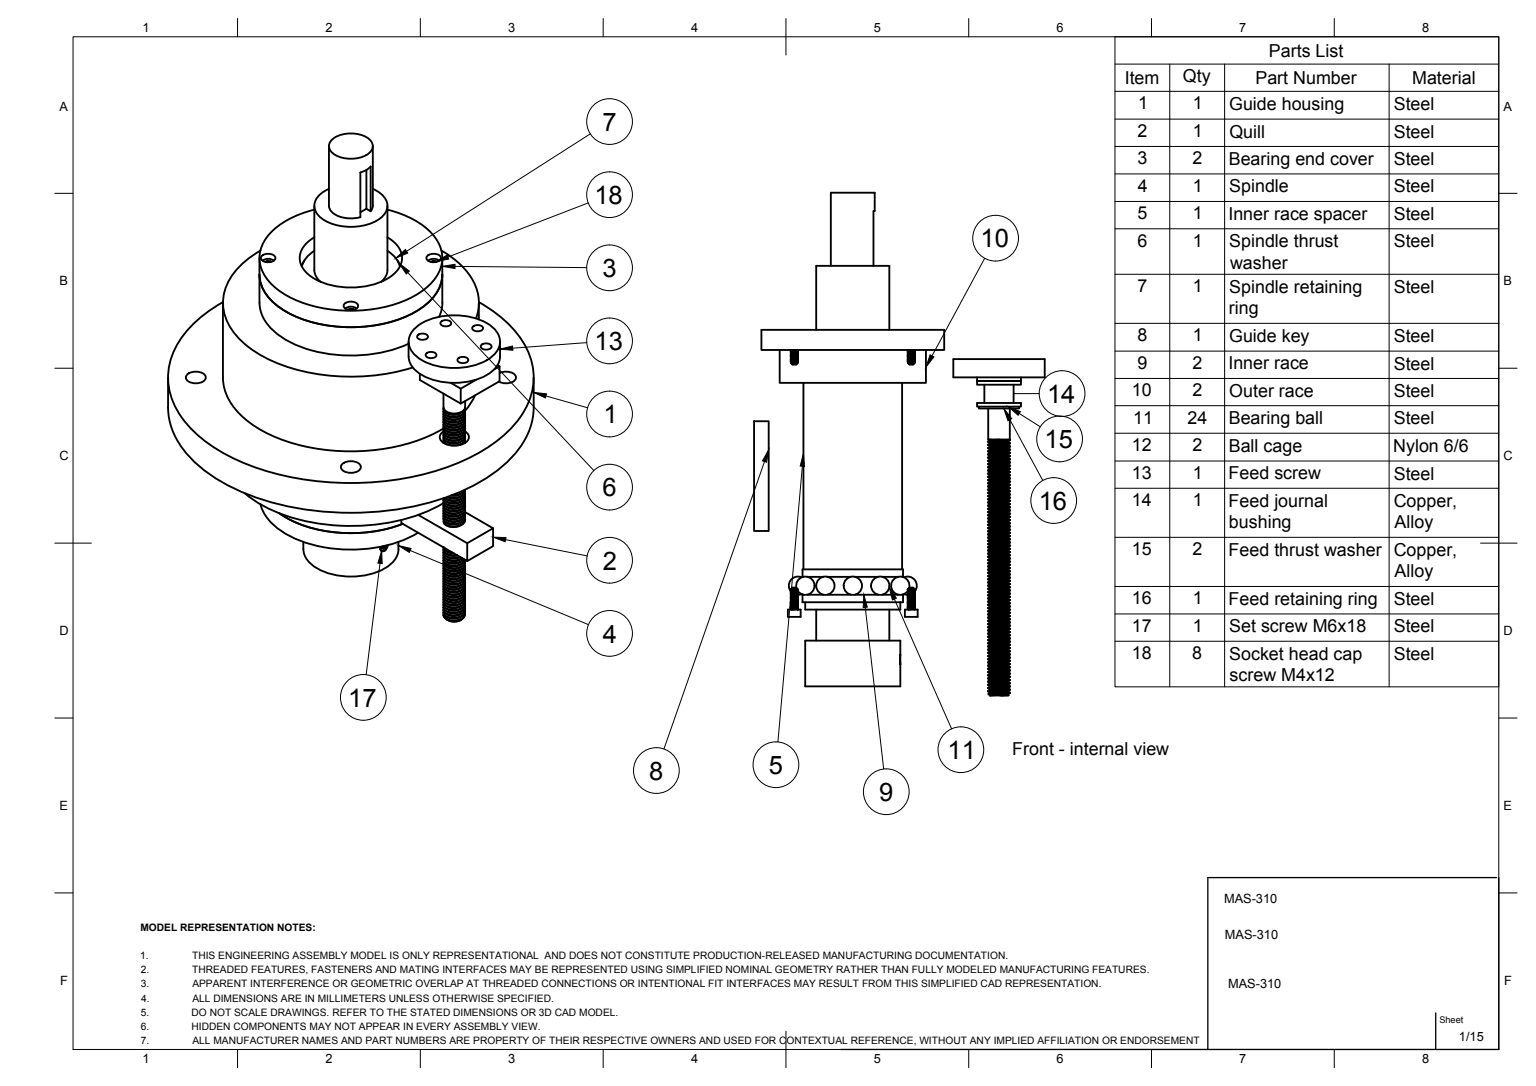
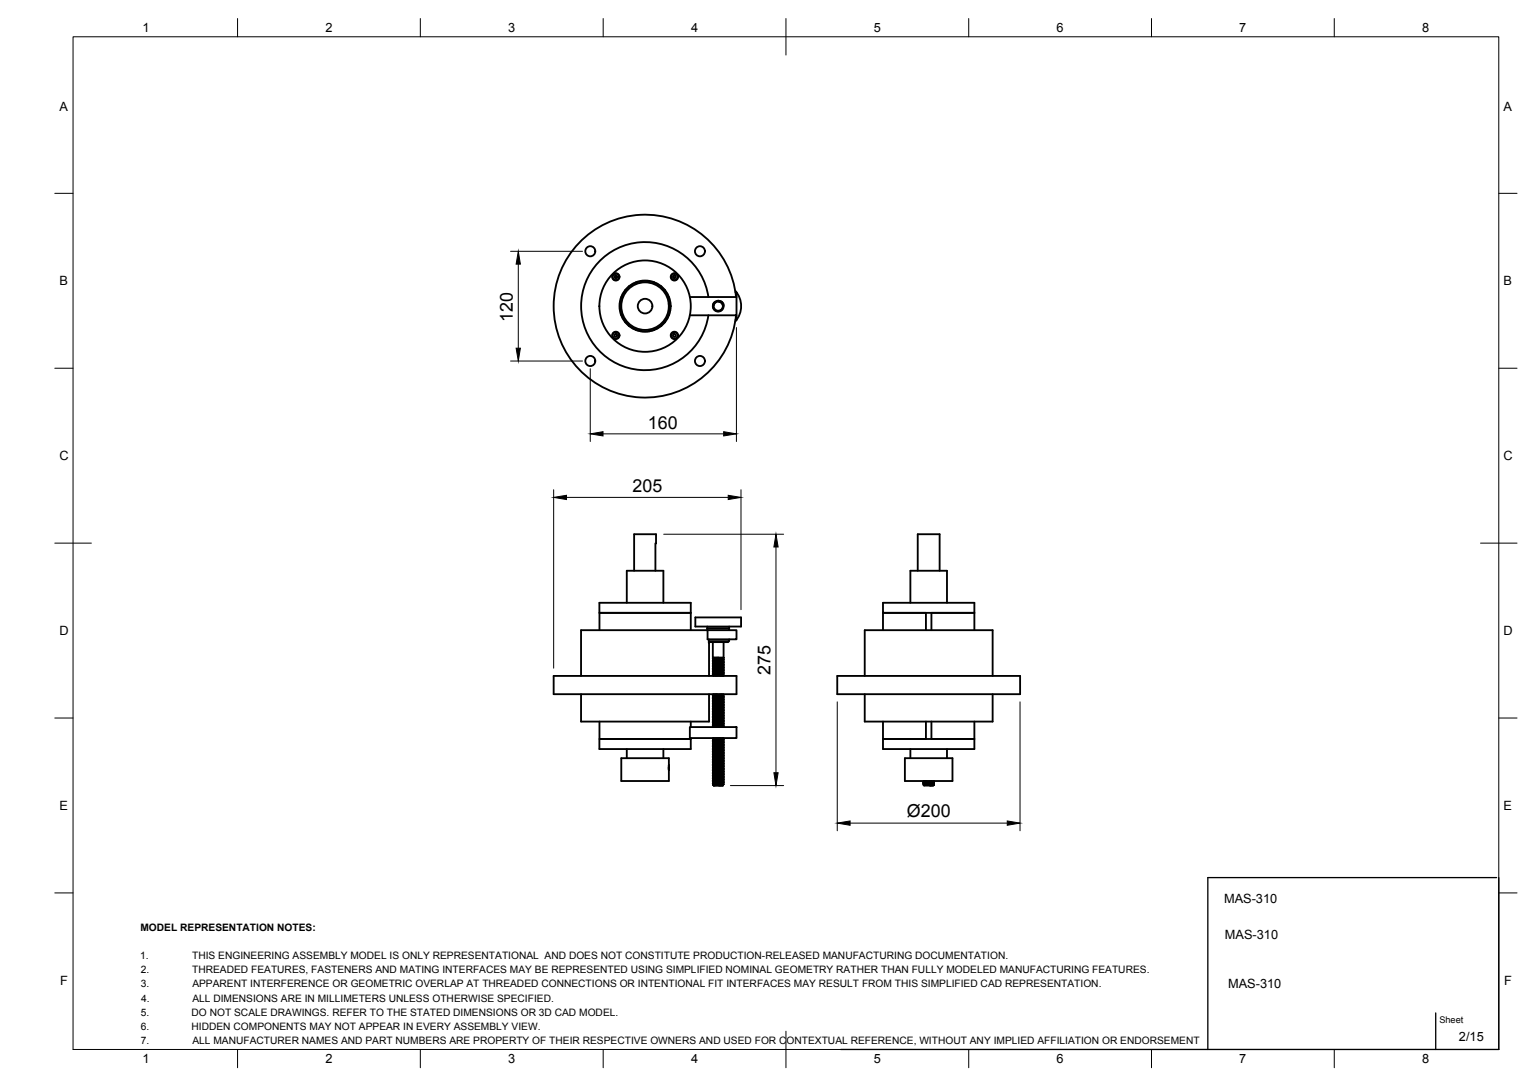
ISO-10303-21;
HEADER;
/* Generated by software containing ST-Developer
 * from STEP Tools, Inc. (www.steptools.com) 
 */

FILE_DESCRIPTION(
/* description */ ('Independent30mm screw-fed quill/spindle unit with16mm straight tool s
ocket, radial set screw, native reusable open ball bearings, retained 
inner/outer race stacks, keyed quill guide and M12x1.75 fine feed. Ext
ernal moving drive and tool not included. Ideal cage orbital links; in
dividual ball spin, force and preload not simulated. No drilling capac
ity, runout, speed, torque, load, life or machine safety rating.'),
/* implementation_level */ '2;1');

FILE_NAME(
/* name */ 'MAS-310.step',
/* time_stamp */ '2026-11-08T18:59:42-08:00',
/* author */ (''),
/* organization */ (''),
/* preprocessor_version */ 'ST-DEVELOPER v20.2',
/* originating_system */ 'Autodesk Translation Framework v15.17.0.0',
/* authorisation */ '');

FILE_SCHEMA (('AUTOMOTIVE_DESIGN { 1 0 10303 214 3 1 1 }'));
ENDSEC;

DATA;
#10=MECHANICAL_DESIGN_GEOMETRIC_PRESENTATION_REPRESENTATION('',(#1592,#1593,
#1594,#1595,#1596,#1597,#1598,#1599,#1600,#1601,#1602,#1603,#1604,#1605,
#1606,#1607,#1608,#1609),#63898);
#11=ITEM_DEFINED_TRANSFORMATION($,$,#15696,#16806);
#12=ITEM_DEFINED_TRANSFORMATION($,$,#15752,#16807);
#13=ITEM_DEFINED_TRANSFORMATION($,$,#16583,#16808);
#14=ITEM_DEFINED_TRANSFORMATION($,$,#16184,#16809);
#15=ITEM_DEFINED_TRANSFORMATION($,$,#16268,#16810);
#16=ITEM_DEFINED_TRANSFORMATION($,$,#16277,#16811);
#17=ITEM_DEFINED_TRANSFORMATION($,$,#16286,#16812);
#18=ITEM_DEFINED_TRANSFORMATION($,$,#16297,#16813);
#19=ITEM_DEFINED_TRANSFORMATION($,$,#16620,#16814);
#20=ITEM_DEFINED_TRANSFORMATION($,$,#16634,#16815);
#21=ITEM_DEFINED_TRANSFORMATION($,$,#16648,#16816);
#22=ITEM_DEFINED_TRANSFORMATION($,$,#16651,#16817);
#23=ITEM_DEFINED_TRANSFORMATION($,$,#16304,#16818);
#24=ITEM_DEFINED_TRANSFORMATION($,$,#16511,#16819);
#25=ITEM_DEFINED_TRANSFORMATION($,$,#16743,#16820);
#26=ITEM_DEFINED_TRANSFORMATION($,$,#16520,#16821);
#27=ITEM_DEFINED_TRANSFORMATION($,$,#16531,#16822);
#28=ITEM_DEFINED_TRANSFORMATION($,$,#16752,#16823);
#29=ITEM_DEFINED_TRANSFORMATION($,$,#16583,#16824);
#30=ITEM_DEFINED_TRANSFORMATION($,$,#16648,#16825);
#31=ITEM_DEFINED_TRANSFORMATION($,$,#16648,#16826);
#32=ITEM_DEFINED_TRANSFORMATION($,$,#16648,#16827);
#33=ITEM_DEFINED_TRANSFORMATION($,$,#16648,#16828);
#34=ITEM_DEFINED_TRANSFORMATION($,$,#16648,#16829);
#35=ITEM_DEFINED_TRANSFORMATION($,$,#16648,#16830);
#36=ITEM_DEFINED_TRANSFORMATION($,$,#16648,#16831);
#37=ITEM_DEFINED_TRANSFORMATION($,$,#16648,#16832);
#38=ITEM_DEFINED_TRANSFORMATION($,$,#16648,#16833);
#39=ITEM_DEFINED_TRANSFORMATION($,$,#16648,#16834);
#40=ITEM_DEFINED_TRANSFORMATION($,$,#16648,#16835);
#41=ITEM_DEFINED_TRANSFORMATION($,$,#16620,#16836);
#42=ITEM_DEFINED_TRANSFORMATION($,$,#16634,#16837);
#43=ITEM_DEFINED_TRANSFORMATION($,$,#16648,#16838);
#44=ITEM_DEFINED_TRANSFORMATION($,$,#16648,#16839);
#45=ITEM_DEFINED_TRANSFORMATION($,$,#16648,#16840);
#46=ITEM_DEFINED_TRANSFORMATION($,$,#16648,#16841);
#47=ITEM_DEFINED_TRANSFORMATION($,$,#16648,#16842);
#48=ITEM_DEFINED_TRANSFORMATION($,$,#16648,#16843);
#49=ITEM_DEFINED_TRANSFORMATION($,$,#16648,#16844);
#50=ITEM_DEFINED_TRANSFORMATION($,$,#16648,#16845);
#51=ITEM_DEFINED_TRANSFORMATION($,$,#16648,#16846);
#52=ITEM_DEFINED_TRANSFORMATION($,$,#16648,#16847);
#53=ITEM_DEFINED_TRANSFORMATION($,$,#16648,#16848);
#54=ITEM_DEFINED_TRANSFORMATION($,$,#16648,#16849);
#55=ITEM_DEFINED_TRANSFORMATION($,$,#16651,#16850);
#56=ITEM_DEFINED_TRANSFORMATION($,$,#16743,#16851);
#57=ITEM_DEFINED_TRANSFORMATION($,$,#16752,#16852);
#58=ITEM_DEFINED_TRANSFORMATION($,$,#16752,#16853);
#59=ITEM_DEFINED_TRANSFORMATION($,$,#16752,#16854);
#60=ITEM_DEFINED_TRANSFORMATION($,$,#16752,#16855);
#61=ITEM_DEFINED_TRANSFORMATION($,$,#16752,#16856);
#62=ITEM_DEFINED_TRANSFORMATION($,$,#16752,#16857);
#63=ITEM_DEFINED_TRANSFORMATION($,$,#16752,#16858);
#64=(
REPRESENTATION_RELATIONSHIP($,$,#63995,#63994)
REPRESENTATION_RELATIONSHIP_WITH_TRANSFORMATION(#11)
SHAPE_REPRESENTATION_RELATIONSHIP()
);
#65=(
REPRESENTATION_RELATIONSHIP($,$,#63996,#63994)
REPRESENTATION_RELATIONSHIP_WITH_TRANSFORMATION(#12)
SHAPE_REPRESENTATION_RELATIONSHIP()
);
#66=(
REPRESENTATION_RELATIONSHIP($,$,#64006,#63994)
REPRESENTATION_RELATIONSHIP_WITH_TRANSFORMATION(#13)
SHAPE_REPRESENTATION_RELATIONSHIP()
);
#67=(
REPRESENTATION_RELATIONSHIP($,$,#63997,#63994)
REPRESENTATION_RELATIONSHIP_WITH_TRANSFORMATION(#14)
SHAPE_REPRESENTATION_RELATIONSHIP()
);
#68=(
REPRESENTATION_RELATIONSHIP($,$,#63998,#63994)
REPRESENTATION_RELATIONSHIP_WITH_TRANSFORMATION(#15)
SHAPE_REPRESENTATION_RELATIONSHIP()
);
#69=(
REPRESENTATION_RELATIONSHIP($,$,#63999,#63994)
REPRESENTATION_RELATIONSHIP_WITH_TRANSFORMATION(#16)
SHAPE_REPRESENTATION_RELATIONSHIP()
);
#70=(
REPRESENTATION_RELATIONSHIP($,$,#64000,#63994)
REPRESENTATION_RELATIONSHIP_WITH_TRANSFORMATION(#17)
SHAPE_REPRESENTATION_RELATIONSHIP()
);
#71=(
REPRESENTATION_RELATIONSHIP($,$,#64001,#63994)
REPRESENTATION_RELATIONSHIP_WITH_TRANSFORMATION(#18)
SHAPE_REPRESENTATION_RELATIONSHIP()
);
#72=(
REPRESENTATION_RELATIONSHIP($,$,#64007,#63994)
REPRESENTATION_RELATIONSHIP_WITH_TRANSFORMATION(#19)
SHAPE_REPRESENTATION_RELATIONSHIP()
);
#73=(
REPRESENTATION_RELATIONSHIP($,$,#64008,#63994)
REPRESENTATION_RELATIONSHIP_WITH_TRANSFORMATION(#20)
SHAPE_REPRESENTATION_RELATIONSHIP()
);
#74=(
REPRESENTATION_RELATIONSHIP($,$,#64009,#63994)
REPRESENTATION_RELATIONSHIP_WITH_TRANSFORMATION(#21)
SHAPE_REPRESENTATION_RELATIONSHIP()
);
#75=(
REPRESENTATION_RELATIONSHIP($,$,#64010,#63994)
REPRESENTATION_RELATIONSHIP_WITH_TRANSFORMATION(#22)
SHAPE_REPRESENTATION_RELATIONSHIP()
);
#76=(
REPRESENTATION_RELATIONSHIP($,$,#64002,#63994)
REPRESENTATION_RELATIONSHIP_WITH_TRANSFORMATION(#23)
SHAPE_REPRESENTATION_RELATIONSHIP()
);
#77=(
REPRESENTATION_RELATIONSHIP($,$,#64003,#63994)
REPRESENTATION_RELATIONSHIP_WITH_TRANSFORMATION(#24)
SHAPE_REPRESENTATION_RELATIONSHIP()
);
#78=(
REPRESENTATION_RELATIONSHIP($,$,#64011,#63994)
REPRESENTATION_RELATIONSHIP_WITH_TRANSFORMATION(#25)
SHAPE_REPRESENTATION_RELATIONSHIP()
);
#79=(
REPRESENTATION_RELATIONSHIP($,$,#64004,#63994)
REPRESENTATION_RELATIONSHIP_WITH_TRANSFORMATION(#26)
SHAPE_REPRESENTATION_RELATIONSHIP()
);
#80=(
REPRESENTATION_RELATIONSHIP($,$,#64005,#63994)
REPRESENTATION_RELATIONSHIP_WITH_TRANSFORMATION(#27)
SHAPE_REPRESENTATION_RELATIONSHIP()
);
#81=(
REPRESENTATION_RELATIONSHIP($,$,#64012,#63994)
REPRESENTATION_RELATIONSHIP_WITH_TRANSFORMATION(#28)
SHAPE_REPRESENTATION_RELATIONSHIP()
);
#82=(
REPRESENTATION_RELATIONSHIP($,$,#64006,#63994)
REPRESENTATION_RELATIONSHIP_WITH_TRANSFORMATION(#29)
SHAPE_REPRESENTATION_RELATIONSHIP()
);
#83=(
REPRESENTATION_RELATIONSHIP($,$,#64009,#63994)
REPRESENTATION_RELATIONSHIP_WITH_TRANSFORMATION(#30)
SHAPE_REPRESENTATION_RELATIONSHIP()
);
#84=(
REPRESENTATION_RELATIONSHIP($,$,#64009,#63994)
REPRESENTATION_RELATIONSHIP_WITH_TRANSFORMATION(#31)
SHAPE_REPRESENTATION_RELATIONSHIP()
);
#85=(
REPRESENTATION_RELATIONSHIP($,$,#64009,#63994)
REPRESENTATION_RELATIONSHIP_WITH_TRANSFORMATION(#32)
SHAPE_REPRESENTATION_RELATIONSHIP()
);
#86=(
REPRESENTATION_RELATIONSHIP($,$,#64009,#63994)
REPRESENTATION_RELATIONSHIP_WITH_TRANSFORMATION(#33)
SHAPE_REPRESENTATION_RELATIONSHIP()
);
#87=(
REPRESENTATION_RELATIONSHIP($,$,#64009,#63994)
REPRESENTATION_RELATIONSHIP_WITH_TRANSFORMATION(#34)
SHAPE_REPRESENTATION_RELATIONSHIP()
);
#88=(
REPRESENTATION_RELATIONSHIP($,$,#64009,#63994)
REPRESENTATION_RELATIONSHIP_WITH_TRANSFORMATION(#35)
SHAPE_REPRESENTATION_RELATIONSHIP()
);
#89=(
REPRESENTATION_RELATIONSHIP($,$,#64009,#63994)
REPRESENTATION_RELATIONSHIP_WITH_TRANSFORMATION(#36)
SHAPE_REPRESENTATION_RELATIONSHIP()
);
#90=(
REPRESENTATION_RELATIONSHIP($,$,#64009,#63994)
REPRESENTATION_RELATIONSHIP_WITH_TRANSFORMATION(#37)
SHAPE_REPRESENTATION_RELATIONSHIP()
);
#91=(
REPRESENTATION_RELATIONSHIP($,$,#64009,#63994)
REPRESENTATION_RELATIONSHIP_WITH_TRANSFORMATION(#38)
SHAPE_REPRESENTATION_RELATIONSHIP()
);
#92=(
REPRESENTATION_RELATIONSHIP($,$,#64009,#63994)
REPRESENTATION_RELATIONSHIP_WITH_TRANSFORMATION(#39)
SHAPE_REPRESENTATION_RELATIONSHIP()
);
#93=(
REPRESENTATION_RELATIONSHIP($,$,#64009,#63994)
REPRESENTATION_RELATIONSHIP_WITH_TRANSFORMATION(#40)
SHAPE_REPRESENTATION_RELATIONSHIP()
);
#94=(
REPRESENTATION_RELATIONSHIP($,$,#64007,#63994)
REPRESENTATION_RELATIONSHIP_WITH_TRANSFORMATION(#41)
SHAPE_REPRESENTATION_RELATIONSHIP()
);
#95=(
REPRESENTATION_RELATIONSHIP($,$,#64008,#63994)
REPRESENTATION_RELATIONSHIP_WITH_TRANSFORMATION(#42)
SHAPE_REPRESENTATION_RELATIONSHIP()
);
#96=(
REPRESENTATION_RELATIONSHIP($,$,#64009,#63994)
REPRESENTATION_RELATIONSHIP_WITH_TRANSFORMATION(#43)
SHAPE_REPRESENTATION_RELATIONSHIP()
);
#97=(
REPRESENTATION_RELATIONSHIP($,$,#64009,#63994)
REPRESENTATION_RELATIONSHIP_WITH_TRANSFORMATION(#44)
SHAPE_REPRESENTATION_RELATIONSHIP()
);
#98=(
REPRESENTATION_RELATIONSHIP($,$,#64009,#63994)
REPRESENTATION_RELATIONSHIP_WITH_TRANSFORMATION(#45)
SHAPE_REPRESENTATION_RELATIONSHIP()
);
#99=(
REPRESENTATION_RELATIONSHIP($,$,#64009,#63994)
REPRESENTATION_RELATIONSHIP_WITH_TRANSFORMATION(#46)
SHAPE_REPRESENTATION_RELATIONSHIP()
);
#100=(
REPRESENTATION_RELATIONSHIP($,$,#64009,#63994)
REPRESENTATION_RELATIONSHIP_WITH_TRANSFORMATION(#47)
SHAPE_REPRESENTATION_RELATIONSHIP()
);
#101=(
REPRESENTATION_RELATIONSHIP($,$,#64009,#63994)
REPRESENTATION_RELATIONSHIP_WITH_TRANSFORMATION(#48)
SHAPE_REPRESENTATION_RELATIONSHIP()
);
#102=(
REPRESENTATION_RELATIONSHIP($,$,#64009,#63994)
REPRESENTATION_RELATIONSHIP_WITH_TRANSFORMATION(#49)
SHAPE_REPRESENTATION_RELATIONSHIP()
);
#103=(
REPRESENTATION_RELATIONSHIP($,$,#64009,#63994)
REPRESENTATION_RELATIONSHIP_WITH_TRANSFORMATION(#50)
SHAPE_REPRESENTATION_RELATIONSHIP()
);
#104=(
REPRESENTATION_RELATIONSHIP($,$,#64009,#63994)
REPRESENTATION_RELATIONSHIP_WITH_TRANSFORMATION(#51)
SHAPE_REPRESENTATION_RELATIONSHIP()
);
#105=(
REPRESENTATION_RELATIONSHIP($,$,#64009,#63994)
REPRESENTATION_RELATIONSHIP_WITH_TRANSFORMATION(#52)
SHAPE_REPRESENTATION_RELATIONSHIP()
);
#106=(
REPRESENTATION_RELATIONSHIP($,$,#64009,#63994)
REPRESENTATION_RELATIONSHIP_WITH_TRANSFORMATION(#53)
SHAPE_REPRESENTATION_RELATIONSHIP()
);
#107=(
REPRESENTATION_RELATIONSHIP($,$,#64009,#63994)
REPRESENTATION_RELATIONSHIP_WITH_TRANSFORMATION(#54)
SHAPE_REPRESENTATION_RELATIONSHIP()
);
#108=(
REPRESENTATION_RELATIONSHIP($,$,#64010,#63994)
REPRESENTATION_RELATIONSHIP_WITH_TRANSFORMATION(#55)
SHAPE_REPRESENTATION_RELATIONSHIP()
);
#109=(
REPRESENTATION_RELATIONSHIP($,$,#64011,#63994)
REPRESENTATION_RELATIONSHIP_WITH_TRANSFORMATION(#56)
SHAPE_REPRESENTATION_RELATIONSHIP()
);
#110=(
REPRESENTATION_RELATIONSHIP($,$,#64012,#63994)
REPRESENTATION_RELATIONSHIP_WITH_TRANSFORMATION(#57)
SHAPE_REPRESENTATION_RELATIONSHIP()
);
#111=(
REPRESENTATION_RELATIONSHIP($,$,#64012,#63994)
REPRESENTATION_RELATIONSHIP_WITH_TRANSFORMATION(#58)
SHAPE_REPRESENTATION_RELATIONSHIP()
);
#112=(
REPRESENTATION_RELATIONSHIP($,$,#64012,#63994)
REPRESENTATION_RELATIONSHIP_WITH_TRANSFORMATION(#59)
SHAPE_REPRESENTATION_RELATIONSHIP()
);
#113=(
REPRESENTATION_RELATIONSHIP($,$,#64012,#63994)
REPRESENTATION_RELATIONSHIP_WITH_TRANSFORMATION(#60)
SHAPE_REPRESENTATION_RELATIONSHIP()
);
#114=(
REPRESENTATION_RELATIONSHIP($,$,#64012,#63994)
REPRESENTATION_RELATIONSHIP_WITH_TRANSFORMATION(#61)
SHAPE_REPRESENTATION_RELATIONSHIP()
);
#115=(
REPRESENTATION_RELATIONSHIP($,$,#64012,#63994)
REPRESENTATION_RELATIONSHIP_WITH_TRANSFORMATION(#62)
SHAPE_REPRESENTATION_RELATIONSHIP()
);
#116=(
REPRESENTATION_RELATIONSHIP($,$,#64012,#63994)
REPRESENTATION_RELATIONSHIP_WITH_TRANSFORMATION(#63)
SHAPE_REPRESENTATION_RELATIONSHIP()
);
#117=CONTEXT_DEPENDENT_SHAPE_REPRESENTATION(#64,#63941);
#118=CONTEXT_DEPENDENT_SHAPE_REPRESENTATION(#65,#63942);
#119=CONTEXT_DEPENDENT_SHAPE_REPRESENTATION(#66,#63943);
#120=CONTEXT_DEPENDENT_SHAPE_REPRESENTATION(#67,#63944);
#121=CONTEXT_DEPENDENT_SHAPE_REPRESENTATION(#68,#63945);
#122=CONTEXT_DEPENDENT_SHAPE_REPRESENTATION(#69,#63946);
#123=CONTEXT_DEPENDENT_SHAPE_REPRESENTATION(#70,#63947);
#124=CONTEXT_DEPENDENT_SHAPE_REPRESENTATION(#71,#63948);
#125=CONTEXT_DEPENDENT_SHAPE_REPRESENTATION(#72,#63949);
#126=CONTEXT_DEPENDENT_SHAPE_REPRESENTATION(#73,#63950);
#127=CONTEXT_DEPENDENT_SHAPE_REPRESENTATION(#74,#63951);
#128=CONTEXT_DEPENDENT_SHAPE_REPRESENTATION(#75,#63952);
#129=CONTEXT_DEPENDENT_SHAPE_REPRESENTATION(#76,#63953);
#130=CONTEXT_DEPENDENT_SHAPE_REPRESENTATION(#77,#63954);
#131=CONTEXT_DEPENDENT_SHAPE_REPRESENTATION(#78,#63955);
#132=CONTEXT_DEPENDENT_SHAPE_REPRESENTATION(#79,#63956);
#133=CONTEXT_DEPENDENT_SHAPE_REPRESENTATION(#80,#63957);
#134=CONTEXT_DEPENDENT_SHAPE_REPRESENTATION(#81,#63958);
#135=CONTEXT_DEPENDENT_SHAPE_REPRESENTATION(#82,#63959);
#136=CONTEXT_DEPENDENT_SHAPE_REPRESENTATION(#83,#63960);
#137=CONTEXT_DEPENDENT_SHAPE_REPRESENTATION(#84,#63961);
#138=CONTEXT_DEPENDENT_SHAPE_REPRESENTATION(#85,#63962);
#139=CONTEXT_DEPENDENT_SHAPE_REPRESENTATION(#86,#63963);
#140=CONTEXT_DEPENDENT_SHAPE_REPRESENTATION(#87,#63964);
#141=CONTEXT_DEPENDENT_SHAPE_REPRESENTATION(#88,#63965);
#142=CONTEXT_DEPENDENT_SHAPE_REPRESENTATION(#89,#63966);
#143=CONTEXT_DEPENDENT_SHAPE_REPRESENTATION(#90,#63967);
#144=CONTEXT_DEPENDENT_SHAPE_REPRESENTATION(#91,#63968);
#145=CONTEXT_DEPENDENT_SHAPE_REPRESENTATION(#92,#63969);
#146=CONTEXT_DEPENDENT_SHAPE_REPRESENTATION(#93,#63970);
#147=CONTEXT_DEPENDENT_SHAPE_REPRESENTATION(#94,#63971);
#148=CONTEXT_DEPENDENT_SHAPE_REPRESENTATION(#95,#63972);
#149=CONTEXT_DEPENDENT_SHAPE_REPRESENTATION(#96,#63973);
#150=CONTEXT_DEPENDENT_SHAPE_REPRESENTATION(#97,#63974);
#151=CONTEXT_DEPENDENT_SHAPE_REPRESENTATION(#98,#63975);
#152=CONTEXT_DEPENDENT_SHAPE_REPRESENTATION(#99,#63976);
#153=CONTEXT_DEPENDENT_SHAPE_REPRESENTATION(#100,#63977);
#154=CONTEXT_DEPENDENT_SHAPE_REPRESENTATION(#101,#63978);
#155=CONTEXT_DEPENDENT_SHAPE_REPRESENTATION(#102,#63979);
#156=CONTEXT_DEPENDENT_SHAPE_REPRESENTATION(#103,#63980);
#157=CONTEXT_DEPENDENT_SHAPE_REPRESENTATION(#104,#63981);
#158=CONTEXT_DEPENDENT_SHAPE_REPRESENTATION(#105,#63982);
#159=CONTEXT_DEPENDENT_SHAPE_REPRESENTATION(#106,#63983);
#160=CONTEXT_DEPENDENT_SHAPE_REPRESENTATION(#107,#63984);
#161=CONTEXT_DEPENDENT_SHAPE_REPRESENTATION(#108,#63985);
#162=CONTEXT_DEPENDENT_SHAPE_REPRESENTATION(#109,#63986);
#163=CONTEXT_DEPENDENT_SHAPE_REPRESENTATION(#110,#63987);
#164=CONTEXT_DEPENDENT_SHAPE_REPRESENTATION(#111,#63988);
#165=CONTEXT_DEPENDENT_SHAPE_REPRESENTATION(#112,#63989);
#166=CONTEXT_DEPENDENT_SHAPE_REPRESENTATION(#113,#63990);
#167=CONTEXT_DEPENDENT_SHAPE_REPRESENTATION(#114,#63991);
#168=CONTEXT_DEPENDENT_SHAPE_REPRESENTATION(#115,#63992);
#169=CONTEXT_DEPENDENT_SHAPE_REPRESENTATION(#116,#63993);
#170=NEXT_ASSEMBLY_USAGE_OCCURRENCE('Guide housing:1','Guide housing:1',
'Guide housing:1',#64014,#64015,'Guide housing:1');
#171=NEXT_ASSEMBLY_USAGE_OCCURRENCE('Quill:1','Quill:1','Quill:1',#64014,
#64016,'Quill:1');
#172=NEXT_ASSEMBLY_USAGE_OCCURRENCE('Bearing end cover:1',
'Bearing end cover:1','Bearing end cover:1',#64014,#64026,
'Bearing end cover:1');
#173=NEXT_ASSEMBLY_USAGE_OCCURRENCE('Spindle:1','Spindle:1','Spindle:1',
#64014,#64017,'Spindle:1');
#174=NEXT_ASSEMBLY_USAGE_OCCURRENCE('Inner race spacer:1',
'Inner race spacer:1','Inner race spacer:1',#64014,#64018,
'Inner race spacer:1');
#175=NEXT_ASSEMBLY_USAGE_OCCURRENCE('Spindle thrust washer:1',
'Spindle thrust washer:1','Spindle thrust washer:1',#64014,#64019,
'Spindle thrust washer:1');
#176=NEXT_ASSEMBLY_USAGE_OCCURRENCE('Spindle retaining ring:1',
'Spindle retaining ring:1','Spindle retaining ring:1',#64014,#64020,
'Spindle retaining ring:1');
#177=NEXT_ASSEMBLY_USAGE_OCCURRENCE('Guide key:1','Guide key:1',
'Guide key:1',#64014,#64021,'Guide key:1');
#178=NEXT_ASSEMBLY_USAGE_OCCURRENCE('Inner race:1','Inner race:1',
'Inner race:1',#64014,#64027,'Inner race:1');
#179=NEXT_ASSEMBLY_USAGE_OCCURRENCE('Outer race:1','Outer race:1',
'Outer race:1',#64014,#64028,'Outer race:1');
#180=NEXT_ASSEMBLY_USAGE_OCCURRENCE('Bearing ball:1','Bearing ball:1',
'Bearing ball:1',#64014,#64029,'Bearing ball:1');
#181=NEXT_ASSEMBLY_USAGE_OCCURRENCE('Ball cage:1','Ball cage:1',
'Ball cage:1',#64014,#64030,'Ball cage:1');
#182=NEXT_ASSEMBLY_USAGE_OCCURRENCE('Feed screw:1','Feed screw:1',
'Feed screw:1',#64014,#64022,'Feed screw:1');
#183=NEXT_ASSEMBLY_USAGE_OCCURRENCE('Feed journal bushing:1',
'Feed journal bushing:1','Feed journal bushing:1',#64014,#64023,
'Feed journal bushing:1');
#184=NEXT_ASSEMBLY_USAGE_OCCURRENCE('Feed thrust washer:1',
'Feed thrust washer:1','Feed thrust washer:1',#64014,#64031,
'Feed thrust washer:1');
#185=NEXT_ASSEMBLY_USAGE_OCCURRENCE('Feed retaining ring:1',
'Feed retaining ring:1','Feed retaining ring:1',#64014,#64024,
'Feed retaining ring:1');
#186=NEXT_ASSEMBLY_USAGE_OCCURRENCE('Set screw M6x18:1',
'Set screw M6x18:1','Set screw M6x18:1',#64014,#64025,
'Set screw M6x18:1');
#187=NEXT_ASSEMBLY_USAGE_OCCURRENCE('Socket head cap screw M4x12:1',
'Socket head cap screw M4x12:1','Socket head cap screw M4x12:1',#64014,
#64032,'Socket head cap screw M4x12:1');
#188=NEXT_ASSEMBLY_USAGE_OCCURRENCE('Bearing end cover:2',
'Bearing end cover:2','Bearing end cover:2',#64014,#64026,
'Bearing end cover:2');
#189=NEXT_ASSEMBLY_USAGE_OCCURRENCE('Bearing ball:2','Bearing ball:2',
'Bearing ball:2',#64014,#64029,'Bearing ball:2');
#190=NEXT_ASSEMBLY_USAGE_OCCURRENCE('Bearing ball:3','Bearing ball:3',
'Bearing ball:3',#64014,#64029,'Bearing ball:3');
#191=NEXT_ASSEMBLY_USAGE_OCCURRENCE('Bearing ball:4','Bearing ball:4',
'Bearing ball:4',#64014,#64029,'Bearing ball:4');
#192=NEXT_ASSEMBLY_USAGE_OCCURRENCE('Bearing ball:5','Bearing ball:5',
'Bearing ball:5',#64014,#64029,'Bearing ball:5');
#193=NEXT_ASSEMBLY_USAGE_OCCURRENCE('Bearing ball:6','Bearing ball:6',
'Bearing ball:6',#64014,#64029,'Bearing ball:6');
#194=NEXT_ASSEMBLY_USAGE_OCCURRENCE('Bearing ball:7','Bearing ball:7',
'Bearing ball:7',#64014,#64029,'Bearing ball:7');
#195=NEXT_ASSEMBLY_USAGE_OCCURRENCE('Bearing ball:8','Bearing ball:8',
'Bearing ball:8',#64014,#64029,'Bearing ball:8');
#196=NEXT_ASSEMBLY_USAGE_OCCURRENCE('Bearing ball:9','Bearing ball:9',
'Bearing ball:9',#64014,#64029,'Bearing ball:9');
#197=NEXT_ASSEMBLY_USAGE_OCCURRENCE('Bearing ball:10','Bearing ball:10',
'Bearing ball:10',#64014,#64029,'Bearing ball:10');
#198=NEXT_ASSEMBLY_USAGE_OCCURRENCE('Bearing ball:11','Bearing ball:11',
'Bearing ball:11',#64014,#64029,'Bearing ball:11');
#199=NEXT_ASSEMBLY_USAGE_OCCURRENCE('Bearing ball:12','Bearing ball:12',
'Bearing ball:12',#64014,#64029,'Bearing ball:12');
#200=NEXT_ASSEMBLY_USAGE_OCCURRENCE('Inner race:2','Inner race:2',
'Inner race:2',#64014,#64027,'Inner race:2');
#201=NEXT_ASSEMBLY_USAGE_OCCURRENCE('Outer race:2','Outer race:2',
'Outer race:2',#64014,#64028,'Outer race:2');
#202=NEXT_ASSEMBLY_USAGE_OCCURRENCE('Bearing ball:13','Bearing ball:13',
'Bearing ball:13',#64014,#64029,'Bearing ball:13');
#203=NEXT_ASSEMBLY_USAGE_OCCURRENCE('Bearing ball:14','Bearing ball:14',
'Bearing ball:14',#64014,#64029,'Bearing ball:14');
#204=NEXT_ASSEMBLY_USAGE_OCCURRENCE('Bearing ball:15','Bearing ball:15',
'Bearing ball:15',#64014,#64029,'Bearing ball:15');
#205=NEXT_ASSEMBLY_USAGE_OCCURRENCE('Bearing ball:16','Bearing ball:16',
'Bearing ball:16',#64014,#64029,'Bearing ball:16');
#206=NEXT_ASSEMBLY_USAGE_OCCURRENCE('Bearing ball:17','Bearing ball:17',
'Bearing ball:17',#64014,#64029,'Bearing ball:17');
#207=NEXT_ASSEMBLY_USAGE_OCCURRENCE('Bearing ball:18','Bearing ball:18',
'Bearing ball:18',#64014,#64029,'Bearing ball:18');
#208=NEXT_ASSEMBLY_USAGE_OCCURRENCE('Bearing ball:19','Bearing ball:19',
'Bearing ball:19',#64014,#64029,'Bearing ball:19');
#209=NEXT_ASSEMBLY_USAGE_OCCURRENCE('Bearing ball:20','Bearing ball:20',
'Bearing ball:20',#64014,#64029,'Bearing ball:20');
#210=NEXT_ASSEMBLY_USAGE_OCCURRENCE('Bearing ball:21','Bearing ball:21',
'Bearing ball:21',#64014,#64029,'Bearing ball:21');
#211=NEXT_ASSEMBLY_USAGE_OCCURRENCE('Bearing ball:22','Bearing ball:22',
'Bearing ball:22',#64014,#64029,'Bearing ball:22');
#212=NEXT_ASSEMBLY_USAGE_OCCURRENCE('Bearing ball:23','Bearing ball:23',
'Bearing ball:23',#64014,#64029,'Bearing ball:23');
#213=NEXT_ASSEMBLY_USAGE_OCCURRENCE('Bearing ball:24','Bearing ball:24',
'Bearing ball:24',#64014,#64029,'Bearing ball:24');
#214=NEXT_ASSEMBLY_USAGE_OCCURRENCE('Ball cage:2','Ball cage:2',
'Ball cage:2',#64014,#64030,'Ball cage:2');
#215=NEXT_ASSEMBLY_USAGE_OCCURRENCE('Feed thrust washer:2',
'Feed thrust washer:2','Feed thrust washer:2',#64014,#64031,
'Feed thrust washer:2');
#216=NEXT_ASSEMBLY_USAGE_OCCURRENCE('Socket head cap screw M4x12:2',
'Socket head cap screw M4x12:2','Socket head cap screw M4x12:2',#64014,
#64032,'Socket head cap screw M4x12:2');
#217=NEXT_ASSEMBLY_USAGE_OCCURRENCE('Socket head cap screw M4x12:3',
'Socket head cap screw M4x12:3','Socket head cap screw M4x12:3',#64014,
#64032,'Socket head cap screw M4x12:3');
#218=NEXT_ASSEMBLY_USAGE_OCCURRENCE('Socket head cap screw M4x12:4',
'Socket head cap screw M4x12:4','Socket head cap screw M4x12:4',#64014,
#64032,'Socket head cap screw M4x12:4');
#219=NEXT_ASSEMBLY_USAGE_OCCURRENCE('Socket head cap screw M4x12:5',
'Socket head cap screw M4x12:5','Socket head cap screw M4x12:5',#64014,
#64032,'Socket head cap screw M4x12:5');
#220=NEXT_ASSEMBLY_USAGE_OCCURRENCE('Socket head cap screw M4x12:6',
'Socket head cap screw M4x12:6','Socket head cap screw M4x12:6',#64014,
#64032,'Socket head cap screw M4x12:6');
#221=NEXT_ASSEMBLY_USAGE_OCCURRENCE('Socket head cap screw M4x12:7',
'Socket head cap screw M4x12:7','Socket head cap screw M4x12:7',#64014,
#64032,'Socket head cap screw M4x12:7');
#222=NEXT_ASSEMBLY_USAGE_OCCURRENCE('Socket head cap screw M4x12:8',
'Socket head cap screw M4x12:8','Socket head cap screw M4x12:8',#64014,
#64032,'Socket head cap screw M4x12:8');
#223=SPHERICAL_SURFACE('',#16649,5.);
#224=SPHERICAL_SURFACE('',#16652,6.);
#225=SPHERICAL_SURFACE('',#16673,6.);
#226=SPHERICAL_SURFACE('',#16679,6.);
#227=SPHERICAL_SURFACE('',#16686,6.);
#228=SPHERICAL_SURFACE('',#16692,6.);
#229=SPHERICAL_SURFACE('',#16698,6.);
#230=SPHERICAL_SURFACE('',#16704,6.);
#231=SPHERICAL_SURFACE('',#16710,6.);
#232=SPHERICAL_SURFACE('',#16717,6.);
#233=SPHERICAL_SURFACE('',#16723,6.);
#234=SPHERICAL_SURFACE('',#16729,6.);
#235=SPHERICAL_SURFACE('',#16735,6.);
#236=TOROIDAL_SURFACE('',#16621,31.,6.);
#237=TOROIDAL_SURFACE('',#16635,29.,6.);
#238=CONICAL_SURFACE('',#16469,5.5,0.785398163397448);
#239=CONICAL_SURFACE('',#16787,1.5,0.785398163397449);
#240=B_SPLINE_SURFACE_WITH_KNOTS('',3,3,((#31744,#31745,#31746,#31747,#31748,
#31749,#31750,#31751,#31752,#31753,#31754,#31755,#31756,#31757,#31758,#31759,
#31760,#31761,#31762,#31763,#31764,#31765,#31766,#31767,#31768,#31769,#31770,
#31771,#31772,#31773,#31774,#31775,#31776,#31777,#31778,#31779,#31780,#31781,
#31782,#31783,#31784,#31785,#31786,#31787,#31788,#31789,#31790,#31791,#31792,
#31793,#31794,#31795,#31796,#31797,#31798,#31799,#31800,#31801,#31802,#31803,
#31804,#31805,#31806,#31807,#31808,#31809,#31810,#31811,#31812,#31813,#31814,
#31815,#31816,#31817,#31818,#31819,#31820,#31821,#31822,#31823,#31824,#31825,
#31826,#31827,#31828,#31829,#31830,#31831,#31832,#31833,#31834,#31835,#31836,
#31837,#31838,#31839,#31840,#31841,#31842,#31843,#31844,#31845,#31846,#31847,
#31848,#31849,#31850,#31851,#31852,#31853,#31854,#31855,#31856,#31857,#31858,
#31859,#31860,#31861,#31862,#31863,#31864,#31865),(#31866,#31867,#31868,
#31869,#31870,#31871,#31872,#31873,#31874,#31875,#31876,#31877,#31878,#31879,
#31880,#31881,#31882,#31883,#31884,#31885,#31886,#31887,#31888,#31889,#31890,
#31891,#31892,#31893,#31894,#31895,#31896,#31897,#31898,#31899,#31900,#31901,
#31902,#31903,#31904,#31905,#31906,#31907,#31908,#31909,#31910,#31911,#31912,
#31913,#31914,#31915,#31916,#31917,#31918,#31919,#31920,#31921,#31922,#31923,
#31924,#31925,#31926,#31927,#31928,#31929,#31930,#31931,#31932,#31933,#31934,
#31935,#31936,#31937,#31938,#31939,#31940,#31941,#31942,#31943,#31944,#31945,
#31946,#31947,#31948,#31949,#31950,#31951,#31952,#31953,#31954,#31955,#31956,
#31957,#31958,#31959,#31960,#31961,#31962,#31963,#31964,#31965,#31966,#31967,
#31968,#31969,#31970,#31971,#31972,#31973,#31974,#31975,#31976,#31977,#31978,
#31979,#31980,#31981,#31982,#31983,#31984,#31985,#31986,#31987),(#31988,
#31989,#31990,#31991,#31992,#31993,#31994,#31995,#31996,#31997,#31998,#31999,
#32000,#32001,#32002,#32003,#32004,#32005,#32006,#32007,#32008,#32009,#32010,
#32011,#32012,#32013,#32014,#32015,#32016,#32017,#32018,#32019,#32020,#32021,
#32022,#32023,#32024,#32025,#32026,#32027,#32028,#32029,#32030,#32031,#32032,
#32033,#32034,#32035,#32036,#32037,#32038,#32039,#32040,#32041,#32042,#32043,
#32044,#32045,#32046,#32047,#32048,#32049,#32050,#32051,#32052,#32053,#32054,
#32055,#32056,#32057,#32058,#32059,#32060,#32061,#32062,#32063,#32064,#32065,
#32066,#32067,#32068,#32069,#32070,#32071,#32072,#32073,#32074,#32075,#32076,
#32077,#32078,#32079,#32080,#32081,#32082,#32083,#32084,#32085,#32086,#32087,
#32088,#32089,#32090,#32091,#32092,#32093,#32094,#32095,#32096,#32097,#32098,
#32099,#32100,#32101,#32102,#32103,#32104,#32105,#32106,#32107,#32108,#32109),
(#32110,#32111,#32112,#32113,#32114,#32115,#32116,#32117,#32118,#32119,
#32120,#32121,#32122,#32123,#32124,#32125,#32126,#32127,#32128,#32129,#32130,
#32131,#32132,#32133,#32134,#32135,#32136,#32137,#32138,#32139,#32140,#32141,
#32142,#32143,#32144,#32145,#32146,#32147,#32148,#32149,#32150,#32151,#32152,
#32153,#32154,#32155,#32156,#32157,#32158,#32159,#32160,#32161,#32162,#32163,
#32164,#32165,#32166,#32167,#32168,#32169,#32170,#32171,#32172,#32173,#32174,
#32175,#32176,#32177,#32178,#32179,#32180,#32181,#32182,#32183,#32184,#32185,
#32186,#32187,#32188,#32189,#32190,#32191,#32192,#32193,#32194,#32195,#32196,
#32197,#32198,#32199,#32200,#32201,#32202,#32203,#32204,#32205,#32206,#32207,
#32208,#32209,#32210,#32211,#32212,#32213,#32214,#32215,#32216,#32217,#32218,
#32219,#32220,#32221,#32222,#32223,#32224,#32225,#32226,#32227,#32228,#32229,
#32230,#32231)),.UNSPECIFIED.,.F.,.F.,.F.,(4,4),(4,1,1,1,1,1,1,1,1,1,1,
1,1,1,1,1,1,1,1,1,1,1,1,1,1,1,1,1,1,1,1,1,1,1,1,1,1,1,1,1,1,1,1,1,1,1,1,
1,1,1,1,1,1,1,1,1,1,1,1,1,1,1,1,1,1,1,1,1,1,1,1,1,1,1,1,1,1,1,1,1,1,1,1,
1,1,1,1,1,1,1,1,1,1,1,1,1,1,1,1,1,1,1,1,1,1,1,1,1,1,1,1,1,1,1,1,1,1,1,1,
4),(0.,0.0448889834294937),(11.8615800042573,12.8590786597078,13.8565773151583,
14.8540759706088,15.8515746260593,16.8490732815098,17.8465719369603,18.8440705924108,
19.8415692478613,20.8390679033118,21.8365665587623,22.8340652142128,23.8315638696633,
24.8290625251138,25.8265611805643,26.8240598360148,27.8215584914653,28.8190571469158,
29.8165558023663,30.8140544578168,31.8115531132673,32.8090517687178,33.8065504241683,
34.8040490796188,35.8015477350693,36.7990463905198,37.7965450459703,38.7940437014208,
39.7915423568713,40.7890410123218,41.7865396677723,42.7840383232228,43.7815369786733,
44.7790356341238,45.7765342895743,46.7740329450248,47.7715316004753,48.7690302559258,
49.7665289113763,50.7640275668268,51.7615262222773,52.7590248777278,53.7565235331783,
54.7540221886288,55.7515208440793,56.7490194995298,57.7465181549803,58.7440168104308,
59.7415154658813,60.7390141213318,61.7365127767823,62.7340114322328,63.7315100876833,
64.7290087431338,65.7265073985843,66.7240060540348,67.7215047094853,68.7190033649358,
69.7165020203863,70.7140006758368,71.7114993312873,72.7089979867378,73.7064966421883,
74.7039952976388,75.7014939530893,76.6989926085398,77.6964912639903,78.6939899194408,
79.6914885748913,80.6889872303418,81.6864858857923,82.6839845412428,83.6814831966933,
84.6789818521438,85.6764805075943,86.6739791630448,87.6714778184953,88.6689764739458,
89.6664751293963,90.6639737848468,91.6614724402973,92.6589710957478,93.6564697511983,
94.6539684066488,95.6514670620993,96.6489657175498,97.6464643730003,98.6439630284508,
99.6414616839013,100.638960339352,101.636458994802,102.633957650253,103.631456305703,
104.628954961154,105.626453616604,106.623952272055,107.621450927505,108.618949582956,
109.616448238406,110.613946893857,111.611445549307,112.608944204758,113.606442860208,
114.603941515659,115.601440171109,116.59893882656,117.59643748201,118.593936137461,
119.591434792911,120.588933448362,121.586432103812,122.583930759263,123.581429414713,
124.578928070164,125.576426725614,126.573925381065,127.571424036515,128.568922691966,
129.566421347416,130.563920002867),.UNSPECIFIED.);
#241=B_SPLINE_SURFACE_WITH_KNOTS('',3,3,((#32339,#32340,#32341,#32342,#32343,
#32344,#32345,#32346,#32347,#32348,#32349,#32350,#32351,#32352,#32353,#32354,
#32355,#32356,#32357,#32358,#32359,#32360,#32361,#32362,#32363,#32364,#32365,
#32366,#32367,#32368,#32369,#32370,#32371,#32372,#32373,#32374,#32375,#32376,
#32377,#32378,#32379,#32380,#32381,#32382,#32383,#32384,#32385,#32386,#32387,
#32388,#32389,#32390,#32391,#32392,#32393,#32394,#32395,#32396,#32397,#32398,
#32399,#32400,#32401,#32402,#32403,#32404,#32405,#32406,#32407,#32408,#32409,
#32410,#32411,#32412,#32413,#32414,#32415,#32416,#32417,#32418,#32419,#32420,
#32421,#32422,#32423,#32424,#32425,#32426,#32427,#32428,#32429,#32430,#32431,
#32432,#32433,#32434,#32435,#32436,#32437,#32438,#32439,#32440,#32441,#32442,
#32443,#32444,#32445,#32446,#32447,#32448,#32449,#32450,#32451,#32452,#32453,
#32454,#32455,#32456,#32457,#32458,#32459,#32460),(#32461,#32462,#32463,
#32464,#32465,#32466,#32467,#32468,#32469,#32470,#32471,#32472,#32473,#32474,
#32475,#32476,#32477,#32478,#32479,#32480,#32481,#32482,#32483,#32484,#32485,
#32486,#32487,#32488,#32489,#32490,#32491,#32492,#32493,#32494,#32495,#32496,
#32497,#32498,#32499,#32500,#32501,#32502,#32503,#32504,#32505,#32506,#32507,
#32508,#32509,#32510,#32511,#32512,#32513,#32514,#32515,#32516,#32517,#32518,
#32519,#32520,#32521,#32522,#32523,#32524,#32525,#32526,#32527,#32528,#32529,
#32530,#32531,#32532,#32533,#32534,#32535,#32536,#32537,#32538,#32539,#32540,
#32541,#32542,#32543,#32544,#32545,#32546,#32547,#32548,#32549,#32550,#32551,
#32552,#32553,#32554,#32555,#32556,#32557,#32558,#32559,#32560,#32561,#32562,
#32563,#32564,#32565,#32566,#32567,#32568,#32569,#32570,#32571,#32572,#32573,
#32574,#32575,#32576,#32577,#32578,#32579,#32580,#32581,#32582),(#32583,
#32584,#32585,#32586,#32587,#32588,#32589,#32590,#32591,#32592,#32593,#32594,
#32595,#32596,#32597,#32598,#32599,#32600,#32601,#32602,#32603,#32604,#32605,
#32606,#32607,#32608,#32609,#32610,#32611,#32612,#32613,#32614,#32615,#32616,
#32617,#32618,#32619,#32620,#32621,#32622,#32623,#32624,#32625,#32626,#32627,
#32628,#32629,#32630,#32631,#32632,#32633,#32634,#32635,#32636,#32637,#32638,
#32639,#32640,#32641,#32642,#32643,#32644,#32645,#32646,#32647,#32648,#32649,
#32650,#32651,#32652,#32653,#32654,#32655,#32656,#32657,#32658,#32659,#32660,
#32661,#32662,#32663,#32664,#32665,#32666,#32667,#32668,#32669,#32670,#32671,
#32672,#32673,#32674,#32675,#32676,#32677,#32678,#32679,#32680,#32681,#32682,
#32683,#32684,#32685,#32686,#32687,#32688,#32689,#32690,#32691,#32692,#32693,
#32694,#32695,#32696,#32697,#32698,#32699,#32700,#32701,#32702,#32703,#32704),
(#32705,#32706,#32707,#32708,#32709,#32710,#32711,#32712,#32713,#32714,
#32715,#32716,#32717,#32718,#32719,#32720,#32721,#32722,#32723,#32724,#32725,
#32726,#32727,#32728,#32729,#32730,#32731,#32732,#32733,#32734,#32735,#32736,
#32737,#32738,#32739,#32740,#32741,#32742,#32743,#32744,#32745,#32746,#32747,
#32748,#32749,#32750,#32751,#32752,#32753,#32754,#32755,#32756,#32757,#32758,
#32759,#32760,#32761,#32762,#32763,#32764,#32765,#32766,#32767,#32768,#32769,
#32770,#32771,#32772,#32773,#32774,#32775,#32776,#32777,#32778,#32779,#32780,
#32781,#32782,#32783,#32784,#32785,#32786,#32787,#32788,#32789,#32790,#32791,
#32792,#32793,#32794,#32795,#32796,#32797,#32798,#32799,#32800,#32801,#32802,
#32803,#32804,#32805,#32806,#32807,#32808,#32809,#32810,#32811,#32812,#32813,
#32814,#32815,#32816,#32817,#32818,#32819,#32820,#32821,#32822,#32823,#32824,
#32825,#32826)),.UNSPECIFIED.,.F.,.F.,.F.,(4,4),(4,1,1,1,1,1,1,1,1,1,1,
1,1,1,1,1,1,1,1,1,1,1,1,1,1,1,1,1,1,1,1,1,1,1,1,1,1,1,1,1,1,1,1,1,1,1,1,
1,1,1,1,1,1,1,1,1,1,1,1,1,1,1,1,1,1,1,1,1,1,1,1,1,1,1,1,1,1,1,1,1,1,1,1,
1,1,1,1,1,1,1,1,1,1,1,1,1,1,1,1,1,1,1,1,1,1,1,1,1,1,1,1,1,1,1,1,1,1,1,1,
4),(0.,0.0448889834294937),(14.3981410127776,15.3956396682281,16.3931383236786,
17.3906369791291,18.3881356345796,19.3856342900301,20.3831329454806,21.3806316009311,
22.3781302563816,23.3756289118321,24.3731275672826,25.3706262227331,26.3681248781836,
27.3656235336341,28.3631221890846,29.3606208445351,30.3581194999856,31.3556181554361,
32.3531168108866,33.3506154663371,34.3481141217876,35.3456127772381,36.3431114326886,
37.3406100881391,38.3381087435896,39.3356073990401,40.3331060544906,41.3306047099411,
42.3281033653916,43.3256020208421,44.3231006762926,45.3205993317431,46.3180979871936,
47.3155966426441,48.3130952980946,49.3105939535451,50.3080926089956,51.3055912644461,
52.3030899198966,53.3005885753471,54.2980872307976,55.2955858862481,56.2930845416986,
57.2905831971491,58.2880818525996,59.2855805080501,60.2830791635006,61.2805778189511,
62.2780764744016,63.2755751298521,64.2730737853026,65.2705724407531,66.2680710962036,
67.2655697516541,68.2630684071046,69.2605670625551,70.2580657180056,71.2555643734561,
72.2530630289066,73.2505616843571,74.2480603398076,75.2455589952581,76.2430576507086,
77.2405563061591,78.2380549616096,79.2355536170601,80.2330522725106,81.2305509279611,
82.2280495834116,83.2255482388621,84.2230468943126,85.2205455497631,86.2180442052136,
87.2155428606641,88.2130415161146,89.2105401715651,90.2080388270156,91.2055374824661,
92.2030361379166,93.2005347933671,94.1980334488176,95.1955321042681,96.1930307597186,
97.1905294151691,98.1880280706196,99.1855267260701,100.183025381521,101.180524036971,
102.178022692422,103.175521347872,104.173020003323,105.170518658773,106.168017314224,
107.165515969674,108.163014625125,109.160513280575,110.158011936026,111.155510591476,
112.153009246927,113.150507902377,114.148006557828,115.145505213278,116.143003868729,
117.140502524179,118.13800117963,119.13549983508,120.132998490531,121.130497145981,
122.127995801432,123.125494456882,124.122993112333,125.120491767783,126.117990423234,
127.115489078684,128.112987734135,129.110486389585,130.107985045036,131.105483700486,
132.102982355937,133.100481011387),.UNSPECIFIED.);
#242=B_SPLINE_SURFACE_WITH_KNOTS('',3,3,((#33131,#33132,#33133,#33134,#33135,
#33136,#33137,#33138,#33139,#33140,#33141,#33142,#33143,#33144,#33145,#33146,
#33147,#33148,#33149,#33150,#33151,#33152,#33153,#33154,#33155,#33156,#33157,
#33158,#33159,#33160,#33161,#33162,#33163,#33164,#33165,#33166,#33167,#33168,
#33169,#33170,#33171,#33172,#33173,#33174,#33175,#33176,#33177,#33178,#33179,
#33180,#33181,#33182,#33183,#33184,#33185,#33186,#33187,#33188,#33189,#33190,
#33191,#33192,#33193,#33194,#33195,#33196,#33197,#33198,#33199,#33200,#33201,
#33202,#33203,#33204,#33205,#33206,#33207,#33208,#33209,#33210,#33211,#33212,
#33213,#33214,#33215,#33216,#33217,#33218,#33219,#33220,#33221,#33222,#33223,
#33224,#33225,#33226,#33227,#33228,#33229,#33230,#33231,#33232,#33233,#33234,
#33235,#33236,#33237,#33238,#33239,#33240,#33241,#33242,#33243,#33244,#33245,
#33246,#33247,#33248,#33249,#33250,#33251,#33252),(#33253,#33254,#33255,
#33256,#33257,#33258,#33259,#33260,#33261,#33262,#33263,#33264,#33265,#33266,
#33267,#33268,#33269,#33270,#33271,#33272,#33273,#33274,#33275,#33276,#33277,
#33278,#33279,#33280,#33281,#33282,#33283,#33284,#33285,#33286,#33287,#33288,
#33289,#33290,#33291,#33292,#33293,#33294,#33295,#33296,#33297,#33298,#33299,
#33300,#33301,#33302,#33303,#33304,#33305,#33306,#33307,#33308,#33309,#33310,
#33311,#33312,#33313,#33314,#33315,#33316,#33317,#33318,#33319,#33320,#33321,
#33322,#33323,#33324,#33325,#33326,#33327,#33328,#33329,#33330,#33331,#33332,
#33333,#33334,#33335,#33336,#33337,#33338,#33339,#33340,#33341,#33342,#33343,
#33344,#33345,#33346,#33347,#33348,#33349,#33350,#33351,#33352,#33353,#33354,
#33355,#33356,#33357,#33358,#33359,#33360,#33361,#33362,#33363,#33364,#33365,
#33366,#33367,#33368,#33369,#33370,#33371,#33372,#33373,#33374),(#33375,
#33376,#33377,#33378,#33379,#33380,#33381,#33382,#33383,#33384,#33385,#33386,
#33387,#33388,#33389,#33390,#33391,#33392,#33393,#33394,#33395,#33396,#33397,
#33398,#33399,#33400,#33401,#33402,#33403,#33404,#33405,#33406,#33407,#33408,
#33409,#33410,#33411,#33412,#33413,#33414,#33415,#33416,#33417,#33418,#33419,
#33420,#33421,#33422,#33423,#33424,#33425,#33426,#33427,#33428,#33429,#33430,
#33431,#33432,#33433,#33434,#33435,#33436,#33437,#33438,#33439,#33440,#33441,
#33442,#33443,#33444,#33445,#33446,#33447,#33448,#33449,#33450,#33451,#33452,
#33453,#33454,#33455,#33456,#33457,#33458,#33459,#33460,#33461,#33462,#33463,
#33464,#33465,#33466,#33467,#33468,#33469,#33470,#33471,#33472,#33473,#33474,
#33475,#33476,#33477,#33478,#33479,#33480,#33481,#33482,#33483,#33484,#33485,
#33486,#33487,#33488,#33489,#33490,#33491,#33492,#33493,#33494,#33495,#33496),
(#33497,#33498,#33499,#33500,#33501,#33502,#33503,#33504,#33505,#33506,
#33507,#33508,#33509,#33510,#33511,#33512,#33513,#33514,#33515,#33516,#33517,
#33518,#33519,#33520,#33521,#33522,#33523,#33524,#33525,#33526,#33527,#33528,
#33529,#33530,#33531,#33532,#33533,#33534,#33535,#33536,#33537,#33538,#33539,
#33540,#33541,#33542,#33543,#33544,#33545,#33546,#33547,#33548,#33549,#33550,
#33551,#33552,#33553,#33554,#33555,#33556,#33557,#33558,#33559,#33560,#33561,
#33562,#33563,#33564,#33565,#33566,#33567,#33568,#33569,#33570,#33571,#33572,
#33573,#33574,#33575,#33576,#33577,#33578,#33579,#33580,#33581,#33582,#33583,
#33584,#33585,#33586,#33587,#33588,#33589,#33590,#33591,#33592,#33593,#33594,
#33595,#33596,#33597,#33598,#33599,#33600,#33601,#33602,#33603,#33604,#33605,
#33606,#33607,#33608,#33609,#33610,#33611,#33612,#33613,#33614,#33615,#33616,
#33617,#33618)),.UNSPECIFIED.,.F.,.F.,.F.,(4,4),(4,1,1,1,1,1,1,1,1,1,1,
1,1,1,1,1,1,1,1,1,1,1,1,1,1,1,1,1,1,1,1,1,1,1,1,1,1,1,1,1,1,1,1,1,1,1,1,
1,1,1,1,1,1,1,1,1,1,1,1,1,1,1,1,1,1,1,1,1,1,1,1,1,1,1,1,1,1,1,1,1,1,1,1,
1,1,1,1,1,1,1,1,1,1,1,1,1,1,1,1,1,1,1,1,1,1,1,1,1,1,1,1,1,1,1,1,1,1,1,1,
4),(0.,0.0448889834294937),(11.8615800042567,12.8590786597072,13.8565773151577,
14.8540759706082,15.8515746260587,16.8490732815092,17.8465719369597,18.8440705924102,
19.8415692478607,20.8390679033112,21.8365665587617,22.8340652142122,23.8315638696627,
24.8290625251132,25.8265611805637,26.8240598360142,27.8215584914647,28.8190571469152,
29.8165558023657,30.8140544578162,31.8115531132667,32.8090517687172,33.8065504241677,
34.8040490796182,35.8015477350687,36.7990463905192,37.7965450459697,38.7940437014202,
39.7915423568707,40.7890410123212,41.7865396677717,42.7840383232222,43.7815369786727,
44.7790356341232,45.7765342895737,46.7740329450242,47.7715316004747,48.7690302559252,
49.7665289113757,50.7640275668262,51.7615262222767,52.7590248777272,53.7565235331777,
54.7540221886282,55.7515208440787,56.7490194995292,57.7465181549797,58.7440168104302,
59.7415154658807,60.7390141213312,61.7365127767817,62.7340114322322,63.7315100876827,
64.7290087431332,65.7265073985837,66.7240060540342,67.7215047094847,68.7190033649352,
69.7165020203857,70.7140006758362,71.7114993312867,72.7089979867372,73.7064966421877,
74.7039952976382,75.7014939530887,76.6989926085392,77.6964912639897,78.6939899194402,
79.6914885748907,80.6889872303412,81.6864858857917,82.6839845412422,83.6814831966927,
84.6789818521432,85.6764805075937,86.6739791630442,87.6714778184947,88.6689764739452,
89.6664751293957,90.6639737848462,91.6614724402967,92.6589710957472,93.6564697511977,
94.6539684066482,95.6514670620987,96.6489657175492,97.6464643729997,98.6439630284502,
99.6414616839007,100.638960339351,101.636458994802,102.633957650252,103.631456305703,
104.628954961153,105.626453616604,106.623952272054,107.621450927505,108.618949582955,
109.616448238406,110.613946893856,111.611445549307,112.608944204757,113.606442860208,
114.603941515658,115.601440171109,116.598938826559,117.59643748201,118.59393613746,
119.591434792911,120.588933448361,121.586432103812,122.583930759262,123.581429414713,
124.578928070163,125.576426725614,126.573925381064,127.571424036515,128.568922691965,
129.566421347416,130.563920002866),.UNSPECIFIED.);
#243=B_SPLINE_SURFACE_WITH_KNOTS('',3,3,((#33726,#33727,#33728,#33729,#33730,
#33731,#33732,#33733,#33734,#33735,#33736,#33737,#33738,#33739,#33740,#33741,
#33742,#33743,#33744,#33745,#33746,#33747,#33748,#33749,#33750,#33751,#33752,
#33753,#33754,#33755,#33756,#33757,#33758,#33759,#33760,#33761,#33762,#33763,
#33764,#33765,#33766,#33767,#33768,#33769,#33770,#33771,#33772,#33773,#33774,
#33775,#33776,#33777,#33778,#33779,#33780,#33781,#33782,#33783,#33784,#33785,
#33786,#33787,#33788,#33789,#33790,#33791,#33792,#33793,#33794,#33795,#33796,
#33797,#33798,#33799,#33800,#33801,#33802,#33803,#33804,#33805,#33806,#33807,
#33808,#33809,#33810,#33811,#33812,#33813,#33814,#33815,#33816,#33817,#33818,
#33819,#33820,#33821,#33822,#33823,#33824,#33825,#33826,#33827,#33828,#33829,
#33830,#33831,#33832,#33833,#33834,#33835,#33836,#33837,#33838,#33839,#33840,
#33841,#33842,#33843,#33844,#33845,#33846,#33847),(#33848,#33849,#33850,
#33851,#33852,#33853,#33854,#33855,#33856,#33857,#33858,#33859,#33860,#33861,
#33862,#33863,#33864,#33865,#33866,#33867,#33868,#33869,#33870,#33871,#33872,
#33873,#33874,#33875,#33876,#33877,#33878,#33879,#33880,#33881,#33882,#33883,
#33884,#33885,#33886,#33887,#33888,#33889,#33890,#33891,#33892,#33893,#33894,
#33895,#33896,#33897,#33898,#33899,#33900,#33901,#33902,#33903,#33904,#33905,
#33906,#33907,#33908,#33909,#33910,#33911,#33912,#33913,#33914,#33915,#33916,
#33917,#33918,#33919,#33920,#33921,#33922,#33923,#33924,#33925,#33926,#33927,
#33928,#33929,#33930,#33931,#33932,#33933,#33934,#33935,#33936,#33937,#33938,
#33939,#33940,#33941,#33942,#33943,#33944,#33945,#33946,#33947,#33948,#33949,
#33950,#33951,#33952,#33953,#33954,#33955,#33956,#33957,#33958,#33959,#33960,
#33961,#33962,#33963,#33964,#33965,#33966,#33967,#33968,#33969),(#33970,
#33971,#33972,#33973,#33974,#33975,#33976,#33977,#33978,#33979,#33980,#33981,
#33982,#33983,#33984,#33985,#33986,#33987,#33988,#33989,#33990,#33991,#33992,
#33993,#33994,#33995,#33996,#33997,#33998,#33999,#34000,#34001,#34002,#34003,
#34004,#34005,#34006,#34007,#34008,#34009,#34010,#34011,#34012,#34013,#34014,
#34015,#34016,#34017,#34018,#34019,#34020,#34021,#34022,#34023,#34024,#34025,
#34026,#34027,#34028,#34029,#34030,#34031,#34032,#34033,#34034,#34035,#34036,
#34037,#34038,#34039,#34040,#34041,#34042,#34043,#34044,#34045,#34046,#34047,
#34048,#34049,#34050,#34051,#34052,#34053,#34054,#34055,#34056,#34057,#34058,
#34059,#34060,#34061,#34062,#34063,#34064,#34065,#34066,#34067,#34068,#34069,
#34070,#34071,#34072,#34073,#34074,#34075,#34076,#34077,#34078,#34079,#34080,
#34081,#34082,#34083,#34084,#34085,#34086,#34087,#34088,#34089,#34090,#34091),
(#34092,#34093,#34094,#34095,#34096,#34097,#34098,#34099,#34100,#34101,
#34102,#34103,#34104,#34105,#34106,#34107,#34108,#34109,#34110,#34111,#34112,
#34113,#34114,#34115,#34116,#34117,#34118,#34119,#34120,#34121,#34122,#34123,
#34124,#34125,#34126,#34127,#34128,#34129,#34130,#34131,#34132,#34133,#34134,
#34135,#34136,#34137,#34138,#34139,#34140,#34141,#34142,#34143,#34144,#34145,
#34146,#34147,#34148,#34149,#34150,#34151,#34152,#34153,#34154,#34155,#34156,
#34157,#34158,#34159,#34160,#34161,#34162,#34163,#34164,#34165,#34166,#34167,
#34168,#34169,#34170,#34171,#34172,#34173,#34174,#34175,#34176,#34177,#34178,
#34179,#34180,#34181,#34182,#34183,#34184,#34185,#34186,#34187,#34188,#34189,
#34190,#34191,#34192,#34193,#34194,#34195,#34196,#34197,#34198,#34199,#34200,
#34201,#34202,#34203,#34204,#34205,#34206,#34207,#34208,#34209,#34210,#34211,
#34212,#34213)),.UNSPECIFIED.,.F.,.F.,.F.,(4,4),(4,1,1,1,1,1,1,1,1,1,1,
1,1,1,1,1,1,1,1,1,1,1,1,1,1,1,1,1,1,1,1,1,1,1,1,1,1,1,1,1,1,1,1,1,1,1,1,
1,1,1,1,1,1,1,1,1,1,1,1,1,1,1,1,1,1,1,1,1,1,1,1,1,1,1,1,1,1,1,1,1,1,1,1,
1,1,1,1,1,1,1,1,1,1,1,1,1,1,1,1,1,1,1,1,1,1,1,1,1,1,1,1,1,1,1,1,1,1,1,1,
4),(0.,0.0448889834294937),(14.398141012777,15.3956396682275,16.393138323678,
17.3906369791285,18.388135634579,19.3856342900295,20.38313294548,21.3806316009305,
22.378130256381,23.3756289118315,24.373127567282,25.3706262227325,26.368124878183,
27.3656235336335,28.363122189084,29.3606208445345,30.358119499985,31.3556181554355,
32.353116810886,33.3506154663365,34.348114121787,35.3456127772375,36.343111432688,
37.3406100881385,38.338108743589,39.3356073990395,40.33310605449,41.3306047099405,
42.328103365391,43.3256020208415,44.323100676292,45.3205993317425,46.318097987193,
47.3155966426435,48.313095298094,49.3105939535445,50.308092608995,51.3055912644455,
52.303089919896,53.3005885753465,54.298087230797,55.2955858862475,56.293084541698,
57.2905831971485,58.288081852599,59.2855805080495,60.2830791635,61.2805778189505,
62.278076474401,63.2755751298515,64.273073785302,65.2705724407525,66.268071096203,
67.2655697516535,68.263068407104,69.2605670625545,70.258065718005,71.2555643734555,
72.253063028906,73.2505616843565,74.248060339807,75.2455589952575,76.243057650708,
77.2405563061585,78.238054961609,79.2355536170595,80.23305227251,81.2305509279605,
82.228049583411,83.2255482388615,84.223046894312,85.2205455497625,86.218044205213,
87.2155428606635,88.213041516114,89.2105401715645,90.208038827015,91.2055374824655,
92.203036137916,93.2005347933665,94.198033448817,95.1955321042675,96.193030759718,
97.1905294151685,98.1880280706191,99.1855267260696,100.18302538152,101.180524036971,
102.178022692421,103.175521347872,104.173020003322,105.170518658773,106.168017314223,
107.165515969674,108.163014625124,109.160513280575,110.158011936025,111.155510591476,
112.153009246926,113.150507902377,114.148006557827,115.145505213278,116.143003868728,
117.140502524179,118.138001179629,119.13549983508,120.13299849053,121.130497145981,
122.127995801431,123.125494456882,124.122993112332,125.120491767783,126.117990423233,
127.115489078684,128.112987734134,129.110486389585,130.107985045035,131.105483700486,
132.102982355936,133.100481011387),.UNSPECIFIED.);
#244=B_SPLINE_SURFACE_WITH_KNOTS('',3,3,((#34518,#34519,#34520,#34521,#34522,
#34523,#34524,#34525,#34526,#34527,#34528,#34529,#34530,#34531,#34532,#34533,
#34534,#34535,#34536,#34537,#34538,#34539,#34540,#34541,#34542,#34543,#34544,
#34545,#34546,#34547,#34548,#34549,#34550,#34551,#34552,#34553,#34554,#34555,
#34556,#34557,#34558,#34559,#34560,#34561,#34562,#34563,#34564,#34565,#34566,
#34567,#34568,#34569,#34570,#34571,#34572,#34573,#34574,#34575,#34576,#34577,
#34578,#34579,#34580,#34581,#34582,#34583,#34584,#34585,#34586,#34587,#34588,
#34589,#34590,#34591,#34592,#34593,#34594,#34595,#34596,#34597,#34598,#34599,
#34600,#34601,#34602,#34603,#34604,#34605,#34606,#34607,#34608,#34609,#34610,
#34611,#34612,#34613,#34614,#34615,#34616,#34617,#34618,#34619,#34620,#34621,
#34622,#34623,#34624,#34625,#34626,#34627,#34628,#34629,#34630,#34631,#34632,
#34633,#34634,#34635,#34636,#34637,#34638,#34639),(#34640,#34641,#34642,
#34643,#34644,#34645,#34646,#34647,#34648,#34649,#34650,#34651,#34652,#34653,
#34654,#34655,#34656,#34657,#34658,#34659,#34660,#34661,#34662,#34663,#34664,
#34665,#34666,#34667,#34668,#34669,#34670,#34671,#34672,#34673,#34674,#34675,
#34676,#34677,#34678,#34679,#34680,#34681,#34682,#34683,#34684,#34685,#34686,
#34687,#34688,#34689,#34690,#34691,#34692,#34693,#34694,#34695,#34696,#34697,
#34698,#34699,#34700,#34701,#34702,#34703,#34704,#34705,#34706,#34707,#34708,
#34709,#34710,#34711,#34712,#34713,#34714,#34715,#34716,#34717,#34718,#34719,
#34720,#34721,#34722,#34723,#34724,#34725,#34726,#34727,#34728,#34729,#34730,
#34731,#34732,#34733,#34734,#34735,#34736,#34737,#34738,#34739,#34740,#34741,
#34742,#34743,#34744,#34745,#34746,#34747,#34748,#34749,#34750,#34751,#34752,
#34753,#34754,#34755,#34756,#34757,#34758,#34759,#34760,#34761),(#34762,
#34763,#34764,#34765,#34766,#34767,#34768,#34769,#34770,#34771,#34772,#34773,
#34774,#34775,#34776,#34777,#34778,#34779,#34780,#34781,#34782,#34783,#34784,
#34785,#34786,#34787,#34788,#34789,#34790,#34791,#34792,#34793,#34794,#34795,
#34796,#34797,#34798,#34799,#34800,#34801,#34802,#34803,#34804,#34805,#34806,
#34807,#34808,#34809,#34810,#34811,#34812,#34813,#34814,#34815,#34816,#34817,
#34818,#34819,#34820,#34821,#34822,#34823,#34824,#34825,#34826,#34827,#34828,
#34829,#34830,#34831,#34832,#34833,#34834,#34835,#34836,#34837,#34838,#34839,
#34840,#34841,#34842,#34843,#34844,#34845,#34846,#34847,#34848,#34849,#34850,
#34851,#34852,#34853,#34854,#34855,#34856,#34857,#34858,#34859,#34860,#34861,
#34862,#34863,#34864,#34865,#34866,#34867,#34868,#34869,#34870,#34871,#34872,
#34873,#34874,#34875,#34876,#34877,#34878,#34879,#34880,#34881,#34882,#34883),
(#34884,#34885,#34886,#34887,#34888,#34889,#34890,#34891,#34892,#34893,
#34894,#34895,#34896,#34897,#34898,#34899,#34900,#34901,#34902,#34903,#34904,
#34905,#34906,#34907,#34908,#34909,#34910,#34911,#34912,#34913,#34914,#34915,
#34916,#34917,#34918,#34919,#34920,#34921,#34922,#34923,#34924,#34925,#34926,
#34927,#34928,#34929,#34930,#34931,#34932,#34933,#34934,#34935,#34936,#34937,
#34938,#34939,#34940,#34941,#34942,#34943,#34944,#34945,#34946,#34947,#34948,
#34949,#34950,#34951,#34952,#34953,#34954,#34955,#34956,#34957,#34958,#34959,
#34960,#34961,#34962,#34963,#34964,#34965,#34966,#34967,#34968,#34969,#34970,
#34971,#34972,#34973,#34974,#34975,#34976,#34977,#34978,#34979,#34980,#34981,
#34982,#34983,#34984,#34985,#34986,#34987,#34988,#34989,#34990,#34991,#34992,
#34993,#34994,#34995,#34996,#34997,#34998,#34999,#35000,#35001,#35002,#35003,
#35004,#35005)),.UNSPECIFIED.,.F.,.F.,.F.,(4,4),(4,1,1,1,1,1,1,1,1,1,1,
1,1,1,1,1,1,1,1,1,1,1,1,1,1,1,1,1,1,1,1,1,1,1,1,1,1,1,1,1,1,1,1,1,1,1,1,
1,1,1,1,1,1,1,1,1,1,1,1,1,1,1,1,1,1,1,1,1,1,1,1,1,1,1,1,1,1,1,1,1,1,1,1,
1,1,1,1,1,1,1,1,1,1,1,1,1,1,1,1,1,1,1,1,1,1,1,1,1,1,1,1,1,1,1,1,1,1,1,1,
4),(0.,0.0448889834294937),(11.861580004257,12.8590786597075,13.856577315158,
14.8540759706085,15.851574626059,16.8490732815095,17.84657193696,18.8440705924105,
19.841569247861,20.8390679033115,21.836566558762,22.8340652142125,23.831563869663,
24.8290625251135,25.826561180564,26.8240598360145,27.821558491465,28.8190571469155,
29.816555802366,30.8140544578165,31.811553113267,32.8090517687175,33.806550424168,
34.8040490796185,35.801547735069,36.7990463905195,37.79654504597,38.7940437014205,
39.791542356871,40.7890410123215,41.786539667772,42.7840383232225,43.781536978673,
44.7790356341235,45.776534289574,46.7740329450245,47.771531600475,48.7690302559255,
49.766528911376,50.7640275668265,51.761526222277,52.7590248777275,53.756523533178,
54.7540221886285,55.751520844079,56.7490194995295,57.74651815498,58.7440168104305,
59.741515465881,60.7390141213315,61.736512776782,62.7340114322325,63.731510087683,
64.7290087431335,65.726507398584,66.7240060540345,67.721504709485,68.7190033649355,
69.716502020386,70.7140006758365,71.711499331287,72.7089979867375,73.706496642188,
74.7039952976385,75.701493953089,76.6989926085395,77.69649126399,78.6939899194405,
79.691488574891,80.6889872303415,81.686485885792,82.6839845412425,83.681483196693,
84.6789818521435,85.676480507594,86.6739791630445,87.671477818495,88.6689764739455,
89.666475129396,90.6639737848465,91.661472440297,92.6589710957475,93.656469751198,
94.6539684066485,95.651467062099,96.6489657175495,97.646464373,98.6439630284505,
99.641461683901,100.638960339352,101.636458994802,102.633957650253,103.631456305703,
104.628954961154,105.626453616604,106.623952272055,107.621450927505,108.618949582956,
109.616448238406,110.613946893857,111.611445549307,112.608944204758,113.606442860208,
114.603941515659,115.601440171109,116.59893882656,117.59643748201,118.593936137461,
119.591434792911,120.588933448362,121.586432103812,122.583930759263,123.581429414713,
124.578928070164,125.576426725614,126.573925381065,127.571424036515,128.568922691966,
129.566421347416,130.563920002867),.UNSPECIFIED.);
#245=B_SPLINE_SURFACE_WITH_KNOTS('',3,3,((#35113,#35114,#35115,#35116,#35117,
#35118,#35119,#35120,#35121,#35122,#35123,#35124,#35125,#35126,#35127,#35128,
#35129,#35130,#35131,#35132,#35133,#35134,#35135,#35136,#35137,#35138,#35139,
#35140,#35141,#35142,#35143,#35144,#35145,#35146,#35147,#35148,#35149,#35150,
#35151,#35152,#35153,#35154,#35155,#35156,#35157,#35158,#35159,#35160,#35161,
#35162,#35163,#35164,#35165,#35166,#35167,#35168,#35169,#35170,#35171,#35172,
#35173,#35174,#35175,#35176,#35177,#35178,#35179,#35180,#35181,#35182,#35183,
#35184,#35185,#35186,#35187,#35188,#35189,#35190,#35191,#35192,#35193,#35194,
#35195,#35196,#35197,#35198,#35199,#35200,#35201,#35202,#35203,#35204,#35205,
#35206,#35207,#35208,#35209,#35210,#35211,#35212,#35213,#35214,#35215,#35216,
#35217,#35218,#35219,#35220,#35221,#35222,#35223,#35224,#35225,#35226,#35227,
#35228,#35229,#35230,#35231,#35232,#35233,#35234),(#35235,#35236,#35237,
#35238,#35239,#35240,#35241,#35242,#35243,#35244,#35245,#35246,#35247,#35248,
#35249,#35250,#35251,#35252,#35253,#35254,#35255,#35256,#35257,#35258,#35259,
#35260,#35261,#35262,#35263,#35264,#35265,#35266,#35267,#35268,#35269,#35270,
#35271,#35272,#35273,#35274,#35275,#35276,#35277,#35278,#35279,#35280,#35281,
#35282,#35283,#35284,#35285,#35286,#35287,#35288,#35289,#35290,#35291,#35292,
#35293,#35294,#35295,#35296,#35297,#35298,#35299,#35300,#35301,#35302,#35303,
#35304,#35305,#35306,#35307,#35308,#35309,#35310,#35311,#35312,#35313,#35314,
#35315,#35316,#35317,#35318,#35319,#35320,#35321,#35322,#35323,#35324,#35325,
#35326,#35327,#35328,#35329,#35330,#35331,#35332,#35333,#35334,#35335,#35336,
#35337,#35338,#35339,#35340,#35341,#35342,#35343,#35344,#35345,#35346,#35347,
#35348,#35349,#35350,#35351,#35352,#35353,#35354,#35355,#35356),(#35357,
#35358,#35359,#35360,#35361,#35362,#35363,#35364,#35365,#35366,#35367,#35368,
#35369,#35370,#35371,#35372,#35373,#35374,#35375,#35376,#35377,#35378,#35379,
#35380,#35381,#35382,#35383,#35384,#35385,#35386,#35387,#35388,#35389,#35390,
#35391,#35392,#35393,#35394,#35395,#35396,#35397,#35398,#35399,#35400,#35401,
#35402,#35403,#35404,#35405,#35406,#35407,#35408,#35409,#35410,#35411,#35412,
#35413,#35414,#35415,#35416,#35417,#35418,#35419,#35420,#35421,#35422,#35423,
#35424,#35425,#35426,#35427,#35428,#35429,#35430,#35431,#35432,#35433,#35434,
#35435,#35436,#35437,#35438,#35439,#35440,#35441,#35442,#35443,#35444,#35445,
#35446,#35447,#35448,#35449,#35450,#35451,#35452,#35453,#35454,#35455,#35456,
#35457,#35458,#35459,#35460,#35461,#35462,#35463,#35464,#35465,#35466,#35467,
#35468,#35469,#35470,#35471,#35472,#35473,#35474,#35475,#35476,#35477,#35478),
(#35479,#35480,#35481,#35482,#35483,#35484,#35485,#35486,#35487,#35488,
#35489,#35490,#35491,#35492,#35493,#35494,#35495,#35496,#35497,#35498,#35499,
#35500,#35501,#35502,#35503,#35504,#35505,#35506,#35507,#35508,#35509,#35510,
#35511,#35512,#35513,#35514,#35515,#35516,#35517,#35518,#35519,#35520,#35521,
#35522,#35523,#35524,#35525,#35526,#35527,#35528,#35529,#35530,#35531,#35532,
#35533,#35534,#35535,#35536,#35537,#35538,#35539,#35540,#35541,#35542,#35543,
#35544,#35545,#35546,#35547,#35548,#35549,#35550,#35551,#35552,#35553,#35554,
#35555,#35556,#35557,#35558,#35559,#35560,#35561,#35562,#35563,#35564,#35565,
#35566,#35567,#35568,#35569,#35570,#35571,#35572,#35573,#35574,#35575,#35576,
#35577,#35578,#35579,#35580,#35581,#35582,#35583,#35584,#35585,#35586,#35587,
#35588,#35589,#35590,#35591,#35592,#35593,#35594,#35595,#35596,#35597,#35598,
#35599,#35600)),.UNSPECIFIED.,.F.,.F.,.F.,(4,4),(4,1,1,1,1,1,1,1,1,1,1,
1,1,1,1,1,1,1,1,1,1,1,1,1,1,1,1,1,1,1,1,1,1,1,1,1,1,1,1,1,1,1,1,1,1,1,1,
1,1,1,1,1,1,1,1,1,1,1,1,1,1,1,1,1,1,1,1,1,1,1,1,1,1,1,1,1,1,1,1,1,1,1,1,
1,1,1,1,1,1,1,1,1,1,1,1,1,1,1,1,1,1,1,1,1,1,1,1,1,1,1,1,1,1,1,1,1,1,1,1,
4),(0.,0.0448889834294937),(14.3981410127773,15.3956396682278,16.3931383236783,
17.3906369791288,18.3881356345793,19.3856342900298,20.3831329454803,21.3806316009308,
22.3781302563813,23.3756289118318,24.3731275672823,25.3706262227328,26.3681248781833,
27.3656235336338,28.3631221890843,29.3606208445348,30.3581194999853,31.3556181554358,
32.3531168108863,33.3506154663368,34.3481141217873,35.3456127772378,36.3431114326883,
37.3406100881388,38.3381087435893,39.3356073990398,40.3331060544903,41.3306047099408,
42.3281033653913,43.3256020208418,44.3231006762923,45.3205993317428,46.3180979871933,
47.3155966426438,48.3130952980943,49.3105939535448,50.3080926089953,51.3055912644458,
52.3030899198963,53.3005885753468,54.2980872307973,55.2955858862478,56.2930845416983,
57.2905831971488,58.2880818525993,59.2855805080498,60.2830791635003,61.2805778189508,
62.2780764744013,63.2755751298518,64.2730737853023,65.2705724407528,66.2680710962033,
67.2655697516538,68.2630684071043,69.2605670625549,70.2580657180054,71.2555643734559,
72.2530630289064,73.2505616843569,74.2480603398074,75.2455589952579,76.2430576507084,
77.2405563061589,78.2380549616094,79.2355536170598,80.2330522725103,81.2305509279608,
82.2280495834113,83.2255482388618,84.2230468943123,85.2205455497629,86.2180442052134,
87.2155428606639,88.2130415161144,89.2105401715649,90.2080388270154,91.2055374824659,
92.2030361379164,93.2005347933669,94.1980334488174,95.1955321042679,96.1930307597184,
97.1905294151689,98.1880280706194,99.1855267260699,100.18302538152,101.180524036971,
102.178022692421,103.175521347872,104.173020003322,105.170518658773,106.168017314223,
107.165515969674,108.163014625124,109.160513280575,110.158011936025,111.155510591476,
112.153009246926,113.150507902377,114.148006557827,115.145505213278,116.143003868728,
117.140502524179,118.138001179629,119.13549983508,120.13299849053,121.130497145981,
122.127995801431,123.125494456882,124.122993112332,125.120491767783,126.117990423233,
127.115489078684,128.112987734134,129.110486389585,130.107985045035,131.105483700486,
132.102982355936,133.100481011387),.UNSPECIFIED.);
#246=B_SPLINE_SURFACE_WITH_KNOTS('',3,3,((#35905,#35906,#35907,#35908,#35909,
#35910,#35911,#35912,#35913,#35914,#35915,#35916,#35917,#35918,#35919,#35920,
#35921,#35922,#35923,#35924,#35925,#35926,#35927,#35928,#35929,#35930,#35931,
#35932,#35933,#35934,#35935,#35936,#35937,#35938,#35939,#35940,#35941,#35942,
#35943,#35944,#35945,#35946,#35947,#35948,#35949,#35950,#35951,#35952,#35953,
#35954,#35955,#35956,#35957,#35958,#35959,#35960,#35961,#35962,#35963,#35964,
#35965,#35966,#35967,#35968,#35969,#35970,#35971,#35972,#35973,#35974,#35975,
#35976,#35977,#35978,#35979,#35980,#35981,#35982,#35983,#35984,#35985,#35986,
#35987,#35988,#35989,#35990,#35991,#35992,#35993,#35994,#35995,#35996,#35997,
#35998,#35999,#36000,#36001,#36002,#36003,#36004,#36005,#36006,#36007,#36008,
#36009,#36010,#36011,#36012,#36013,#36014,#36015,#36016,#36017,#36018,#36019,
#36020,#36021,#36022,#36023,#36024,#36025,#36026),(#36027,#36028,#36029,
#36030,#36031,#36032,#36033,#36034,#36035,#36036,#36037,#36038,#36039,#36040,
#36041,#36042,#36043,#36044,#36045,#36046,#36047,#36048,#36049,#36050,#36051,
#36052,#36053,#36054,#36055,#36056,#36057,#36058,#36059,#36060,#36061,#36062,
#36063,#36064,#36065,#36066,#36067,#36068,#36069,#36070,#36071,#36072,#36073,
#36074,#36075,#36076,#36077,#36078,#36079,#36080,#36081,#36082,#36083,#36084,
#36085,#36086,#36087,#36088,#36089,#36090,#36091,#36092,#36093,#36094,#36095,
#36096,#36097,#36098,#36099,#36100,#36101,#36102,#36103,#36104,#36105,#36106,
#36107,#36108,#36109,#36110,#36111,#36112,#36113,#36114,#36115,#36116,#36117,
#36118,#36119,#36120,#36121,#36122,#36123,#36124,#36125,#36126,#36127,#36128,
#36129,#36130,#36131,#36132,#36133,#36134,#36135,#36136,#36137,#36138,#36139,
#36140,#36141,#36142,#36143,#36144,#36145,#36146,#36147,#36148),(#36149,
#36150,#36151,#36152,#36153,#36154,#36155,#36156,#36157,#36158,#36159,#36160,
#36161,#36162,#36163,#36164,#36165,#36166,#36167,#36168,#36169,#36170,#36171,
#36172,#36173,#36174,#36175,#36176,#36177,#36178,#36179,#36180,#36181,#36182,
#36183,#36184,#36185,#36186,#36187,#36188,#36189,#36190,#36191,#36192,#36193,
#36194,#36195,#36196,#36197,#36198,#36199,#36200,#36201,#36202,#36203,#36204,
#36205,#36206,#36207,#36208,#36209,#36210,#36211,#36212,#36213,#36214,#36215,
#36216,#36217,#36218,#36219,#36220,#36221,#36222,#36223,#36224,#36225,#36226,
#36227,#36228,#36229,#36230,#36231,#36232,#36233,#36234,#36235,#36236,#36237,
#36238,#36239,#36240,#36241,#36242,#36243,#36244,#36245,#36246,#36247,#36248,
#36249,#36250,#36251,#36252,#36253,#36254,#36255,#36256,#36257,#36258,#36259,
#36260,#36261,#36262,#36263,#36264,#36265,#36266,#36267,#36268,#36269,#36270),
(#36271,#36272,#36273,#36274,#36275,#36276,#36277,#36278,#36279,#36280,
#36281,#36282,#36283,#36284,#36285,#36286,#36287,#36288,#36289,#36290,#36291,
#36292,#36293,#36294,#36295,#36296,#36297,#36298,#36299,#36300,#36301,#36302,
#36303,#36304,#36305,#36306,#36307,#36308,#36309,#36310,#36311,#36312,#36313,
#36314,#36315,#36316,#36317,#36318,#36319,#36320,#36321,#36322,#36323,#36324,
#36325,#36326,#36327,#36328,#36329,#36330,#36331,#36332,#36333,#36334,#36335,
#36336,#36337,#36338,#36339,#36340,#36341,#36342,#36343,#36344,#36345,#36346,
#36347,#36348,#36349,#36350,#36351,#36352,#36353,#36354,#36355,#36356,#36357,
#36358,#36359,#36360,#36361,#36362,#36363,#36364,#36365,#36366,#36367,#36368,
#36369,#36370,#36371,#36372,#36373,#36374,#36375,#36376,#36377,#36378,#36379,
#36380,#36381,#36382,#36383,#36384,#36385,#36386,#36387,#36388,#36389,#36390,
#36391,#36392)),.UNSPECIFIED.,.F.,.F.,.F.,(4,4),(4,1,1,1,1,1,1,1,1,1,1,
1,1,1,1,1,1,1,1,1,1,1,1,1,1,1,1,1,1,1,1,1,1,1,1,1,1,1,1,1,1,1,1,1,1,1,1,
1,1,1,1,1,1,1,1,1,1,1,1,1,1,1,1,1,1,1,1,1,1,1,1,1,1,1,1,1,1,1,1,1,1,1,1,
1,1,1,1,1,1,1,1,1,1,1,1,1,1,1,1,1,1,1,1,1,1,1,1,1,1,1,1,1,1,1,1,1,1,1,1,
4),(0.,0.0448889834294937),(11.861580004257,12.8590786597075,13.856577315158,
14.8540759706085,15.851574626059,16.8490732815095,17.84657193696,18.8440705924105,
19.841569247861,20.8390679033115,21.836566558762,22.8340652142125,23.831563869663,
24.8290625251135,25.826561180564,26.8240598360145,27.821558491465,28.8190571469155,
29.816555802366,30.8140544578165,31.811553113267,32.8090517687175,33.806550424168,
34.8040490796185,35.801547735069,36.7990463905195,37.79654504597,38.7940437014205,
39.791542356871,40.7890410123215,41.786539667772,42.7840383232225,43.781536978673,
44.7790356341235,45.776534289574,46.7740329450245,47.771531600475,48.7690302559255,
49.766528911376,50.7640275668265,51.761526222277,52.7590248777275,53.756523533178,
54.7540221886285,55.751520844079,56.7490194995295,57.74651815498,58.7440168104305,
59.741515465881,60.7390141213315,61.736512776782,62.7340114322325,63.731510087683,
64.7290087431335,65.726507398584,66.7240060540345,67.721504709485,68.7190033649355,
69.716502020386,70.7140006758365,71.711499331287,72.7089979867375,73.706496642188,
74.7039952976385,75.701493953089,76.6989926085395,77.69649126399,78.6939899194405,
79.691488574891,80.6889872303415,81.686485885792,82.6839845412425,83.681483196693,
84.6789818521435,85.676480507594,86.6739791630445,87.671477818495,88.6689764739455,
89.666475129396,90.6639737848465,91.661472440297,92.6589710957475,93.656469751198,
94.6539684066485,95.651467062099,96.6489657175495,97.646464373,98.6439630284505,
99.641461683901,100.638960339352,101.636458994802,102.633957650253,103.631456305703,
104.628954961154,105.626453616604,106.623952272055,107.621450927505,108.618949582956,
109.616448238406,110.613946893857,111.611445549307,112.608944204758,113.606442860208,
114.603941515659,115.601440171109,116.59893882656,117.59643748201,118.593936137461,
119.591434792911,120.588933448362,121.586432103812,122.583930759263,123.581429414713,
124.578928070164,125.576426725614,126.573925381065,127.571424036515,128.568922691966,
129.566421347416,130.563920002867),.UNSPECIFIED.);
#247=B_SPLINE_SURFACE_WITH_KNOTS('',3,3,((#36500,#36501,#36502,#36503,#36504,
#36505,#36506,#36507,#36508,#36509,#36510,#36511,#36512,#36513,#36514,#36515,
#36516,#36517,#36518,#36519,#36520,#36521,#36522,#36523,#36524,#36525,#36526,
#36527,#36528,#36529,#36530,#36531,#36532,#36533,#36534,#36535,#36536,#36537,
#36538,#36539,#36540,#36541,#36542,#36543,#36544,#36545,#36546,#36547,#36548,
#36549,#36550,#36551,#36552,#36553,#36554,#36555,#36556,#36557,#36558,#36559,
#36560,#36561,#36562,#36563,#36564,#36565,#36566,#36567,#36568,#36569,#36570,
#36571,#36572,#36573,#36574,#36575,#36576,#36577,#36578,#36579,#36580,#36581,
#36582,#36583,#36584,#36585,#36586,#36587,#36588,#36589,#36590,#36591,#36592,
#36593,#36594,#36595,#36596,#36597,#36598,#36599,#36600,#36601,#36602,#36603,
#36604,#36605,#36606,#36607,#36608,#36609,#36610,#36611,#36612,#36613,#36614,
#36615,#36616,#36617,#36618,#36619,#36620,#36621),(#36622,#36623,#36624,
#36625,#36626,#36627,#36628,#36629,#36630,#36631,#36632,#36633,#36634,#36635,
#36636,#36637,#36638,#36639,#36640,#36641,#36642,#36643,#36644,#36645,#36646,
#36647,#36648,#36649,#36650,#36651,#36652,#36653,#36654,#36655,#36656,#36657,
#36658,#36659,#36660,#36661,#36662,#36663,#36664,#36665,#36666,#36667,#36668,
#36669,#36670,#36671,#36672,#36673,#36674,#36675,#36676,#36677,#36678,#36679,
#36680,#36681,#36682,#36683,#36684,#36685,#36686,#36687,#36688,#36689,#36690,
#36691,#36692,#36693,#36694,#36695,#36696,#36697,#36698,#36699,#36700,#36701,
#36702,#36703,#36704,#36705,#36706,#36707,#36708,#36709,#36710,#36711,#36712,
#36713,#36714,#36715,#36716,#36717,#36718,#36719,#36720,#36721,#36722,#36723,
#36724,#36725,#36726,#36727,#36728,#36729,#36730,#36731,#36732,#36733,#36734,
#36735,#36736,#36737,#36738,#36739,#36740,#36741,#36742,#36743),(#36744,
#36745,#36746,#36747,#36748,#36749,#36750,#36751,#36752,#36753,#36754,#36755,
#36756,#36757,#36758,#36759,#36760,#36761,#36762,#36763,#36764,#36765,#36766,
#36767,#36768,#36769,#36770,#36771,#36772,#36773,#36774,#36775,#36776,#36777,
#36778,#36779,#36780,#36781,#36782,#36783,#36784,#36785,#36786,#36787,#36788,
#36789,#36790,#36791,#36792,#36793,#36794,#36795,#36796,#36797,#36798,#36799,
#36800,#36801,#36802,#36803,#36804,#36805,#36806,#36807,#36808,#36809,#36810,
#36811,#36812,#36813,#36814,#36815,#36816,#36817,#36818,#36819,#36820,#36821,
#36822,#36823,#36824,#36825,#36826,#36827,#36828,#36829,#36830,#36831,#36832,
#36833,#36834,#36835,#36836,#36837,#36838,#36839,#36840,#36841,#36842,#36843,
#36844,#36845,#36846,#36847,#36848,#36849,#36850,#36851,#36852,#36853,#36854,
#36855,#36856,#36857,#36858,#36859,#36860,#36861,#36862,#36863,#36864,#36865),
(#36866,#36867,#36868,#36869,#36870,#36871,#36872,#36873,#36874,#36875,
#36876,#36877,#36878,#36879,#36880,#36881,#36882,#36883,#36884,#36885,#36886,
#36887,#36888,#36889,#36890,#36891,#36892,#36893,#36894,#36895,#36896,#36897,
#36898,#36899,#36900,#36901,#36902,#36903,#36904,#36905,#36906,#36907,#36908,
#36909,#36910,#36911,#36912,#36913,#36914,#36915,#36916,#36917,#36918,#36919,
#36920,#36921,#36922,#36923,#36924,#36925,#36926,#36927,#36928,#36929,#36930,
#36931,#36932,#36933,#36934,#36935,#36936,#36937,#36938,#36939,#36940,#36941,
#36942,#36943,#36944,#36945,#36946,#36947,#36948,#36949,#36950,#36951,#36952,
#36953,#36954,#36955,#36956,#36957,#36958,#36959,#36960,#36961,#36962,#36963,
#36964,#36965,#36966,#36967,#36968,#36969,#36970,#36971,#36972,#36973,#36974,
#36975,#36976,#36977,#36978,#36979,#36980,#36981,#36982,#36983,#36984,#36985,
#36986,#36987)),.UNSPECIFIED.,.F.,.F.,.F.,(4,4),(4,1,1,1,1,1,1,1,1,1,1,
1,1,1,1,1,1,1,1,1,1,1,1,1,1,1,1,1,1,1,1,1,1,1,1,1,1,1,1,1,1,1,1,1,1,1,1,
1,1,1,1,1,1,1,1,1,1,1,1,1,1,1,1,1,1,1,1,1,1,1,1,1,1,1,1,1,1,1,1,1,1,1,1,
1,1,1,1,1,1,1,1,1,1,1,1,1,1,1,1,1,1,1,1,1,1,1,1,1,1,1,1,1,1,1,1,1,1,1,1,
4),(0.,0.0448889834294937),(14.3981410127773,15.3956396682278,16.3931383236783,
17.3906369791288,18.3881356345793,19.3856342900298,20.3831329454803,21.3806316009308,
22.3781302563813,23.3756289118318,24.3731275672823,25.3706262227328,26.3681248781833,
27.3656235336338,28.3631221890843,29.3606208445348,30.3581194999853,31.3556181554358,
32.3531168108863,33.3506154663368,34.3481141217873,35.3456127772378,36.3431114326883,
37.3406100881388,38.3381087435893,39.3356073990398,40.3331060544903,41.3306047099408,
42.3281033653913,43.3256020208418,44.3231006762923,45.3205993317428,46.3180979871933,
47.3155966426438,48.3130952980943,49.3105939535448,50.3080926089953,51.3055912644458,
52.3030899198963,53.3005885753468,54.2980872307973,55.2955858862478,56.2930845416983,
57.2905831971488,58.2880818525993,59.2855805080498,60.2830791635003,61.2805778189508,
62.2780764744013,63.2755751298518,64.2730737853023,65.2705724407528,66.2680710962033,
67.2655697516538,68.2630684071043,69.2605670625549,70.2580657180054,71.2555643734559,
72.2530630289064,73.2505616843569,74.2480603398074,75.2455589952579,76.2430576507084,
77.2405563061589,78.2380549616094,79.2355536170598,80.2330522725103,81.2305509279608,
82.2280495834113,83.2255482388618,84.2230468943123,85.2205455497629,86.2180442052134,
87.2155428606639,88.2130415161144,89.2105401715649,90.2080388270154,91.2055374824659,
92.2030361379164,93.2005347933669,94.1980334488174,95.1955321042679,96.1930307597184,
97.1905294151689,98.1880280706194,99.1855267260699,100.18302538152,101.180524036971,
102.178022692421,103.175521347872,104.173020003322,105.170518658773,106.168017314223,
107.165515969674,108.163014625124,109.160513280575,110.158011936025,111.155510591476,
112.153009246926,113.150507902377,114.148006557827,115.145505213278,116.143003868728,
117.140502524179,118.138001179629,119.13549983508,120.13299849053,121.130497145981,
122.127995801431,123.125494456882,124.122993112332,125.120491767783,126.117990423233,
127.115489078684,128.112987734134,129.110486389585,130.107985045035,131.105483700486,
132.102982355936,133.100481011387),.UNSPECIFIED.);
#248=B_SPLINE_SURFACE_WITH_KNOTS('',3,3,((#37296,#37297,#37298,#37299,#37300,
#37301,#37302,#37303,#37304,#37305,#37306,#37307,#37308,#37309,#37310,#37311,
#37312,#37313,#37314,#37315,#37316,#37317,#37318,#37319,#37320,#37321,#37322,
#37323,#37324,#37325,#37326,#37327,#37328,#37329,#37330,#37331,#37332,#37333,
#37334,#37335,#37336,#37337,#37338,#37339,#37340,#37341,#37342,#37343,#37344,
#37345,#37346,#37347,#37348,#37349,#37350,#37351,#37352,#37353,#37354,#37355,
#37356,#37357,#37358,#37359,#37360,#37361,#37362,#37363,#37364,#37365,#37366,
#37367,#37368,#37369,#37370,#37371,#37372,#37373,#37374,#37375,#37376,#37377,
#37378,#37379,#37380,#37381,#37382,#37383,#37384,#37385,#37386,#37387,#37388,
#37389,#37390,#37391,#37392,#37393,#37394,#37395,#37396,#37397,#37398,#37399,
#37400,#37401,#37402,#37403,#37404,#37405,#37406,#37407,#37408,#37409,#37410,
#37411,#37412,#37413,#37414,#37415,#37416,#37417),(#37418,#37419,#37420,
#37421,#37422,#37423,#37424,#37425,#37426,#37427,#37428,#37429,#37430,#37431,
#37432,#37433,#37434,#37435,#37436,#37437,#37438,#37439,#37440,#37441,#37442,
#37443,#37444,#37445,#37446,#37447,#37448,#37449,#37450,#37451,#37452,#37453,
#37454,#37455,#37456,#37457,#37458,#37459,#37460,#37461,#37462,#37463,#37464,
#37465,#37466,#37467,#37468,#37469,#37470,#37471,#37472,#37473,#37474,#37475,
#37476,#37477,#37478,#37479,#37480,#37481,#37482,#37483,#37484,#37485,#37486,
#37487,#37488,#37489,#37490,#37491,#37492,#37493,#37494,#37495,#37496,#37497,
#37498,#37499,#37500,#37501,#37502,#37503,#37504,#37505,#37506,#37507,#37508,
#37509,#37510,#37511,#37512,#37513,#37514,#37515,#37516,#37517,#37518,#37519,
#37520,#37521,#37522,#37523,#37524,#37525,#37526,#37527,#37528,#37529,#37530,
#37531,#37532,#37533,#37534,#37535,#37536,#37537,#37538,#37539),(#37540,
#37541,#37542,#37543,#37544,#37545,#37546,#37547,#37548,#37549,#37550,#37551,
#37552,#37553,#37554,#37555,#37556,#37557,#37558,#37559,#37560,#37561,#37562,
#37563,#37564,#37565,#37566,#37567,#37568,#37569,#37570,#37571,#37572,#37573,
#37574,#37575,#37576,#37577,#37578,#37579,#37580,#37581,#37582,#37583,#37584,
#37585,#37586,#37587,#37588,#37589,#37590,#37591,#37592,#37593,#37594,#37595,
#37596,#37597,#37598,#37599,#37600,#37601,#37602,#37603,#37604,#37605,#37606,
#37607,#37608,#37609,#37610,#37611,#37612,#37613,#37614,#37615,#37616,#37617,
#37618,#37619,#37620,#37621,#37622,#37623,#37624,#37625,#37626,#37627,#37628,
#37629,#37630,#37631,#37632,#37633,#37634,#37635,#37636,#37637,#37638,#37639,
#37640,#37641,#37642,#37643,#37644,#37645,#37646,#37647,#37648,#37649,#37650,
#37651,#37652,#37653,#37654,#37655,#37656,#37657,#37658,#37659,#37660,#37661),
(#37662,#37663,#37664,#37665,#37666,#37667,#37668,#37669,#37670,#37671,
#37672,#37673,#37674,#37675,#37676,#37677,#37678,#37679,#37680,#37681,#37682,
#37683,#37684,#37685,#37686,#37687,#37688,#37689,#37690,#37691,#37692,#37693,
#37694,#37695,#37696,#37697,#37698,#37699,#37700,#37701,#37702,#37703,#37704,
#37705,#37706,#37707,#37708,#37709,#37710,#37711,#37712,#37713,#37714,#37715,
#37716,#37717,#37718,#37719,#37720,#37721,#37722,#37723,#37724,#37725,#37726,
#37727,#37728,#37729,#37730,#37731,#37732,#37733,#37734,#37735,#37736,#37737,
#37738,#37739,#37740,#37741,#37742,#37743,#37744,#37745,#37746,#37747,#37748,
#37749,#37750,#37751,#37752,#37753,#37754,#37755,#37756,#37757,#37758,#37759,
#37760,#37761,#37762,#37763,#37764,#37765,#37766,#37767,#37768,#37769,#37770,
#37771,#37772,#37773,#37774,#37775,#37776,#37777,#37778,#37779,#37780,#37781,
#37782,#37783)),.UNSPECIFIED.,.F.,.F.,.F.,(4,4),(4,1,1,1,1,1,1,1,1,1,1,
1,1,1,1,1,1,1,1,1,1,1,1,1,1,1,1,1,1,1,1,1,1,1,1,1,1,1,1,1,1,1,1,1,1,1,1,
1,1,1,1,1,1,1,1,1,1,1,1,1,1,1,1,1,1,1,1,1,1,1,1,1,1,1,1,1,1,1,1,1,1,1,1,
1,1,1,1,1,1,1,1,1,1,1,1,1,1,1,1,1,1,1,1,1,1,1,1,1,1,1,1,1,1,1,1,1,1,1,1,
4),(0.,0.0448889834294937),(11.8615800042567,12.8590786597072,13.8565773151577,
14.8540759706082,15.8515746260587,16.8490732815092,17.8465719369597,18.8440705924102,
19.8415692478607,20.8390679033112,21.8365665587617,22.8340652142122,23.8315638696627,
24.8290625251132,25.8265611805637,26.8240598360142,27.8215584914647,28.8190571469152,
29.8165558023657,30.8140544578162,31.8115531132667,32.8090517687172,33.8065504241677,
34.8040490796182,35.8015477350687,36.7990463905192,37.7965450459697,38.7940437014202,
39.7915423568707,40.7890410123212,41.7865396677717,42.7840383232222,43.7815369786727,
44.7790356341232,45.7765342895737,46.7740329450242,47.7715316004747,48.7690302559252,
49.7665289113757,50.7640275668262,51.7615262222767,52.7590248777272,53.7565235331777,
54.7540221886282,55.7515208440787,56.7490194995292,57.7465181549797,58.7440168104302,
59.7415154658807,60.7390141213312,61.7365127767817,62.7340114322322,63.7315100876827,
64.7290087431332,65.7265073985837,66.7240060540342,67.7215047094847,68.7190033649352,
69.7165020203857,70.7140006758362,71.7114993312867,72.7089979867372,73.7064966421877,
74.7039952976382,75.7014939530887,76.6989926085392,77.6964912639897,78.6939899194402,
79.6914885748908,80.6889872303413,81.6864858857918,82.6839845412423,83.6814831966928,
84.6789818521433,85.6764805075938,86.6739791630443,87.6714778184948,88.6689764739453,
89.6664751293958,90.6639737848463,91.6614724402968,92.6589710957473,93.6564697511978,
94.6539684066483,95.6514670620988,96.6489657175493,97.6464643729998,98.6439630284503,
99.6414616839008,100.638960339351,101.636458994802,102.633957650252,103.631456305703,
104.628954961153,105.626453616604,106.623952272054,107.621450927505,108.618949582955,
109.616448238406,110.613946893856,111.611445549307,112.608944204757,113.606442860208,
114.603941515658,115.601440171109,116.598938826559,117.59643748201,118.59393613746,
119.591434792911,120.588933448361,121.586432103812,122.583930759262,123.581429414713,
124.578928070163,125.576426725614,126.573925381064,127.571424036515,128.568922691965,
129.566421347416,130.563920002866),.UNSPECIFIED.);
#249=B_SPLINE_SURFACE_WITH_KNOTS('',3,3,((#37891,#37892,#37893,#37894,#37895,
#37896,#37897,#37898,#37899,#37900,#37901,#37902,#37903,#37904,#37905,#37906,
#37907,#37908,#37909,#37910,#37911,#37912,#37913,#37914,#37915,#37916,#37917,
#37918,#37919,#37920,#37921,#37922,#37923,#37924,#37925,#37926,#37927,#37928,
#37929,#37930,#37931,#37932,#37933,#37934,#37935,#37936,#37937,#37938,#37939,
#37940,#37941,#37942,#37943,#37944,#37945,#37946,#37947,#37948,#37949,#37950,
#37951,#37952,#37953,#37954,#37955,#37956,#37957,#37958,#37959,#37960,#37961,
#37962,#37963,#37964,#37965,#37966,#37967,#37968,#37969,#37970,#37971,#37972,
#37973,#37974,#37975,#37976,#37977,#37978,#37979,#37980,#37981,#37982,#37983,
#37984,#37985,#37986,#37987,#37988,#37989,#37990,#37991,#37992,#37993,#37994,
#37995,#37996,#37997,#37998,#37999,#38000,#38001,#38002,#38003,#38004,#38005,
#38006,#38007,#38008,#38009,#38010,#38011,#38012),(#38013,#38014,#38015,
#38016,#38017,#38018,#38019,#38020,#38021,#38022,#38023,#38024,#38025,#38026,
#38027,#38028,#38029,#38030,#38031,#38032,#38033,#38034,#38035,#38036,#38037,
#38038,#38039,#38040,#38041,#38042,#38043,#38044,#38045,#38046,#38047,#38048,
#38049,#38050,#38051,#38052,#38053,#38054,#38055,#38056,#38057,#38058,#38059,
#38060,#38061,#38062,#38063,#38064,#38065,#38066,#38067,#38068,#38069,#38070,
#38071,#38072,#38073,#38074,#38075,#38076,#38077,#38078,#38079,#38080,#38081,
#38082,#38083,#38084,#38085,#38086,#38087,#38088,#38089,#38090,#38091,#38092,
#38093,#38094,#38095,#38096,#38097,#38098,#38099,#38100,#38101,#38102,#38103,
#38104,#38105,#38106,#38107,#38108,#38109,#38110,#38111,#38112,#38113,#38114,
#38115,#38116,#38117,#38118,#38119,#38120,#38121,#38122,#38123,#38124,#38125,
#38126,#38127,#38128,#38129,#38130,#38131,#38132,#38133,#38134),(#38135,
#38136,#38137,#38138,#38139,#38140,#38141,#38142,#38143,#38144,#38145,#38146,
#38147,#38148,#38149,#38150,#38151,#38152,#38153,#38154,#38155,#38156,#38157,
#38158,#38159,#38160,#38161,#38162,#38163,#38164,#38165,#38166,#38167,#38168,
#38169,#38170,#38171,#38172,#38173,#38174,#38175,#38176,#38177,#38178,#38179,
#38180,#38181,#38182,#38183,#38184,#38185,#38186,#38187,#38188,#38189,#38190,
#38191,#38192,#38193,#38194,#38195,#38196,#38197,#38198,#38199,#38200,#38201,
#38202,#38203,#38204,#38205,#38206,#38207,#38208,#38209,#38210,#38211,#38212,
#38213,#38214,#38215,#38216,#38217,#38218,#38219,#38220,#38221,#38222,#38223,
#38224,#38225,#38226,#38227,#38228,#38229,#38230,#38231,#38232,#38233,#38234,
#38235,#38236,#38237,#38238,#38239,#38240,#38241,#38242,#38243,#38244,#38245,
#38246,#38247,#38248,#38249,#38250,#38251,#38252,#38253,#38254,#38255,#38256),
(#38257,#38258,#38259,#38260,#38261,#38262,#38263,#38264,#38265,#38266,
#38267,#38268,#38269,#38270,#38271,#38272,#38273,#38274,#38275,#38276,#38277,
#38278,#38279,#38280,#38281,#38282,#38283,#38284,#38285,#38286,#38287,#38288,
#38289,#38290,#38291,#38292,#38293,#38294,#38295,#38296,#38297,#38298,#38299,
#38300,#38301,#38302,#38303,#38304,#38305,#38306,#38307,#38308,#38309,#38310,
#38311,#38312,#38313,#38314,#38315,#38316,#38317,#38318,#38319,#38320,#38321,
#38322,#38323,#38324,#38325,#38326,#38327,#38328,#38329,#38330,#38331,#38332,
#38333,#38334,#38335,#38336,#38337,#38338,#38339,#38340,#38341,#38342,#38343,
#38344,#38345,#38346,#38347,#38348,#38349,#38350,#38351,#38352,#38353,#38354,
#38355,#38356,#38357,#38358,#38359,#38360,#38361,#38362,#38363,#38364,#38365,
#38366,#38367,#38368,#38369,#38370,#38371,#38372,#38373,#38374,#38375,#38376,
#38377,#38378)),.UNSPECIFIED.,.F.,.F.,.F.,(4,4),(4,1,1,1,1,1,1,1,1,1,1,
1,1,1,1,1,1,1,1,1,1,1,1,1,1,1,1,1,1,1,1,1,1,1,1,1,1,1,1,1,1,1,1,1,1,1,1,
1,1,1,1,1,1,1,1,1,1,1,1,1,1,1,1,1,1,1,1,1,1,1,1,1,1,1,1,1,1,1,1,1,1,1,1,
1,1,1,1,1,1,1,1,1,1,1,1,1,1,1,1,1,1,1,1,1,1,1,1,1,1,1,1,1,1,1,1,1,1,1,1,
4),(0.,0.0448889834294937),(14.3981410127769,15.3956396682274,16.3931383236779,
17.3906369791284,18.3881356345789,19.3856342900294,20.3831329454799,21.3806316009304,
22.3781302563809,23.3756289118314,24.3731275672819,25.3706262227324,26.3681248781829,
27.3656235336334,28.3631221890839,29.3606208445344,30.3581194999849,31.3556181554354,
32.3531168108859,33.3506154663364,34.3481141217869,35.3456127772374,36.3431114326879,
37.3406100881384,38.3381087435889,39.3356073990394,40.3331060544899,41.3306047099404,
42.3281033653909,43.3256020208414,44.3231006762919,45.3205993317424,46.3180979871929,
47.3155966426434,48.3130952980939,49.3105939535444,50.3080926089949,51.3055912644454,
52.3030899198959,53.3005885753464,54.2980872307969,55.2955858862474,56.2930845416979,
57.2905831971484,58.2880818525989,59.2855805080494,60.2830791634999,61.2805778189504,
62.2780764744009,63.2755751298514,64.2730737853019,65.2705724407524,66.2680710962029,
67.2655697516534,68.2630684071039,69.2605670625544,70.2580657180049,71.2555643734554,
72.2530630289059,73.2505616843565,74.248060339807,75.2455589952575,76.243057650708,
77.2405563061585,78.238054961609,79.2355536170595,80.23305227251,81.2305509279605,
82.228049583411,83.2255482388615,84.223046894312,85.2205455497625,86.218044205213,
87.2155428606635,88.213041516114,89.2105401715645,90.208038827015,91.2055374824655,
92.203036137916,93.2005347933665,94.198033448817,95.1955321042675,96.193030759718,
97.1905294151685,98.188028070619,99.1855267260695,100.18302538152,101.18052403697,
102.178022692421,103.175521347871,104.173020003322,105.170518658772,106.168017314223,
107.165515969673,108.163014625124,109.160513280574,110.158011936025,111.155510591476,
112.153009246926,113.150507902377,114.148006557827,115.145505213278,116.143003868728,
117.140502524179,118.138001179629,119.13549983508,120.13299849053,121.130497145981,
122.127995801431,123.125494456882,124.122993112332,125.120491767783,126.117990423233,
127.115489078684,128.112987734134,129.110486389585,130.107985045035,131.105483700486,
132.102982355936,133.100481011387),.UNSPECIFIED.);
#250=B_SPLINE_SURFACE_WITH_KNOTS('',3,3,((#38683,#38684,#38685,#38686,#38687,
#38688,#38689,#38690,#38691,#38692,#38693,#38694,#38695,#38696,#38697,#38698,
#38699,#38700,#38701,#38702,#38703,#38704,#38705,#38706,#38707,#38708,#38709,
#38710,#38711,#38712,#38713,#38714,#38715,#38716,#38717,#38718,#38719,#38720,
#38721,#38722,#38723,#38724,#38725,#38726,#38727,#38728,#38729,#38730,#38731,
#38732,#38733,#38734,#38735,#38736,#38737,#38738,#38739,#38740,#38741,#38742,
#38743,#38744,#38745,#38746,#38747,#38748,#38749,#38750,#38751,#38752,#38753,
#38754,#38755,#38756,#38757,#38758,#38759,#38760,#38761,#38762,#38763,#38764,
#38765,#38766,#38767,#38768,#38769,#38770,#38771,#38772,#38773,#38774,#38775,
#38776,#38777,#38778,#38779,#38780,#38781,#38782,#38783,#38784,#38785,#38786,
#38787,#38788,#38789,#38790,#38791,#38792,#38793,#38794,#38795,#38796,#38797,
#38798,#38799,#38800,#38801,#38802,#38803,#38804),(#38805,#38806,#38807,
#38808,#38809,#38810,#38811,#38812,#38813,#38814,#38815,#38816,#38817,#38818,
#38819,#38820,#38821,#38822,#38823,#38824,#38825,#38826,#38827,#38828,#38829,
#38830,#38831,#38832,#38833,#38834,#38835,#38836,#38837,#38838,#38839,#38840,
#38841,#38842,#38843,#38844,#38845,#38846,#38847,#38848,#38849,#38850,#38851,
#38852,#38853,#38854,#38855,#38856,#38857,#38858,#38859,#38860,#38861,#38862,
#38863,#38864,#38865,#38866,#38867,#38868,#38869,#38870,#38871,#38872,#38873,
#38874,#38875,#38876,#38877,#38878,#38879,#38880,#38881,#38882,#38883,#38884,
#38885,#38886,#38887,#38888,#38889,#38890,#38891,#38892,#38893,#38894,#38895,
#38896,#38897,#38898,#38899,#38900,#38901,#38902,#38903,#38904,#38905,#38906,
#38907,#38908,#38909,#38910,#38911,#38912,#38913,#38914,#38915,#38916,#38917,
#38918,#38919,#38920,#38921,#38922,#38923,#38924,#38925,#38926),(#38927,
#38928,#38929,#38930,#38931,#38932,#38933,#38934,#38935,#38936,#38937,#38938,
#38939,#38940,#38941,#38942,#38943,#38944,#38945,#38946,#38947,#38948,#38949,
#38950,#38951,#38952,#38953,#38954,#38955,#38956,#38957,#38958,#38959,#38960,
#38961,#38962,#38963,#38964,#38965,#38966,#38967,#38968,#38969,#38970,#38971,
#38972,#38973,#38974,#38975,#38976,#38977,#38978,#38979,#38980,#38981,#38982,
#38983,#38984,#38985,#38986,#38987,#38988,#38989,#38990,#38991,#38992,#38993,
#38994,#38995,#38996,#38997,#38998,#38999,#39000,#39001,#39002,#39003,#39004,
#39005,#39006,#39007,#39008,#39009,#39010,#39011,#39012,#39013,#39014,#39015,
#39016,#39017,#39018,#39019,#39020,#39021,#39022,#39023,#39024,#39025,#39026,
#39027,#39028,#39029,#39030,#39031,#39032,#39033,#39034,#39035,#39036,#39037,
#39038,#39039,#39040,#39041,#39042,#39043,#39044,#39045,#39046,#39047,#39048),
(#39049,#39050,#39051,#39052,#39053,#39054,#39055,#39056,#39057,#39058,
#39059,#39060,#39061,#39062,#39063,#39064,#39065,#39066,#39067,#39068,#39069,
#39070,#39071,#39072,#39073,#39074,#39075,#39076,#39077,#39078,#39079,#39080,
#39081,#39082,#39083,#39084,#39085,#39086,#39087,#39088,#39089,#39090,#39091,
#39092,#39093,#39094,#39095,#39096,#39097,#39098,#39099,#39100,#39101,#39102,
#39103,#39104,#39105,#39106,#39107,#39108,#39109,#39110,#39111,#39112,#39113,
#39114,#39115,#39116,#39117,#39118,#39119,#39120,#39121,#39122,#39123,#39124,
#39125,#39126,#39127,#39128,#39129,#39130,#39131,#39132,#39133,#39134,#39135,
#39136,#39137,#39138,#39139,#39140,#39141,#39142,#39143,#39144,#39145,#39146,
#39147,#39148,#39149,#39150,#39151,#39152,#39153,#39154,#39155,#39156,#39157,
#39158,#39159,#39160,#39161,#39162,#39163,#39164,#39165,#39166,#39167,#39168,
#39169,#39170)),.UNSPECIFIED.,.F.,.F.,.F.,(4,4),(4,1,1,1,1,1,1,1,1,1,1,
1,1,1,1,1,1,1,1,1,1,1,1,1,1,1,1,1,1,1,1,1,1,1,1,1,1,1,1,1,1,1,1,1,1,1,1,
1,1,1,1,1,1,1,1,1,1,1,1,1,1,1,1,1,1,1,1,1,1,1,1,1,1,1,1,1,1,1,1,1,1,1,1,
1,1,1,1,1,1,1,1,1,1,1,1,1,1,1,1,1,1,1,1,1,1,1,1,1,1,1,1,1,1,1,1,1,1,1,1,
4),(0.,0.0448889834294937),(11.8615800042567,12.8590786597072,13.8565773151577,
14.8540759706082,15.8515746260587,16.8490732815092,17.8465719369597,18.8440705924102,
19.8415692478607,20.8390679033112,21.8365665587617,22.8340652142122,23.8315638696627,
24.8290625251132,25.8265611805637,26.8240598360142,27.8215584914647,28.8190571469152,
29.8165558023657,30.8140544578162,31.8115531132667,32.8090517687172,33.8065504241677,
34.8040490796182,35.8015477350687,36.7990463905192,37.7965450459697,38.7940437014202,
39.7915423568707,40.7890410123212,41.7865396677717,42.7840383232222,43.7815369786727,
44.7790356341232,45.7765342895737,46.7740329450242,47.7715316004747,48.7690302559252,
49.7665289113757,50.7640275668262,51.7615262222767,52.7590248777272,53.7565235331777,
54.7540221886282,55.7515208440787,56.7490194995292,57.7465181549797,58.7440168104302,
59.7415154658807,60.7390141213312,61.7365127767817,62.7340114322322,63.7315100876827,
64.7290087431332,65.7265073985837,66.7240060540342,67.7215047094847,68.7190033649352,
69.7165020203857,70.7140006758362,71.7114993312867,72.7089979867372,73.7064966421877,
74.7039952976382,75.7014939530887,76.6989926085392,77.6964912639897,78.6939899194402,
79.6914885748908,80.6889872303413,81.6864858857918,82.6839845412423,83.6814831966928,
84.6789818521433,85.6764805075938,86.6739791630443,87.6714778184948,88.6689764739453,
89.6664751293958,90.6639737848463,91.6614724402968,92.6589710957473,93.6564697511978,
94.6539684066483,95.6514670620988,96.6489657175493,97.6464643729998,98.6439630284503,
99.6414616839008,100.638960339351,101.636458994802,102.633957650252,103.631456305703,
104.628954961153,105.626453616604,106.623952272054,107.621450927505,108.618949582955,
109.616448238406,110.613946893856,111.611445549307,112.608944204757,113.606442860208,
114.603941515658,115.601440171109,116.598938826559,117.59643748201,118.59393613746,
119.591434792911,120.588933448361,121.586432103812,122.583930759262,123.581429414713,
124.578928070163,125.576426725614,126.573925381064,127.571424036515,128.568922691965,
129.566421347416,130.563920002866),.UNSPECIFIED.);
#251=B_SPLINE_SURFACE_WITH_KNOTS('',3,3,((#39278,#39279,#39280,#39281,#39282,
#39283,#39284,#39285,#39286,#39287,#39288,#39289,#39290,#39291,#39292,#39293,
#39294,#39295,#39296,#39297,#39298,#39299,#39300,#39301,#39302,#39303,#39304,
#39305,#39306,#39307,#39308,#39309,#39310,#39311,#39312,#39313,#39314,#39315,
#39316,#39317,#39318,#39319,#39320,#39321,#39322,#39323,#39324,#39325,#39326,
#39327,#39328,#39329,#39330,#39331,#39332,#39333,#39334,#39335,#39336,#39337,
#39338,#39339,#39340,#39341,#39342,#39343,#39344,#39345,#39346,#39347,#39348,
#39349,#39350,#39351,#39352,#39353,#39354,#39355,#39356,#39357,#39358,#39359,
#39360,#39361,#39362,#39363,#39364,#39365,#39366,#39367,#39368,#39369,#39370,
#39371,#39372,#39373,#39374,#39375,#39376,#39377,#39378,#39379,#39380,#39381,
#39382,#39383,#39384,#39385,#39386,#39387,#39388,#39389,#39390,#39391,#39392,
#39393,#39394,#39395,#39396,#39397,#39398,#39399),(#39400,#39401,#39402,
#39403,#39404,#39405,#39406,#39407,#39408,#39409,#39410,#39411,#39412,#39413,
#39414,#39415,#39416,#39417,#39418,#39419,#39420,#39421,#39422,#39423,#39424,
#39425,#39426,#39427,#39428,#39429,#39430,#39431,#39432,#39433,#39434,#39435,
#39436,#39437,#39438,#39439,#39440,#39441,#39442,#39443,#39444,#39445,#39446,
#39447,#39448,#39449,#39450,#39451,#39452,#39453,#39454,#39455,#39456,#39457,
#39458,#39459,#39460,#39461,#39462,#39463,#39464,#39465,#39466,#39467,#39468,
#39469,#39470,#39471,#39472,#39473,#39474,#39475,#39476,#39477,#39478,#39479,
#39480,#39481,#39482,#39483,#39484,#39485,#39486,#39487,#39488,#39489,#39490,
#39491,#39492,#39493,#39494,#39495,#39496,#39497,#39498,#39499,#39500,#39501,
#39502,#39503,#39504,#39505,#39506,#39507,#39508,#39509,#39510,#39511,#39512,
#39513,#39514,#39515,#39516,#39517,#39518,#39519,#39520,#39521),(#39522,
#39523,#39524,#39525,#39526,#39527,#39528,#39529,#39530,#39531,#39532,#39533,
#39534,#39535,#39536,#39537,#39538,#39539,#39540,#39541,#39542,#39543,#39544,
#39545,#39546,#39547,#39548,#39549,#39550,#39551,#39552,#39553,#39554,#39555,
#39556,#39557,#39558,#39559,#39560,#39561,#39562,#39563,#39564,#39565,#39566,
#39567,#39568,#39569,#39570,#39571,#39572,#39573,#39574,#39575,#39576,#39577,
#39578,#39579,#39580,#39581,#39582,#39583,#39584,#39585,#39586,#39587,#39588,
#39589,#39590,#39591,#39592,#39593,#39594,#39595,#39596,#39597,#39598,#39599,
#39600,#39601,#39602,#39603,#39604,#39605,#39606,#39607,#39608,#39609,#39610,
#39611,#39612,#39613,#39614,#39615,#39616,#39617,#39618,#39619,#39620,#39621,
#39622,#39623,#39624,#39625,#39626,#39627,#39628,#39629,#39630,#39631,#39632,
#39633,#39634,#39635,#39636,#39637,#39638,#39639,#39640,#39641,#39642,#39643),
(#39644,#39645,#39646,#39647,#39648,#39649,#39650,#39651,#39652,#39653,
#39654,#39655,#39656,#39657,#39658,#39659,#39660,#39661,#39662,#39663,#39664,
#39665,#39666,#39667,#39668,#39669,#39670,#39671,#39672,#39673,#39674,#39675,
#39676,#39677,#39678,#39679,#39680,#39681,#39682,#39683,#39684,#39685,#39686,
#39687,#39688,#39689,#39690,#39691,#39692,#39693,#39694,#39695,#39696,#39697,
#39698,#39699,#39700,#39701,#39702,#39703,#39704,#39705,#39706,#39707,#39708,
#39709,#39710,#39711,#39712,#39713,#39714,#39715,#39716,#39717,#39718,#39719,
#39720,#39721,#39722,#39723,#39724,#39725,#39726,#39727,#39728,#39729,#39730,
#39731,#39732,#39733,#39734,#39735,#39736,#39737,#39738,#39739,#39740,#39741,
#39742,#39743,#39744,#39745,#39746,#39747,#39748,#39749,#39750,#39751,#39752,
#39753,#39754,#39755,#39756,#39757,#39758,#39759,#39760,#39761,#39762,#39763,
#39764,#39765)),.UNSPECIFIED.,.F.,.F.,.F.,(4,4),(4,1,1,1,1,1,1,1,1,1,1,
1,1,1,1,1,1,1,1,1,1,1,1,1,1,1,1,1,1,1,1,1,1,1,1,1,1,1,1,1,1,1,1,1,1,1,1,
1,1,1,1,1,1,1,1,1,1,1,1,1,1,1,1,1,1,1,1,1,1,1,1,1,1,1,1,1,1,1,1,1,1,1,1,
1,1,1,1,1,1,1,1,1,1,1,1,1,1,1,1,1,1,1,1,1,1,1,1,1,1,1,1,1,1,1,1,1,1,1,1,
4),(0.,0.0448889834294937),(14.3981410127769,15.3956396682274,16.3931383236779,
17.3906369791284,18.3881356345789,19.3856342900294,20.3831329454799,21.3806316009304,
22.3781302563809,23.3756289118314,24.3731275672819,25.3706262227324,26.3681248781829,
27.3656235336334,28.3631221890839,29.3606208445344,30.3581194999849,31.3556181554354,
32.3531168108859,33.3506154663364,34.3481141217869,35.3456127772374,36.3431114326879,
37.3406100881384,38.3381087435889,39.3356073990394,40.3331060544899,41.3306047099404,
42.3281033653909,43.3256020208414,44.3231006762919,45.3205993317424,46.3180979871929,
47.3155966426434,48.3130952980939,49.3105939535444,50.3080926089949,51.3055912644454,
52.3030899198959,53.3005885753464,54.2980872307969,55.2955858862474,56.2930845416979,
57.2905831971484,58.2880818525989,59.2855805080494,60.2830791634999,61.2805778189504,
62.2780764744009,63.2755751298514,64.2730737853019,65.2705724407524,66.2680710962029,
67.2655697516534,68.2630684071039,69.2605670625544,70.2580657180049,71.2555643734554,
72.2530630289059,73.2505616843565,74.248060339807,75.2455589952575,76.243057650708,
77.2405563061585,78.238054961609,79.2355536170595,80.23305227251,81.2305509279605,
82.228049583411,83.2255482388615,84.223046894312,85.2205455497625,86.218044205213,
87.2155428606635,88.213041516114,89.2105401715645,90.208038827015,91.2055374824655,
92.203036137916,93.2005347933665,94.198033448817,95.1955321042675,96.193030759718,
97.1905294151685,98.188028070619,99.1855267260695,100.18302538152,101.18052403697,
102.178022692421,103.175521347871,104.173020003322,105.170518658772,106.168017314223,
107.165515969673,108.163014625124,109.160513280574,110.158011936025,111.155510591476,
112.153009246926,113.150507902377,114.148006557827,115.145505213278,116.143003868728,
117.140502524179,118.138001179629,119.13549983508,120.13299849053,121.130497145981,
122.127995801431,123.125494456882,124.122993112332,125.120491767783,126.117990423233,
127.115489078684,128.112987734134,129.110486389585,130.107985045035,131.105483700486,
132.102982355936,133.100481011387),.UNSPECIFIED.);
#252=B_SPLINE_SURFACE_WITH_KNOTS('',3,3,((#40070,#40071,#40072,#40073,#40074,
#40075,#40076,#40077,#40078,#40079,#40080,#40081,#40082,#40083,#40084,#40085,
#40086,#40087,#40088,#40089,#40090,#40091,#40092,#40093,#40094,#40095,#40096,
#40097,#40098,#40099,#40100,#40101,#40102,#40103,#40104,#40105,#40106,#40107,
#40108,#40109,#40110,#40111,#40112,#40113,#40114,#40115,#40116,#40117,#40118,
#40119,#40120,#40121,#40122,#40123,#40124,#40125,#40126,#40127,#40128,#40129,
#40130,#40131,#40132,#40133,#40134,#40135,#40136,#40137,#40138,#40139,#40140,
#40141,#40142,#40143,#40144,#40145,#40146,#40147,#40148,#40149,#40150,#40151,
#40152,#40153,#40154,#40155,#40156,#40157,#40158,#40159,#40160,#40161,#40162,
#40163,#40164,#40165,#40166,#40167,#40168,#40169,#40170,#40171,#40172,#40173,
#40174,#40175,#40176,#40177,#40178,#40179,#40180,#40181,#40182,#40183,#40184,
#40185,#40186,#40187,#40188,#40189,#40190,#40191),(#40192,#40193,#40194,
#40195,#40196,#40197,#40198,#40199,#40200,#40201,#40202,#40203,#40204,#40205,
#40206,#40207,#40208,#40209,#40210,#40211,#40212,#40213,#40214,#40215,#40216,
#40217,#40218,#40219,#40220,#40221,#40222,#40223,#40224,#40225,#40226,#40227,
#40228,#40229,#40230,#40231,#40232,#40233,#40234,#40235,#40236,#40237,#40238,
#40239,#40240,#40241,#40242,#40243,#40244,#40245,#40246,#40247,#40248,#40249,
#40250,#40251,#40252,#40253,#40254,#40255,#40256,#40257,#40258,#40259,#40260,
#40261,#40262,#40263,#40264,#40265,#40266,#40267,#40268,#40269,#40270,#40271,
#40272,#40273,#40274,#40275,#40276,#40277,#40278,#40279,#40280,#40281,#40282,
#40283,#40284,#40285,#40286,#40287,#40288,#40289,#40290,#40291,#40292,#40293,
#40294,#40295,#40296,#40297,#40298,#40299,#40300,#40301,#40302,#40303,#40304,
#40305,#40306,#40307,#40308,#40309,#40310,#40311,#40312,#40313),(#40314,
#40315,#40316,#40317,#40318,#40319,#40320,#40321,#40322,#40323,#40324,#40325,
#40326,#40327,#40328,#40329,#40330,#40331,#40332,#40333,#40334,#40335,#40336,
#40337,#40338,#40339,#40340,#40341,#40342,#40343,#40344,#40345,#40346,#40347,
#40348,#40349,#40350,#40351,#40352,#40353,#40354,#40355,#40356,#40357,#40358,
#40359,#40360,#40361,#40362,#40363,#40364,#40365,#40366,#40367,#40368,#40369,
#40370,#40371,#40372,#40373,#40374,#40375,#40376,#40377,#40378,#40379,#40380,
#40381,#40382,#40383,#40384,#40385,#40386,#40387,#40388,#40389,#40390,#40391,
#40392,#40393,#40394,#40395,#40396,#40397,#40398,#40399,#40400,#40401,#40402,
#40403,#40404,#40405,#40406,#40407,#40408,#40409,#40410,#40411,#40412,#40413,
#40414,#40415,#40416,#40417,#40418,#40419,#40420,#40421,#40422,#40423,#40424,
#40425,#40426,#40427,#40428,#40429,#40430,#40431,#40432,#40433,#40434,#40435),
(#40436,#40437,#40438,#40439,#40440,#40441,#40442,#40443,#40444,#40445,
#40446,#40447,#40448,#40449,#40450,#40451,#40452,#40453,#40454,#40455,#40456,
#40457,#40458,#40459,#40460,#40461,#40462,#40463,#40464,#40465,#40466,#40467,
#40468,#40469,#40470,#40471,#40472,#40473,#40474,#40475,#40476,#40477,#40478,
#40479,#40480,#40481,#40482,#40483,#40484,#40485,#40486,#40487,#40488,#40489,
#40490,#40491,#40492,#40493,#40494,#40495,#40496,#40497,#40498,#40499,#40500,
#40501,#40502,#40503,#40504,#40505,#40506,#40507,#40508,#40509,#40510,#40511,
#40512,#40513,#40514,#40515,#40516,#40517,#40518,#40519,#40520,#40521,#40522,
#40523,#40524,#40525,#40526,#40527,#40528,#40529,#40530,#40531,#40532,#40533,
#40534,#40535,#40536,#40537,#40538,#40539,#40540,#40541,#40542,#40543,#40544,
#40545,#40546,#40547,#40548,#40549,#40550,#40551,#40552,#40553,#40554,#40555,
#40556,#40557)),.UNSPECIFIED.,.F.,.F.,.F.,(4,4),(4,1,1,1,1,1,1,1,1,1,1,
1,1,1,1,1,1,1,1,1,1,1,1,1,1,1,1,1,1,1,1,1,1,1,1,1,1,1,1,1,1,1,1,1,1,1,1,
1,1,1,1,1,1,1,1,1,1,1,1,1,1,1,1,1,1,1,1,1,1,1,1,1,1,1,1,1,1,1,1,1,1,1,1,
1,1,1,1,1,1,1,1,1,1,1,1,1,1,1,1,1,1,1,1,1,1,1,1,1,1,1,1,1,1,1,1,1,1,1,1,
4),(0.,0.0448889834294937),(11.8615800042567,12.8590786597072,13.8565773151577,
14.8540759706082,15.8515746260587,16.8490732815092,17.8465719369597,18.8440705924102,
19.8415692478607,20.8390679033112,21.8365665587617,22.8340652142122,23.8315638696627,
24.8290625251132,25.8265611805637,26.8240598360142,27.8215584914647,28.8190571469152,
29.8165558023657,30.8140544578162,31.8115531132667,32.8090517687172,33.8065504241677,
34.8040490796182,35.8015477350687,36.7990463905192,37.7965450459697,38.7940437014202,
39.7915423568707,40.7890410123212,41.7865396677717,42.7840383232222,43.7815369786727,
44.7790356341232,45.7765342895737,46.7740329450242,47.7715316004747,48.7690302559252,
49.7665289113757,50.7640275668262,51.7615262222767,52.7590248777272,53.7565235331777,
54.7540221886282,55.7515208440787,56.7490194995292,57.7465181549797,58.7440168104302,
59.7415154658807,60.7390141213312,61.7365127767817,62.7340114322322,63.7315100876827,
64.7290087431332,65.7265073985837,66.7240060540342,67.7215047094847,68.7190033649352,
69.7165020203857,70.7140006758362,71.7114993312867,72.7089979867372,73.7064966421877,
74.7039952976382,75.7014939530887,76.6989926085392,77.6964912639897,78.6939899194402,
79.6914885748908,80.6889872303413,81.6864858857918,82.6839845412423,83.6814831966928,
84.6789818521433,85.6764805075938,86.6739791630443,87.6714778184948,88.6689764739453,
89.6664751293958,90.6639737848463,91.6614724402968,92.6589710957473,93.6564697511978,
94.6539684066483,95.6514670620988,96.6489657175493,97.6464643729998,98.6439630284503,
99.6414616839008,100.638960339351,101.636458994802,102.633957650252,103.631456305703,
104.628954961153,105.626453616604,106.623952272054,107.621450927505,108.618949582955,
109.616448238406,110.613946893856,111.611445549307,112.608944204757,113.606442860208,
114.603941515658,115.601440171109,116.598938826559,117.59643748201,118.59393613746,
119.591434792911,120.588933448361,121.586432103812,122.583930759262,123.581429414713,
124.578928070163,125.576426725614,126.573925381064,127.571424036515,128.568922691965,
129.566421347416,130.563920002866),.UNSPECIFIED.);
#253=B_SPLINE_SURFACE_WITH_KNOTS('',3,3,((#40665,#40666,#40667,#40668,#40669,
#40670,#40671,#40672,#40673,#40674,#40675,#40676,#40677,#40678,#40679,#40680,
#40681,#40682,#40683,#40684,#40685,#40686,#40687,#40688,#40689,#40690,#40691,
#40692,#40693,#40694,#40695,#40696,#40697,#40698,#40699,#40700,#40701,#40702,
#40703,#40704,#40705,#40706,#40707,#40708,#40709,#40710,#40711,#40712,#40713,
#40714,#40715,#40716,#40717,#40718,#40719,#40720,#40721,#40722,#40723,#40724,
#40725,#40726,#40727,#40728,#40729,#40730,#40731,#40732,#40733,#40734,#40735,
#40736,#40737,#40738,#40739,#40740,#40741,#40742,#40743,#40744,#40745,#40746,
#40747,#40748,#40749,#40750,#40751,#40752,#40753,#40754,#40755,#40756,#40757,
#40758,#40759,#40760,#40761,#40762,#40763,#40764,#40765,#40766,#40767,#40768,
#40769,#40770,#40771,#40772,#40773,#40774,#40775,#40776,#40777,#40778,#40779,
#40780,#40781,#40782,#40783,#40784,#40785,#40786),(#40787,#40788,#40789,
#40790,#40791,#40792,#40793,#40794,#40795,#40796,#40797,#40798,#40799,#40800,
#40801,#40802,#40803,#40804,#40805,#40806,#40807,#40808,#40809,#40810,#40811,
#40812,#40813,#40814,#40815,#40816,#40817,#40818,#40819,#40820,#40821,#40822,
#40823,#40824,#40825,#40826,#40827,#40828,#40829,#40830,#40831,#40832,#40833,
#40834,#40835,#40836,#40837,#40838,#40839,#40840,#40841,#40842,#40843,#40844,
#40845,#40846,#40847,#40848,#40849,#40850,#40851,#40852,#40853,#40854,#40855,
#40856,#40857,#40858,#40859,#40860,#40861,#40862,#40863,#40864,#40865,#40866,
#40867,#40868,#40869,#40870,#40871,#40872,#40873,#40874,#40875,#40876,#40877,
#40878,#40879,#40880,#40881,#40882,#40883,#40884,#40885,#40886,#40887,#40888,
#40889,#40890,#40891,#40892,#40893,#40894,#40895,#40896,#40897,#40898,#40899,
#40900,#40901,#40902,#40903,#40904,#40905,#40906,#40907,#40908),(#40909,
#40910,#40911,#40912,#40913,#40914,#40915,#40916,#40917,#40918,#40919,#40920,
#40921,#40922,#40923,#40924,#40925,#40926,#40927,#40928,#40929,#40930,#40931,
#40932,#40933,#40934,#40935,#40936,#40937,#40938,#40939,#40940,#40941,#40942,
#40943,#40944,#40945,#40946,#40947,#40948,#40949,#40950,#40951,#40952,#40953,
#40954,#40955,#40956,#40957,#40958,#40959,#40960,#40961,#40962,#40963,#40964,
#40965,#40966,#40967,#40968,#40969,#40970,#40971,#40972,#40973,#40974,#40975,
#40976,#40977,#40978,#40979,#40980,#40981,#40982,#40983,#40984,#40985,#40986,
#40987,#40988,#40989,#40990,#40991,#40992,#40993,#40994,#40995,#40996,#40997,
#40998,#40999,#41000,#41001,#41002,#41003,#41004,#41005,#41006,#41007,#41008,
#41009,#41010,#41011,#41012,#41013,#41014,#41015,#41016,#41017,#41018,#41019,
#41020,#41021,#41022,#41023,#41024,#41025,#41026,#41027,#41028,#41029,#41030),
(#41031,#41032,#41033,#41034,#41035,#41036,#41037,#41038,#41039,#41040,
#41041,#41042,#41043,#41044,#41045,#41046,#41047,#41048,#41049,#41050,#41051,
#41052,#41053,#41054,#41055,#41056,#41057,#41058,#41059,#41060,#41061,#41062,
#41063,#41064,#41065,#41066,#41067,#41068,#41069,#41070,#41071,#41072,#41073,
#41074,#41075,#41076,#41077,#41078,#41079,#41080,#41081,#41082,#41083,#41084,
#41085,#41086,#41087,#41088,#41089,#41090,#41091,#41092,#41093,#41094,#41095,
#41096,#41097,#41098,#41099,#41100,#41101,#41102,#41103,#41104,#41105,#41106,
#41107,#41108,#41109,#41110,#41111,#41112,#41113,#41114,#41115,#41116,#41117,
#41118,#41119,#41120,#41121,#41122,#41123,#41124,#41125,#41126,#41127,#41128,
#41129,#41130,#41131,#41132,#41133,#41134,#41135,#41136,#41137,#41138,#41139,
#41140,#41141,#41142,#41143,#41144,#41145,#41146,#41147,#41148,#41149,#41150,
#41151,#41152)),.UNSPECIFIED.,.F.,.F.,.F.,(4,4),(4,1,1,1,1,1,1,1,1,1,1,
1,1,1,1,1,1,1,1,1,1,1,1,1,1,1,1,1,1,1,1,1,1,1,1,1,1,1,1,1,1,1,1,1,1,1,1,
1,1,1,1,1,1,1,1,1,1,1,1,1,1,1,1,1,1,1,1,1,1,1,1,1,1,1,1,1,1,1,1,1,1,1,1,
1,1,1,1,1,1,1,1,1,1,1,1,1,1,1,1,1,1,1,1,1,1,1,1,1,1,1,1,1,1,1,1,1,1,1,1,
4),(0.,0.0448889834294937),(14.3981410127769,15.3956396682274,16.3931383236779,
17.3906369791284,18.3881356345789,19.3856342900294,20.3831329454799,21.3806316009304,
22.3781302563809,23.3756289118314,24.3731275672819,25.3706262227324,26.3681248781829,
27.3656235336334,28.3631221890839,29.3606208445344,30.3581194999849,31.3556181554354,
32.3531168108859,33.3506154663364,34.3481141217869,35.3456127772374,36.3431114326879,
37.3406100881384,38.3381087435889,39.3356073990394,40.3331060544899,41.3306047099404,
42.3281033653909,43.3256020208414,44.3231006762919,45.3205993317424,46.3180979871929,
47.3155966426434,48.3130952980939,49.3105939535444,50.3080926089949,51.3055912644454,
52.3030899198959,53.3005885753464,54.2980872307969,55.2955858862474,56.2930845416979,
57.2905831971484,58.2880818525989,59.2855805080494,60.2830791634999,61.2805778189504,
62.2780764744009,63.2755751298514,64.2730737853019,65.2705724407524,66.2680710962029,
67.2655697516534,68.2630684071039,69.2605670625544,70.2580657180049,71.2555643734554,
72.2530630289059,73.2505616843565,74.248060339807,75.2455589952575,76.243057650708,
77.2405563061585,78.238054961609,79.2355536170595,80.23305227251,81.2305509279605,
82.228049583411,83.2255482388615,84.223046894312,85.2205455497625,86.218044205213,
87.2155428606635,88.213041516114,89.2105401715645,90.208038827015,91.2055374824655,
92.203036137916,93.2005347933665,94.198033448817,95.1955321042675,96.193030759718,
97.1905294151685,98.188028070619,99.1855267260695,100.18302538152,101.18052403697,
102.178022692421,103.175521347871,104.173020003322,105.170518658772,106.168017314223,
107.165515969673,108.163014625124,109.160513280574,110.158011936025,111.155510591476,
112.153009246926,113.150507902377,114.148006557827,115.145505213278,116.143003868728,
117.140502524179,118.138001179629,119.13549983508,120.13299849053,121.130497145981,
122.127995801431,123.125494456882,124.122993112332,125.120491767783,126.117990423233,
127.115489078684,128.112987734134,129.110486389585,130.107985045035,131.105483700486,
132.102982355936,133.100481011387),.UNSPECIFIED.);
#254=B_SPLINE_SURFACE_WITH_KNOTS('',3,3,((#41457,#41458,#41459,#41460,#41461,
#41462,#41463,#41464,#41465,#41466,#41467,#41468,#41469,#41470,#41471,#41472,
#41473,#41474,#41475,#41476,#41477,#41478,#41479,#41480,#41481,#41482,#41483,
#41484,#41485,#41486,#41487,#41488,#41489,#41490,#41491,#41492,#41493,#41494,
#41495,#41496,#41497,#41498,#41499,#41500,#41501,#41502,#41503,#41504,#41505,
#41506,#41507,#41508,#41509,#41510,#41511,#41512,#41513,#41514,#41515,#41516,
#41517,#41518,#41519,#41520,#41521,#41522,#41523,#41524,#41525,#41526,#41527,
#41528,#41529,#41530,#41531,#41532,#41533,#41534,#41535,#41536,#41537,#41538,
#41539,#41540,#41541,#41542,#41543,#41544,#41545,#41546,#41547,#41548,#41549,
#41550,#41551,#41552,#41553,#41554,#41555,#41556,#41557,#41558,#41559,#41560,
#41561,#41562,#41563,#41564,#41565,#41566,#41567,#41568,#41569,#41570,#41571,
#41572,#41573,#41574,#41575,#41576,#41577,#41578),(#41579,#41580,#41581,
#41582,#41583,#41584,#41585,#41586,#41587,#41588,#41589,#41590,#41591,#41592,
#41593,#41594,#41595,#41596,#41597,#41598,#41599,#41600,#41601,#41602,#41603,
#41604,#41605,#41606,#41607,#41608,#41609,#41610,#41611,#41612,#41613,#41614,
#41615,#41616,#41617,#41618,#41619,#41620,#41621,#41622,#41623,#41624,#41625,
#41626,#41627,#41628,#41629,#41630,#41631,#41632,#41633,#41634,#41635,#41636,
#41637,#41638,#41639,#41640,#41641,#41642,#41643,#41644,#41645,#41646,#41647,
#41648,#41649,#41650,#41651,#41652,#41653,#41654,#41655,#41656,#41657,#41658,
#41659,#41660,#41661,#41662,#41663,#41664,#41665,#41666,#41667,#41668,#41669,
#41670,#41671,#41672,#41673,#41674,#41675,#41676,#41677,#41678,#41679,#41680,
#41681,#41682,#41683,#41684,#41685,#41686,#41687,#41688,#41689,#41690,#41691,
#41692,#41693,#41694,#41695,#41696,#41697,#41698,#41699,#41700),(#41701,
#41702,#41703,#41704,#41705,#41706,#41707,#41708,#41709,#41710,#41711,#41712,
#41713,#41714,#41715,#41716,#41717,#41718,#41719,#41720,#41721,#41722,#41723,
#41724,#41725,#41726,#41727,#41728,#41729,#41730,#41731,#41732,#41733,#41734,
#41735,#41736,#41737,#41738,#41739,#41740,#41741,#41742,#41743,#41744,#41745,
#41746,#41747,#41748,#41749,#41750,#41751,#41752,#41753,#41754,#41755,#41756,
#41757,#41758,#41759,#41760,#41761,#41762,#41763,#41764,#41765,#41766,#41767,
#41768,#41769,#41770,#41771,#41772,#41773,#41774,#41775,#41776,#41777,#41778,
#41779,#41780,#41781,#41782,#41783,#41784,#41785,#41786,#41787,#41788,#41789,
#41790,#41791,#41792,#41793,#41794,#41795,#41796,#41797,#41798,#41799,#41800,
#41801,#41802,#41803,#41804,#41805,#41806,#41807,#41808,#41809,#41810,#41811,
#41812,#41813,#41814,#41815,#41816,#41817,#41818,#41819,#41820,#41821,#41822),
(#41823,#41824,#41825,#41826,#41827,#41828,#41829,#41830,#41831,#41832,
#41833,#41834,#41835,#41836,#41837,#41838,#41839,#41840,#41841,#41842,#41843,
#41844,#41845,#41846,#41847,#41848,#41849,#41850,#41851,#41852,#41853,#41854,
#41855,#41856,#41857,#41858,#41859,#41860,#41861,#41862,#41863,#41864,#41865,
#41866,#41867,#41868,#41869,#41870,#41871,#41872,#41873,#41874,#41875,#41876,
#41877,#41878,#41879,#41880,#41881,#41882,#41883,#41884,#41885,#41886,#41887,
#41888,#41889,#41890,#41891,#41892,#41893,#41894,#41895,#41896,#41897,#41898,
#41899,#41900,#41901,#41902,#41903,#41904,#41905,#41906,#41907,#41908,#41909,
#41910,#41911,#41912,#41913,#41914,#41915,#41916,#41917,#41918,#41919,#41920,
#41921,#41922,#41923,#41924,#41925,#41926,#41927,#41928,#41929,#41930,#41931,
#41932,#41933,#41934,#41935,#41936,#41937,#41938,#41939,#41940,#41941,#41942,
#41943,#41944)),.UNSPECIFIED.,.F.,.F.,.F.,(4,4),(4,1,1,1,1,1,1,1,1,1,1,
1,1,1,1,1,1,1,1,1,1,1,1,1,1,1,1,1,1,1,1,1,1,1,1,1,1,1,1,1,1,1,1,1,1,1,1,
1,1,1,1,1,1,1,1,1,1,1,1,1,1,1,1,1,1,1,1,1,1,1,1,1,1,1,1,1,1,1,1,1,1,1,1,
1,1,1,1,1,1,1,1,1,1,1,1,1,1,1,1,1,1,1,1,1,1,1,1,1,1,1,1,1,1,1,1,1,1,1,1,
4),(0.,0.0448889834294937),(11.8615800042567,12.8590786597072,13.8565773151577,
14.8540759706082,15.8515746260587,16.8490732815092,17.8465719369597,18.8440705924102,
19.8415692478607,20.8390679033112,21.8365665587617,22.8340652142122,23.8315638696627,
24.8290625251132,25.8265611805637,26.8240598360142,27.8215584914647,28.8190571469152,
29.8165558023657,30.8140544578162,31.8115531132667,32.8090517687172,33.8065504241677,
34.8040490796182,35.8015477350687,36.7990463905192,37.7965450459697,38.7940437014202,
39.7915423568707,40.7890410123212,41.7865396677717,42.7840383232222,43.7815369786727,
44.7790356341232,45.7765342895737,46.7740329450242,47.7715316004747,48.7690302559252,
49.7665289113757,50.7640275668262,51.7615262222767,52.7590248777272,53.7565235331777,
54.7540221886282,55.7515208440787,56.7490194995292,57.7465181549797,58.7440168104302,
59.7415154658807,60.7390141213312,61.7365127767817,62.7340114322322,63.7315100876827,
64.7290087431332,65.7265073985837,66.7240060540342,67.7215047094847,68.7190033649352,
69.7165020203857,70.7140006758362,71.7114993312867,72.7089979867372,73.7064966421877,
74.7039952976382,75.7014939530887,76.6989926085392,77.6964912639897,78.6939899194402,
79.6914885748908,80.6889872303413,81.6864858857918,82.6839845412423,83.6814831966928,
84.6789818521433,85.6764805075938,86.6739791630443,87.6714778184948,88.6689764739453,
89.6664751293958,90.6639737848463,91.6614724402968,92.6589710957473,93.6564697511978,
94.6539684066483,95.6514670620988,96.6489657175493,97.6464643729998,98.6439630284503,
99.6414616839008,100.638960339351,101.636458994802,102.633957650252,103.631456305703,
104.628954961153,105.626453616604,106.623952272054,107.621450927505,108.618949582955,
109.616448238406,110.613946893856,111.611445549307,112.608944204757,113.606442860208,
114.603941515658,115.601440171109,116.598938826559,117.59643748201,118.59393613746,
119.591434792911,120.588933448361,121.586432103812,122.583930759262,123.581429414713,
124.578928070163,125.576426725614,126.573925381064,127.571424036515,128.568922691965,
129.566421347416,130.563920002866),.UNSPECIFIED.);
#255=B_SPLINE_SURFACE_WITH_KNOTS('',3,3,((#42052,#42053,#42054,#42055,#42056,
#42057,#42058,#42059,#42060,#42061,#42062,#42063,#42064,#42065,#42066,#42067,
#42068,#42069,#42070,#42071,#42072,#42073,#42074,#42075,#42076,#42077,#42078,
#42079,#42080,#42081,#42082,#42083,#42084,#42085,#42086,#42087,#42088,#42089,
#42090,#42091,#42092,#42093,#42094,#42095,#42096,#42097,#42098,#42099,#42100,
#42101,#42102,#42103,#42104,#42105,#42106,#42107,#42108,#42109,#42110,#42111,
#42112,#42113,#42114,#42115,#42116,#42117,#42118,#42119,#42120,#42121,#42122,
#42123,#42124,#42125,#42126,#42127,#42128,#42129,#42130,#42131,#42132,#42133,
#42134,#42135,#42136,#42137,#42138,#42139,#42140,#42141,#42142,#42143,#42144,
#42145,#42146,#42147,#42148,#42149,#42150,#42151,#42152,#42153,#42154,#42155,
#42156,#42157,#42158,#42159,#42160,#42161,#42162,#42163,#42164,#42165,#42166,
#42167,#42168,#42169,#42170,#42171,#42172,#42173),(#42174,#42175,#42176,
#42177,#42178,#42179,#42180,#42181,#42182,#42183,#42184,#42185,#42186,#42187,
#42188,#42189,#42190,#42191,#42192,#42193,#42194,#42195,#42196,#42197,#42198,
#42199,#42200,#42201,#42202,#42203,#42204,#42205,#42206,#42207,#42208,#42209,
#42210,#42211,#42212,#42213,#42214,#42215,#42216,#42217,#42218,#42219,#42220,
#42221,#42222,#42223,#42224,#42225,#42226,#42227,#42228,#42229,#42230,#42231,
#42232,#42233,#42234,#42235,#42236,#42237,#42238,#42239,#42240,#42241,#42242,
#42243,#42244,#42245,#42246,#42247,#42248,#42249,#42250,#42251,#42252,#42253,
#42254,#42255,#42256,#42257,#42258,#42259,#42260,#42261,#42262,#42263,#42264,
#42265,#42266,#42267,#42268,#42269,#42270,#42271,#42272,#42273,#42274,#42275,
#42276,#42277,#42278,#42279,#42280,#42281,#42282,#42283,#42284,#42285,#42286,
#42287,#42288,#42289,#42290,#42291,#42292,#42293,#42294,#42295),(#42296,
#42297,#42298,#42299,#42300,#42301,#42302,#42303,#42304,#42305,#42306,#42307,
#42308,#42309,#42310,#42311,#42312,#42313,#42314,#42315,#42316,#42317,#42318,
#42319,#42320,#42321,#42322,#42323,#42324,#42325,#42326,#42327,#42328,#42329,
#42330,#42331,#42332,#42333,#42334,#42335,#42336,#42337,#42338,#42339,#42340,
#42341,#42342,#42343,#42344,#42345,#42346,#42347,#42348,#42349,#42350,#42351,
#42352,#42353,#42354,#42355,#42356,#42357,#42358,#42359,#42360,#42361,#42362,
#42363,#42364,#42365,#42366,#42367,#42368,#42369,#42370,#42371,#42372,#42373,
#42374,#42375,#42376,#42377,#42378,#42379,#42380,#42381,#42382,#42383,#42384,
#42385,#42386,#42387,#42388,#42389,#42390,#42391,#42392,#42393,#42394,#42395,
#42396,#42397,#42398,#42399,#42400,#42401,#42402,#42403,#42404,#42405,#42406,
#42407,#42408,#42409,#42410,#42411,#42412,#42413,#42414,#42415,#42416,#42417),
(#42418,#42419,#42420,#42421,#42422,#42423,#42424,#42425,#42426,#42427,
#42428,#42429,#42430,#42431,#42432,#42433,#42434,#42435,#42436,#42437,#42438,
#42439,#42440,#42441,#42442,#42443,#42444,#42445,#42446,#42447,#42448,#42449,
#42450,#42451,#42452,#42453,#42454,#42455,#42456,#42457,#42458,#42459,#42460,
#42461,#42462,#42463,#42464,#42465,#42466,#42467,#42468,#42469,#42470,#42471,
#42472,#42473,#42474,#42475,#42476,#42477,#42478,#42479,#42480,#42481,#42482,
#42483,#42484,#42485,#42486,#42487,#42488,#42489,#42490,#42491,#42492,#42493,
#42494,#42495,#42496,#42497,#42498,#42499,#42500,#42501,#42502,#42503,#42504,
#42505,#42506,#42507,#42508,#42509,#42510,#42511,#42512,#42513,#42514,#42515,
#42516,#42517,#42518,#42519,#42520,#42521,#42522,#42523,#42524,#42525,#42526,
#42527,#42528,#42529,#42530,#42531,#42532,#42533,#42534,#42535,#42536,#42537,
#42538,#42539)),.UNSPECIFIED.,.F.,.F.,.F.,(4,4),(4,1,1,1,1,1,1,1,1,1,1,
1,1,1,1,1,1,1,1,1,1,1,1,1,1,1,1,1,1,1,1,1,1,1,1,1,1,1,1,1,1,1,1,1,1,1,1,
1,1,1,1,1,1,1,1,1,1,1,1,1,1,1,1,1,1,1,1,1,1,1,1,1,1,1,1,1,1,1,1,1,1,1,1,
1,1,1,1,1,1,1,1,1,1,1,1,1,1,1,1,1,1,1,1,1,1,1,1,1,1,1,1,1,1,1,1,1,1,1,1,
4),(0.,0.0448889834294937),(14.3981410127769,15.3956396682274,16.3931383236779,
17.3906369791284,18.3881356345789,19.3856342900294,20.3831329454799,21.3806316009304,
22.3781302563809,23.3756289118314,24.3731275672819,25.3706262227324,26.3681248781829,
27.3656235336334,28.3631221890839,29.3606208445344,30.3581194999849,31.3556181554354,
32.3531168108859,33.3506154663364,34.3481141217869,35.3456127772374,36.3431114326879,
37.3406100881384,38.3381087435889,39.3356073990394,40.3331060544899,41.3306047099404,
42.3281033653909,43.3256020208414,44.3231006762919,45.3205993317424,46.3180979871929,
47.3155966426434,48.3130952980939,49.3105939535444,50.3080926089949,51.3055912644454,
52.3030899198959,53.3005885753464,54.2980872307969,55.2955858862474,56.2930845416979,
57.2905831971484,58.2880818525989,59.2855805080494,60.2830791634999,61.2805778189504,
62.2780764744009,63.2755751298514,64.2730737853019,65.2705724407524,66.2680710962029,
67.2655697516534,68.2630684071039,69.2605670625544,70.2580657180049,71.2555643734554,
72.2530630289059,73.2505616843565,74.248060339807,75.2455589952575,76.243057650708,
77.2405563061585,78.238054961609,79.2355536170595,80.23305227251,81.2305509279605,
82.228049583411,83.2255482388615,84.223046894312,85.2205455497625,86.218044205213,
87.2155428606635,88.213041516114,89.2105401715645,90.208038827015,91.2055374824655,
92.203036137916,93.2005347933665,94.198033448817,95.1955321042675,96.193030759718,
97.1905294151685,98.188028070619,99.1855267260695,100.18302538152,101.18052403697,
102.178022692421,103.175521347871,104.173020003322,105.170518658772,106.168017314223,
107.165515969673,108.163014625124,109.160513280574,110.158011936025,111.155510591476,
112.153009246926,113.150507902377,114.148006557827,115.145505213278,116.143003868728,
117.140502524179,118.138001179629,119.13549983508,120.13299849053,121.130497145981,
122.127995801431,123.125494456882,124.122993112332,125.120491767783,126.117990423233,
127.115489078684,128.112987734134,129.110486389585,130.107985045035,131.105483700486,
132.102982355936,133.100481011387),.UNSPECIFIED.);
#256=B_SPLINE_SURFACE_WITH_KNOTS('',3,3,((#42712,#42713,#42714,#42715,#42716,
#42717,#42718,#42719,#42720,#42721,#42722,#42723,#42724,#42725,#42726,#42727,
#42728,#42729,#42730,#42731,#42732,#42733,#42734,#42735,#42736,#42737,#42738,
#42739,#42740,#42741,#42742,#42743,#42744,#42745,#42746,#42747,#42748,#42749,
#42750,#42751,#42752,#42753,#42754,#42755,#42756,#42757,#42758,#42759,#42760,
#42761,#42762,#42763,#42764,#42765,#42766,#42767,#42768,#42769,#42770,#42771,
#42772,#42773,#42774,#42775,#42776,#42777,#42778,#42779,#42780,#42781,#42782,
#42783,#42784,#42785,#42786,#42787,#42788,#42789,#42790,#42791,#42792,#42793,
#42794,#42795,#42796,#42797,#42798,#42799,#42800,#42801,#42802,#42803,#42804,
#42805,#42806),(#42807,#42808,#42809,#42810,#42811,#42812,#42813,#42814,
#42815,#42816,#42817,#42818,#42819,#42820,#42821,#42822,#42823,#42824,#42825,
#42826,#42827,#42828,#42829,#42830,#42831,#42832,#42833,#42834,#42835,#42836,
#42837,#42838,#42839,#42840,#42841,#42842,#42843,#42844,#42845,#42846,#42847,
#42848,#42849,#42850,#42851,#42852,#42853,#42854,#42855,#42856,#42857,#42858,
#42859,#42860,#42861,#42862,#42863,#42864,#42865,#42866,#42867,#42868,#42869,
#42870,#42871,#42872,#42873,#42874,#42875,#42876,#42877,#42878,#42879,#42880,
#42881,#42882,#42883,#42884,#42885,#42886,#42887,#42888,#42889,#42890,#42891,
#42892,#42893,#42894,#42895,#42896,#42897,#42898,#42899,#42900,#42901),
(#42902,#42903,#42904,#42905,#42906,#42907,#42908,#42909,#42910,#42911,
#42912,#42913,#42914,#42915,#42916,#42917,#42918,#42919,#42920,#42921,#42922,
#42923,#42924,#42925,#42926,#42927,#42928,#42929,#42930,#42931,#42932,#42933,
#42934,#42935,#42936,#42937,#42938,#42939,#42940,#42941,#42942,#42943,#42944,
#42945,#42946,#42947,#42948,#42949,#42950,#42951,#42952,#42953,#42954,#42955,
#42956,#42957,#42958,#42959,#42960,#42961,#42962,#42963,#42964,#42965,#42966,
#42967,#42968,#42969,#42970,#42971,#42972,#42973,#42974,#42975,#42976,#42977,
#42978,#42979,#42980,#42981,#42982,#42983,#42984,#42985,#42986,#42987,#42988,
#42989,#42990,#42991,#42992,#42993,#42994,#42995,#42996),(#42997,#42998,
#42999,#43000,#43001,#43002,#43003,#43004,#43005,#43006,#43007,#43008,#43009,
#43010,#43011,#43012,#43013,#43014,#43015,#43016,#43017,#43018,#43019,#43020,
#43021,#43022,#43023,#43024,#43025,#43026,#43027,#43028,#43029,#43030,#43031,
#43032,#43033,#43034,#43035,#43036,#43037,#43038,#43039,#43040,#43041,#43042,
#43043,#43044,#43045,#43046,#43047,#43048,#43049,#43050,#43051,#43052,#43053,
#43054,#43055,#43056,#43057,#43058,#43059,#43060,#43061,#43062,#43063,#43064,
#43065,#43066,#43067,#43068,#43069,#43070,#43071,#43072,#43073,#43074,#43075,
#43076,#43077,#43078,#43079,#43080,#43081,#43082,#43083,#43084,#43085,#43086,
#43087,#43088,#43089,#43090,#43091)),.UNSPECIFIED.,.F.,.F.,.F.,(4,4),(4,
1,1,1,1,1,1,1,1,1,1,1,1,1,1,1,1,1,1,1,1,1,1,1,1,1,1,1,1,1,1,1,1,1,1,1,1,
1,1,1,1,1,1,1,1,1,1,1,1,1,1,1,1,1,1,1,1,1,1,1,1,1,1,1,1,1,1,1,1,1,1,1,1,
1,1,1,1,1,1,1,1,1,1,1,1,1,1,1,1,1,1,1,4),(0.,0.112756507572734),(11.8517336648509,
12.3420477881087,12.8323619113665,13.3226760346243,13.812990157882,14.3033042811398,
14.7936184043976,15.2839325276554,15.7742466509132,16.264560774171,16.7548748974288,
17.2451890206866,17.7355031439444,18.2258172672022,18.71613139046,19.2064455137178,
19.6967596369755,20.1870737602333,20.6773878834911,21.1677020067489,21.6580161300067,
22.1483302532645,22.6386443765223,23.1289584997801,23.6192726230379,24.1095867462957,
24.5999008695535,25.0902149928113,25.5805291160691,26.0708432393268,26.5611573625846,
27.0514714858424,27.5417856091002,28.032099732358,28.5224138556158,29.0127279788736,
29.5030421021314,29.9933562253892,30.483670348647,30.9739844719048,31.4642985951626,
31.9546127184203,32.4449268416781,32.9352409649359,33.4255550881937,33.9158692114515,
34.4061833347093,34.8964974579671,35.3868115812249,35.8771257044827,36.3674398277405,
36.8577539509983,37.3480680742561,37.8383821975139,38.3286963207716,38.8190104440294,
39.3093245672872,39.799638690545,40.2899528138028,40.7802669370606,41.2705810603184,
41.7608951835762,42.251209306834,42.7415234300918,43.2318375533496,43.7221516766074,
44.2124657998651,44.7027799231229,45.1930940463807,45.6834081696385,46.1737222928963,
46.6640364161541,47.1543505394119,47.6446646626697,48.1349787859275,48.6252929091853,
49.1156070324431,49.6059211557009,50.0962352789586,50.5865494022164,51.0768635254742,
51.567177648732,52.0574917719898,52.5478058952476,53.0381200185054,53.5284341417632,
54.018748265021,54.5090623882788,54.9993765115366,55.4896906347944,55.9800047580521,
56.4703188813099,56.9606330045677),.UNSPECIFIED.);
#257=B_SPLINE_SURFACE_WITH_KNOTS('',3,3,((#43365,#43366,#43367,#43368,#43369,
#43370,#43371,#43372,#43373,#43374,#43375,#43376,#43377,#43378,#43379,#43380,
#43381,#43382,#43383,#43384,#43385,#43386,#43387,#43388,#43389,#43390,#43391,
#43392,#43393,#43394,#43395,#43396,#43397,#43398,#43399,#43400,#43401,#43402,
#43403,#43404,#43405,#43406,#43407,#43408,#43409,#43410,#43411,#43412,#43413,
#43414,#43415,#43416,#43417,#43418,#43419,#43420,#43421,#43422,#43423,#43424,
#43425,#43426,#43427,#43428,#43429,#43430,#43431,#43432,#43433,#43434,#43435,
#43436,#43437,#43438,#43439,#43440,#43441,#43442,#43443,#43444,#43445,#43446,
#43447,#43448,#43449,#43450,#43451,#43452,#43453,#43454,#43455,#43456,#43457,
#43458,#43459),(#43460,#43461,#43462,#43463,#43464,#43465,#43466,#43467,
#43468,#43469,#43470,#43471,#43472,#43473,#43474,#43475,#43476,#43477,#43478,
#43479,#43480,#43481,#43482,#43483,#43484,#43485,#43486,#43487,#43488,#43489,
#43490,#43491,#43492,#43493,#43494,#43495,#43496,#43497,#43498,#43499,#43500,
#43501,#43502,#43503,#43504,#43505,#43506,#43507,#43508,#43509,#43510,#43511,
#43512,#43513,#43514,#43515,#43516,#43517,#43518,#43519,#43520,#43521,#43522,
#43523,#43524,#43525,#43526,#43527,#43528,#43529,#43530,#43531,#43532,#43533,
#43534,#43535,#43536,#43537,#43538,#43539,#43540,#43541,#43542,#43543,#43544,
#43545,#43546,#43547,#43548,#43549,#43550,#43551,#43552,#43553,#43554),
(#43555,#43556,#43557,#43558,#43559,#43560,#43561,#43562,#43563,#43564,
#43565,#43566,#43567,#43568,#43569,#43570,#43571,#43572,#43573,#43574,#43575,
#43576,#43577,#43578,#43579,#43580,#43581,#43582,#43583,#43584,#43585,#43586,
#43587,#43588,#43589,#43590,#43591,#43592,#43593,#43594,#43595,#43596,#43597,
#43598,#43599,#43600,#43601,#43602,#43603,#43604,#43605,#43606,#43607,#43608,
#43609,#43610,#43611,#43612,#43613,#43614,#43615,#43616,#43617,#43618,#43619,
#43620,#43621,#43622,#43623,#43624,#43625,#43626,#43627,#43628,#43629,#43630,
#43631,#43632,#43633,#43634,#43635,#43636,#43637,#43638,#43639,#43640,#43641,
#43642,#43643,#43644,#43645,#43646,#43647,#43648,#43649),(#43650,#43651,
#43652,#43653,#43654,#43655,#43656,#43657,#43658,#43659,#43660,#43661,#43662,
#43663,#43664,#43665,#43666,#43667,#43668,#43669,#43670,#43671,#43672,#43673,
#43674,#43675,#43676,#43677,#43678,#43679,#43680,#43681,#43682,#43683,#43684,
#43685,#43686,#43687,#43688,#43689,#43690,#43691,#43692,#43693,#43694,#43695,
#43696,#43697,#43698,#43699,#43700,#43701,#43702,#43703,#43704,#43705,#43706,
#43707,#43708,#43709,#43710,#43711,#43712,#43713,#43714,#43715,#43716,#43717,
#43718,#43719,#43720,#43721,#43722,#43723,#43724,#43725,#43726,#43727,#43728,
#43729,#43730,#43731,#43732,#43733,#43734,#43735,#43736,#43737,#43738,#43739,
#43740,#43741,#43742,#43743,#43744)),.UNSPECIFIED.,.F.,.F.,.F.,(4,4),(4,
1,1,1,1,1,1,1,1,1,1,1,1,1,1,1,1,1,1,1,1,1,1,1,1,1,1,1,1,1,1,1,1,1,1,1,1,
1,1,1,1,1,1,1,1,1,1,1,1,1,1,1,1,1,1,1,1,1,1,1,1,1,1,1,1,1,1,1,1,1,1,1,1,
1,1,1,1,1,1,1,1,1,1,1,1,1,1,1,1,1,1,1,4),(0.,0.112756507572734),(14.3984001269719,
14.8887142502297,15.3790283734874,15.8693424967452,16.359656620003,16.8499707432608,
17.3402848665186,17.8305989897764,18.3209131130342,18.811227236292,19.3015413595498,
19.7918554828076,20.2821696060654,20.7724837293232,21.2627978525809,21.7531119758387,
22.2434260990965,22.7337402223543,23.2240543456121,23.7143684688699,24.2046825921277,
24.6949967153855,25.1853108386433,25.6756249619011,26.1659390851589,26.6562532084167,
27.1465673316744,27.6368814549322,28.12719557819,28.6175097014478,29.1078238247056,
29.5981379479634,30.0884520712212,30.578766194479,31.0690803177368,31.5593944409946,
32.0497085642524,32.5400226875101,33.0303368107679,33.5206509340257,34.0109650572835,
34.5012791805413,34.9915933037991,35.4819074270569,35.9722215503147,36.4625356735725,
36.9528497968303,37.4431639200881,37.9334780433459,38.4237921666036,38.9141062898614,
39.4044204131192,39.894734536377,40.3850486596348,40.8753627828926,41.3656769061504,
41.8559910294082,42.346305152666,42.8366192759238,43.3269333991816,43.8172475224394,
44.3075616456971,44.7978757689549,45.2881898922127,45.7785040154705,46.2688181387283,
46.7591322619861,47.2494463852439,47.7397605085017,48.2300746317595,48.7203887550173,
49.2107028782751,49.7010170015329,50.1913311247907,50.6816452480484,51.1719593713062,
51.662273494564,52.1525876178218,52.6429017410796,53.1332158643374,53.6235299875952,
54.113844110853,54.6041582341108,55.0944723573686,55.5847864806264,56.0751006038842,
56.5654147271419,57.0557288503997,57.5460429736575,58.0363570969153,58.5266712201731,
59.0169853434309,59.5072994666887),.UNSPECIFIED.);
#258=B_SPLINE_SURFACE_WITH_KNOTS('',3,3,((#45452,#45453,#45454,#45455,#45456,
#45457,#45458,#45459,#45460,#45461,#45462,#45463,#45464,#45465,#45466,#45467,
#45468,#45469,#45470,#45471,#45472,#45473,#45474,#45475,#45476,#45477,#45478,
#45479,#45480,#45481,#45482,#45483,#45484,#45485,#45486,#45487,#45488,#45489,
#45490,#45491,#45492,#45493,#45494,#45495,#45496,#45497,#45498,#45499,#45500,
#45501,#45502,#45503,#45504,#45505,#45506,#45507,#45508,#45509,#45510,#45511,
#45512,#45513,#45514,#45515,#45516,#45517,#45518,#45519,#45520,#45521,#45522,
#45523,#45524,#45525,#45526,#45527,#45528,#45529,#45530,#45531,#45532,#45533,
#45534,#45535,#45536,#45537,#45538,#45539,#45540,#45541,#45542,#45543,#45544,
#45545,#45546,#45547,#45548,#45549,#45550,#45551,#45552,#45553,#45554,#45555,
#45556,#45557,#45558,#45559,#45560,#45561,#45562,#45563,#45564,#45565,#45566,
#45567,#45568,#45569),(#45570,#45571,#45572,#45573,#45574,#45575,#45576,
#45577,#45578,#45579,#45580,#45581,#45582,#45583,#45584,#45585,#45586,#45587,
#45588,#45589,#45590,#45591,#45592,#45593,#45594,#45595,#45596,#45597,#45598,
#45599,#45600,#45601,#45602,#45603,#45604,#45605,#45606,#45607,#45608,#45609,
#45610,#45611,#45612,#45613,#45614,#45615,#45616,#45617,#45618,#45619,#45620,
#45621,#45622,#45623,#45624,#45625,#45626,#45627,#45628,#45629,#45630,#45631,
#45632,#45633,#45634,#45635,#45636,#45637,#45638,#45639,#45640,#45641,#45642,
#45643,#45644,#45645,#45646,#45647,#45648,#45649,#45650,#45651,#45652,#45653,
#45654,#45655,#45656,#45657,#45658,#45659,#45660,#45661,#45662,#45663,#45664,
#45665,#45666,#45667,#45668,#45669,#45670,#45671,#45672,#45673,#45674,#45675,
#45676,#45677,#45678,#45679,#45680,#45681,#45682,#45683,#45684,#45685,#45686,
#45687),(#45688,#45689,#45690,#45691,#45692,#45693,#45694,#45695,#45696,
#45697,#45698,#45699,#45700,#45701,#45702,#45703,#45704,#45705,#45706,#45707,
#45708,#45709,#45710,#45711,#45712,#45713,#45714,#45715,#45716,#45717,#45718,
#45719,#45720,#45721,#45722,#45723,#45724,#45725,#45726,#45727,#45728,#45729,
#45730,#45731,#45732,#45733,#45734,#45735,#45736,#45737,#45738,#45739,#45740,
#45741,#45742,#45743,#45744,#45745,#45746,#45747,#45748,#45749,#45750,#45751,
#45752,#45753,#45754,#45755,#45756,#45757,#45758,#45759,#45760,#45761,#45762,
#45763,#45764,#45765,#45766,#45767,#45768,#45769,#45770,#45771,#45772,#45773,
#45774,#45775,#45776,#45777,#45778,#45779,#45780,#45781,#45782,#45783,#45784,
#45785,#45786,#45787,#45788,#45789,#45790,#45791,#45792,#45793,#45794,#45795,
#45796,#45797,#45798,#45799,#45800,#45801,#45802,#45803,#45804,#45805),
(#45806,#45807,#45808,#45809,#45810,#45811,#45812,#45813,#45814,#45815,
#45816,#45817,#45818,#45819,#45820,#45821,#45822,#45823,#45824,#45825,#45826,
#45827,#45828,#45829,#45830,#45831,#45832,#45833,#45834,#45835,#45836,#45837,
#45838,#45839,#45840,#45841,#45842,#45843,#45844,#45845,#45846,#45847,#45848,
#45849,#45850,#45851,#45852,#45853,#45854,#45855,#45856,#45857,#45858,#45859,
#45860,#45861,#45862,#45863,#45864,#45865,#45866,#45867,#45868,#45869,#45870,
#45871,#45872,#45873,#45874,#45875,#45876,#45877,#45878,#45879,#45880,#45881,
#45882,#45883,#45884,#45885,#45886,#45887,#45888,#45889,#45890,#45891,#45892,
#45893,#45894,#45895,#45896,#45897,#45898,#45899,#45900,#45901,#45902,#45903,
#45904,#45905,#45906,#45907,#45908,#45909,#45910,#45911,#45912,#45913,#45914,
#45915,#45916,#45917,#45918,#45919,#45920,#45921,#45922,#45923)),
 .UNSPECIFIED.,.F.,.F.,.F.,(4,4),(4,1,1,1,1,1,1,1,1,1,1,1,1,1,1,1,1,1,1,
1,1,1,1,1,1,1,1,1,1,1,1,1,1,1,1,1,1,1,1,1,1,1,1,1,1,1,1,1,1,1,1,1,1,1,1,
1,1,1,1,1,1,1,1,1,1,1,1,1,1,1,1,1,1,1,1,1,1,1,1,1,1,1,1,1,1,1,1,1,1,1,1,
1,1,1,1,1,1,1,1,1,1,1,1,1,1,1,1,1,1,1,1,1,1,1,1,4),(0.,0.0642013499338863),
(12.6240367263184,13.6183778789988,14.6127190316793,15.6070601843597,16.6014013370402,
17.5957424897206,18.590083642401,19.5844247950815,20.5787659477619,21.5731071004423,
22.5674482531228,23.5617894058032,24.5561305584837,25.5504717111641,26.5448128638445,
27.539154016525,28.5334951692054,29.5278363218858,30.5221774745663,31.5165186272467,
32.5108597799272,33.5052009326076,34.499542085288,35.4938832379685,36.4882243906489,
37.4825655433293,38.4769066960098,39.4712478486902,40.4655890013707,41.4599301540511,
42.4542713067315,43.448612459412,44.4429536120924,45.4372947647728,46.4316359174533,
47.4259770701337,48.4203182228142,49.4146593754946,50.409000528175,51.4033416808555,
52.3976828335359,53.3920239862163,54.3863651388968,55.3807062915772,56.3750474442577,
57.3693885969381,58.3637297496185,59.358070902299,60.3524120549794,61.3467532076598,
62.3410943603403,63.3354355130207,64.3297766657012,65.3241178183816,66.318458971062,
67.3128001237425,68.3071412764229,69.3014824291033,70.2958235817838,71.2901647344642,
72.2845058871447,73.2788470398251,74.2731881925055,75.267529345186,76.2618704978664,
77.2562116505468,78.2505528032273,79.2448939559077,80.2392351085882,81.2335762612686,
82.227917413949,83.2222585666295,84.2165997193099,85.2109408719903,86.2052820246708,
87.1996231773512,88.1939643300317,89.1883054827121,90.1826466353925,91.176987788073,
92.1713289407534,93.1656700934338,94.1600112461143,95.1543523987947,96.1486935514752,
97.1430347041556,98.137375856836,99.1317170095165,100.126058162197,101.120399314877,
102.114740467558,103.109081620238,104.103422772919,105.097763925599,106.09210507828,
107.08644623096,108.08078738364,109.075128536321,110.069469689001,111.063810841682,
112.058151994362,113.052493147043,114.046834299723,115.041175452403,116.035516605084,
117.029857757764,118.024198910445,119.018540063125,120.012881215806,121.007222368486,
122.001563521167,122.995904673847,123.990245826527,124.984586979208,125.978928131888,
126.973269284569),.UNSPECIFIED.);
#259=B_SPLINE_SURFACE_WITH_KNOTS('',3,3,((#46071,#46072,#46073,#46074,#46075,
#46076,#46077,#46078,#46079,#46080,#46081,#46082,#46083,#46084,#46085,#46086,
#46087,#46088,#46089,#46090,#46091,#46092,#46093,#46094,#46095,#46096,#46097,
#46098,#46099,#46100,#46101,#46102,#46103,#46104,#46105,#46106,#46107,#46108,
#46109,#46110,#46111,#46112,#46113,#46114,#46115,#46116,#46117,#46118,#46119,
#46120,#46121,#46122,#46123,#46124,#46125,#46126,#46127,#46128,#46129,#46130,
#46131,#46132,#46133,#46134,#46135,#46136,#46137,#46138,#46139,#46140,#46141,
#46142,#46143,#46144,#46145,#46146,#46147,#46148,#46149,#46150,#46151,#46152,
#46153,#46154,#46155,#46156,#46157,#46158,#46159,#46160,#46161,#46162,#46163,
#46164,#46165,#46166,#46167,#46168,#46169,#46170,#46171,#46172,#46173,#46174,
#46175,#46176,#46177,#46178,#46179,#46180,#46181,#46182,#46183,#46184,#46185,
#46186,#46187,#46188),(#46189,#46190,#46191,#46192,#46193,#46194,#46195,
#46196,#46197,#46198,#46199,#46200,#46201,#46202,#46203,#46204,#46205,#46206,
#46207,#46208,#46209,#46210,#46211,#46212,#46213,#46214,#46215,#46216,#46217,
#46218,#46219,#46220,#46221,#46222,#46223,#46224,#46225,#46226,#46227,#46228,
#46229,#46230,#46231,#46232,#46233,#46234,#46235,#46236,#46237,#46238,#46239,
#46240,#46241,#46242,#46243,#46244,#46245,#46246,#46247,#46248,#46249,#46250,
#46251,#46252,#46253,#46254,#46255,#46256,#46257,#46258,#46259,#46260,#46261,
#46262,#46263,#46264,#46265,#46266,#46267,#46268,#46269,#46270,#46271,#46272,
#46273,#46274,#46275,#46276,#46277,#46278,#46279,#46280,#46281,#46282,#46283,
#46284,#46285,#46286,#46287,#46288,#46289,#46290,#46291,#46292,#46293,#46294,
#46295,#46296,#46297,#46298,#46299,#46300,#46301,#46302,#46303,#46304,#46305,
#46306),(#46307,#46308,#46309,#46310,#46311,#46312,#46313,#46314,#46315,
#46316,#46317,#46318,#46319,#46320,#46321,#46322,#46323,#46324,#46325,#46326,
#46327,#46328,#46329,#46330,#46331,#46332,#46333,#46334,#46335,#46336,#46337,
#46338,#46339,#46340,#46341,#46342,#46343,#46344,#46345,#46346,#46347,#46348,
#46349,#46350,#46351,#46352,#46353,#46354,#46355,#46356,#46357,#46358,#46359,
#46360,#46361,#46362,#46363,#46364,#46365,#46366,#46367,#46368,#46369,#46370,
#46371,#46372,#46373,#46374,#46375,#46376,#46377,#46378,#46379,#46380,#46381,
#46382,#46383,#46384,#46385,#46386,#46387,#46388,#46389,#46390,#46391,#46392,
#46393,#46394,#46395,#46396,#46397,#46398,#46399,#46400,#46401,#46402,#46403,
#46404,#46405,#46406,#46407,#46408,#46409,#46410,#46411,#46412,#46413,#46414,
#46415,#46416,#46417,#46418,#46419,#46420,#46421,#46422,#46423,#46424),
(#46425,#46426,#46427,#46428,#46429,#46430,#46431,#46432,#46433,#46434,
#46435,#46436,#46437,#46438,#46439,#46440,#46441,#46442,#46443,#46444,#46445,
#46446,#46447,#46448,#46449,#46450,#46451,#46452,#46453,#46454,#46455,#46456,
#46457,#46458,#46459,#46460,#46461,#46462,#46463,#46464,#46465,#46466,#46467,
#46468,#46469,#46470,#46471,#46472,#46473,#46474,#46475,#46476,#46477,#46478,
#46479,#46480,#46481,#46482,#46483,#46484,#46485,#46486,#46487,#46488,#46489,
#46490,#46491,#46492,#46493,#46494,#46495,#46496,#46497,#46498,#46499,#46500,
#46501,#46502,#46503,#46504,#46505,#46506,#46507,#46508,#46509,#46510,#46511,
#46512,#46513,#46514,#46515,#46516,#46517,#46518,#46519,#46520,#46521,#46522,
#46523,#46524,#46525,#46526,#46527,#46528,#46529,#46530,#46531,#46532,#46533,
#46534,#46535,#46536,#46537,#46538,#46539,#46540,#46541,#46542)),
 .UNSPECIFIED.,.F.,.F.,.F.,(4,4),(4,1,1,1,1,1,1,1,1,1,1,1,1,1,1,1,1,1,1,
1,1,1,1,1,1,1,1,1,1,1,1,1,1,1,1,1,1,1,1,1,1,1,1,1,1,1,1,1,1,1,1,1,1,1,1,
1,1,1,1,1,1,1,1,1,1,1,1,1,1,1,1,1,1,1,1,1,1,1,1,1,1,1,1,1,1,1,1,1,1,1,1,
1,1,1,1,1,1,1,1,1,1,1,1,1,1,1,1,1,1,1,1,1,1,1,1,4),(0.,0.0642013499338863),
(15.4901713080479,16.481671388406,17.4731714687642,18.4646715491223,19.4561716294804,
20.4476717098386,21.4391717901967,22.4306718705548,23.4221719509129,24.4136720312711,
25.4051721116292,26.3966721919873,27.3881722723455,28.3796723527036,29.3711724330617,
30.3626725134198,31.354172593778,32.3456726741361,33.3371727544942,34.3286728348524,
35.3201729152105,36.3116729955686,37.3031730759268,38.2946731562849,39.286173236643,
40.2776733170011,41.2691733973593,42.2606734777174,43.2521735580755,44.2436736384336,
45.2351737187918,46.2266737991499,47.218173879508,48.2096739598662,49.2011740402243,
50.1926741205824,51.1841742009405,52.1756742812987,53.1671743616568,54.1586744420149,
55.1501745223731,56.1416746027312,57.1331746830893,58.1246747634475,59.1161748438056,
60.1076749241637,61.0991750045218,62.09067508488,63.0821751652381,64.0736752455962,
65.0651753259544,66.0566754063125,67.0481754866706,68.0396755670287,69.0311756473869,
70.022675727745,71.0141758081031,72.0056758884613,72.9971759688194,73.9886760491775,
74.9801761295356,75.9716762098938,76.9631762902519,77.95467637061,78.9461764509682,
79.9376765313263,80.9291766116844,81.9206766920425,82.9121767724007,83.9036768527588,
84.8951769331169,85.8866770134751,86.8781770938332,87.8696771741913,88.8611772545494,
89.8526773349076,90.8441774152657,91.8356774956238,92.827177575982,93.8186776563401,
94.8101777366982,95.8016778170563,96.7931778974145,97.7846779777726,98.7761780581307,
99.7676781384889,100.759178218847,101.750678299205,102.742178379563,103.733678459921,
104.72517854028,105.716678620638,106.708178700996,107.699678781354,108.691178861712,
109.68267894207,110.674179022428,111.665679102786,112.657179183145,113.648679263503,
114.640179343861,115.631679424219,116.623179504577,117.614679584935,118.606179665293,
119.597679745651,120.58917982601,121.580679906368,122.572179986726,123.563680067084,
124.555180147442,125.5466802278,126.538180308158,127.529680388516,128.521180468875,
129.512680549233),.UNSPECIFIED.);
#260=B_SPLINE_SURFACE_WITH_KNOTS('',3,3,((#53360,#53361,#53362,#53363,#53364,
#53365,#53366,#53367,#53368,#53369,#53370,#53371,#53372,#53373,#53374,#53375,
#53376,#53377,#53378,#53379,#53380,#53381,#53382,#53383,#53384,#53385,#53386,
#53387,#53388,#53389,#53390,#53391,#53392,#53393,#53394,#53395,#53396,#53397,
#53398,#53399,#53400,#53401,#53402,#53403,#53404,#53405,#53406,#53407,#53408,
#53409,#53410,#53411,#53412,#53413,#53414,#53415,#53416,#53417,#53418,#53419,
#53420,#53421,#53422,#53423,#53424,#53425,#53426,#53427,#53428,#53429,#53430,
#53431,#53432,#53433,#53434,#53435,#53436,#53437,#53438,#53439,#53440,#53441,
#53442,#53443,#53444,#53445,#53446,#53447,#53448,#53449,#53450,#53451,#53452,
#53453,#53454,#53455,#53456,#53457,#53458,#53459,#53460,#53461,#53462,#53463,
#53464,#53465,#53466,#53467,#53468,#53469,#53470,#53471,#53472,#53473,#53474,
#53475,#53476,#53477,#53478,#53479,#53480,#53481,#53482,#53483,#53484,#53485,
#53486,#53487,#53488,#53489,#53490,#53491,#53492,#53493,#53494,#53495,#53496,
#53497,#53498,#53499,#53500,#53501,#53502,#53503,#53504,#53505,#53506,#53507,
#53508,#53509,#53510,#53511,#53512,#53513,#53514,#53515,#53516,#53517,#53518,
#53519,#53520,#53521,#53522,#53523,#53524,#53525,#53526,#53527,#53528,#53529,
#53530,#53531,#53532,#53533,#53534,#53535,#53536,#53537,#53538,#53539,#53540,
#53541,#53542,#53543,#53544,#53545,#53546,#53547,#53548,#53549,#53550,#53551,
#53552,#53553,#53554,#53555,#53556,#53557,#53558,#53559,#53560,#53561,#53562,
#53563,#53564,#53565,#53566,#53567,#53568,#53569,#53570,#53571,#53572,#53573,
#53574,#53575,#53576,#53577,#53578,#53579,#53580,#53581,#53582,#53583,#53584,
#53585,#53586,#53587,#53588,#53589,#53590,#53591,#53592,#53593,#53594,#53595,
#53596,#53597,#53598,#53599,#53600,#53601,#53602,#53603,#53604,#53605,#53606,
#53607,#53608,#53609,#53610,#53611,#53612,#53613,#53614,#53615,#53616,#53617,
#53618,#53619,#53620,#53621,#53622,#53623,#53624,#53625,#53626,#53627,#53628,
#53629,#53630,#53631,#53632,#53633,#53634,#53635,#53636,#53637,#53638,#53639,
#53640,#53641,#53642,#53643,#53644,#53645,#53646,#53647,#53648,#53649,#53650,
#53651,#53652,#53653,#53654,#53655,#53656,#53657,#53658,#53659,#53660,#53661,
#53662,#53663,#53664,#53665,#53666,#53667,#53668,#53669,#53670,#53671,#53672,
#53673,#53674,#53675,#53676,#53677,#53678,#53679,#53680,#53681,#53682,#53683,
#53684,#53685,#53686,#53687,#53688,#53689,#53690,#53691,#53692,#53693,#53694,
#53695,#53696,#53697,#53698,#53699,#53700,#53701,#53702,#53703,#53704,#53705,
#53706,#53707,#53708,#53709,#53710,#53711,#53712,#53713,#53714,#53715,#53716,
#53717,#53718,#53719,#53720,#53721,#53722,#53723,#53724,#53725,#53726,#53727,
#53728,#53729,#53730,#53731,#53732,#53733,#53734,#53735,#53736,#53737,#53738,
#53739,#53740,#53741,#53742,#53743,#53744,#53745,#53746,#53747,#53748,#53749,
#53750,#53751,#53752,#53753,#53754,#53755,#53756,#53757,#53758,#53759,#53760,
#53761,#53762,#53763,#53764,#53765,#53766,#53767,#53768,#53769,#53770,#53771,
#53772,#53773,#53774,#53775,#53776,#53777,#53778,#53779,#53780,#53781,#53782,
#53783,#53784,#53785,#53786,#53787,#53788,#53789,#53790,#53791,#53792,#53793,
#53794,#53795,#53796,#53797,#53798,#53799,#53800,#53801,#53802,#53803,#53804,
#53805,#53806,#53807,#53808,#53809,#53810,#53811,#53812,#53813,#53814,#53815,
#53816,#53817,#53818,#53819,#53820,#53821,#53822,#53823,#53824,#53825,#53826,
#53827,#53828,#53829,#53830,#53831,#53832,#53833,#53834,#53835,#53836,#53837,
#53838,#53839,#53840,#53841,#53842,#53843,#53844,#53845,#53846,#53847,#53848,
#53849,#53850,#53851,#53852,#53853,#53854,#53855,#53856,#53857,#53858,#53859,
#53860,#53861,#53862,#53863,#53864,#53865,#53866,#53867),(#53868,#53869,
#53870,#53871,#53872,#53873,#53874,#53875,#53876,#53877,#53878,#53879,#53880,
#53881,#53882,#53883,#53884,#53885,#53886,#53887,#53888,#53889,#53890,#53891,
#53892,#53893,#53894,#53895,#53896,#53897,#53898,#53899,#53900,#53901,#53902,
#53903,#53904,#53905,#53906,#53907,#53908,#53909,#53910,#53911,#53912,#53913,
#53914,#53915,#53916,#53917,#53918,#53919,#53920,#53921,#53922,#53923,#53924,
#53925,#53926,#53927,#53928,#53929,#53930,#53931,#53932,#53933,#53934,#53935,
#53936,#53937,#53938,#53939,#53940,#53941,#53942,#53943,#53944,#53945,#53946,
#53947,#53948,#53949,#53950,#53951,#53952,#53953,#53954,#53955,#53956,#53957,
#53958,#53959,#53960,#53961,#53962,#53963,#53964,#53965,#53966,#53967,#53968,
#53969,#53970,#53971,#53972,#53973,#53974,#53975,#53976,#53977,#53978,#53979,
#53980,#53981,#53982,#53983,#53984,#53985,#53986,#53987,#53988,#53989,#53990,
#53991,#53992,#53993,#53994,#53995,#53996,#53997,#53998,#53999,#54000,#54001,
#54002,#54003,#54004,#54005,#54006,#54007,#54008,#54009,#54010,#54011,#54012,
#54013,#54014,#54015,#54016,#54017,#54018,#54019,#54020,#54021,#54022,#54023,
#54024,#54025,#54026,#54027,#54028,#54029,#54030,#54031,#54032,#54033,#54034,
#54035,#54036,#54037,#54038,#54039,#54040,#54041,#54042,#54043,#54044,#54045,
#54046,#54047,#54048,#54049,#54050,#54051,#54052,#54053,#54054,#54055,#54056,
#54057,#54058,#54059,#54060,#54061,#54062,#54063,#54064,#54065,#54066,#54067,
#54068,#54069,#54070,#54071,#54072,#54073,#54074,#54075,#54076,#54077,#54078,
#54079,#54080,#54081,#54082,#54083,#54084,#54085,#54086,#54087,#54088,#54089,
#54090,#54091,#54092,#54093,#54094,#54095,#54096,#54097,#54098,#54099,#54100,
#54101,#54102,#54103,#54104,#54105,#54106,#54107,#54108,#54109,#54110,#54111,
#54112,#54113,#54114,#54115,#54116,#54117,#54118,#54119,#54120,#54121,#54122,
#54123,#54124,#54125,#54126,#54127,#54128,#54129,#54130,#54131,#54132,#54133,
#54134,#54135,#54136,#54137,#54138,#54139,#54140,#54141,#54142,#54143,#54144,
#54145,#54146,#54147,#54148,#54149,#54150,#54151,#54152,#54153,#54154,#54155,
#54156,#54157,#54158,#54159,#54160,#54161,#54162,#54163,#54164,#54165,#54166,
#54167,#54168,#54169,#54170,#54171,#54172,#54173,#54174,#54175,#54176,#54177,
#54178,#54179,#54180,#54181,#54182,#54183,#54184,#54185,#54186,#54187,#54188,
#54189,#54190,#54191,#54192,#54193,#54194,#54195,#54196,#54197,#54198,#54199,
#54200,#54201,#54202,#54203,#54204,#54205,#54206,#54207,#54208,#54209,#54210,
#54211,#54212,#54213,#54214,#54215,#54216,#54217,#54218,#54219,#54220,#54221,
#54222,#54223,#54224,#54225,#54226,#54227,#54228,#54229,#54230,#54231,#54232,
#54233,#54234,#54235,#54236,#54237,#54238,#54239,#54240,#54241,#54242,#54243,
#54244,#54245,#54246,#54247,#54248,#54249,#54250,#54251,#54252,#54253,#54254,
#54255,#54256,#54257,#54258,#54259,#54260,#54261,#54262,#54263,#54264,#54265,
#54266,#54267,#54268,#54269,#54270,#54271,#54272,#54273,#54274,#54275,#54276,
#54277,#54278,#54279,#54280,#54281,#54282,#54283,#54284,#54285,#54286,#54287,
#54288,#54289,#54290,#54291,#54292,#54293,#54294,#54295,#54296,#54297,#54298,
#54299,#54300,#54301,#54302,#54303,#54304,#54305,#54306,#54307,#54308,#54309,
#54310,#54311,#54312,#54313,#54314,#54315,#54316,#54317,#54318,#54319,#54320,
#54321,#54322,#54323,#54324,#54325,#54326,#54327,#54328,#54329,#54330,#54331,
#54332,#54333,#54334,#54335,#54336,#54337,#54338,#54339,#54340,#54341,#54342,
#54343,#54344,#54345,#54346,#54347,#54348,#54349,#54350,#54351,#54352,#54353,
#54354,#54355,#54356,#54357,#54358,#54359,#54360,#54361,#54362,#54363,#54364,
#54365,#54366,#54367,#54368,#54369,#54370,#54371,#54372,#54373,#54374,#54375),
(#54376,#54377,#54378,#54379,#54380,#54381,#54382,#54383,#54384,#54385,
#54386,#54387,#54388,#54389,#54390,#54391,#54392,#54393,#54394,#54395,#54396,
#54397,#54398,#54399,#54400,#54401,#54402,#54403,#54404,#54405,#54406,#54407,
#54408,#54409,#54410,#54411,#54412,#54413,#54414,#54415,#54416,#54417,#54418,
#54419,#54420,#54421,#54422,#54423,#54424,#54425,#54426,#54427,#54428,#54429,
#54430,#54431,#54432,#54433,#54434,#54435,#54436,#54437,#54438,#54439,#54440,
#54441,#54442,#54443,#54444,#54445,#54446,#54447,#54448,#54449,#54450,#54451,
#54452,#54453,#54454,#54455,#54456,#54457,#54458,#54459,#54460,#54461,#54462,
#54463,#54464,#54465,#54466,#54467,#54468,#54469,#54470,#54471,#54472,#54473,
#54474,#54475,#54476,#54477,#54478,#54479,#54480,#54481,#54482,#54483,#54484,
#54485,#54486,#54487,#54488,#54489,#54490,#54491,#54492,#54493,#54494,#54495,
#54496,#54497,#54498,#54499,#54500,#54501,#54502,#54503,#54504,#54505,#54506,
#54507,#54508,#54509,#54510,#54511,#54512,#54513,#54514,#54515,#54516,#54517,
#54518,#54519,#54520,#54521,#54522,#54523,#54524,#54525,#54526,#54527,#54528,
#54529,#54530,#54531,#54532,#54533,#54534,#54535,#54536,#54537,#54538,#54539,
#54540,#54541,#54542,#54543,#54544,#54545,#54546,#54547,#54548,#54549,#54550,
#54551,#54552,#54553,#54554,#54555,#54556,#54557,#54558,#54559,#54560,#54561,
#54562,#54563,#54564,#54565,#54566,#54567,#54568,#54569,#54570,#54571,#54572,
#54573,#54574,#54575,#54576,#54577,#54578,#54579,#54580,#54581,#54582,#54583,
#54584,#54585,#54586,#54587,#54588,#54589,#54590,#54591,#54592,#54593,#54594,
#54595,#54596,#54597,#54598,#54599,#54600,#54601,#54602,#54603,#54604,#54605,
#54606,#54607,#54608,#54609,#54610,#54611,#54612,#54613,#54614,#54615,#54616,
#54617,#54618,#54619,#54620,#54621,#54622,#54623,#54624,#54625,#54626,#54627,
#54628,#54629,#54630,#54631,#54632,#54633,#54634,#54635,#54636,#54637,#54638,
#54639,#54640,#54641,#54642,#54643,#54644,#54645,#54646,#54647,#54648,#54649,
#54650,#54651,#54652,#54653,#54654,#54655,#54656,#54657,#54658,#54659,#54660,
#54661,#54662,#54663,#54664,#54665,#54666,#54667,#54668,#54669,#54670,#54671,
#54672,#54673,#54674,#54675,#54676,#54677,#54678,#54679,#54680,#54681,#54682,
#54683,#54684,#54685,#54686,#54687,#54688,#54689,#54690,#54691,#54692,#54693,
#54694,#54695,#54696,#54697,#54698,#54699,#54700,#54701,#54702,#54703,#54704,
#54705,#54706,#54707,#54708,#54709,#54710,#54711,#54712,#54713,#54714,#54715,
#54716,#54717,#54718,#54719,#54720,#54721,#54722,#54723,#54724,#54725,#54726,
#54727,#54728,#54729,#54730,#54731,#54732,#54733,#54734,#54735,#54736,#54737,
#54738,#54739,#54740,#54741,#54742,#54743,#54744,#54745,#54746,#54747,#54748,
#54749,#54750,#54751,#54752,#54753,#54754,#54755,#54756,#54757,#54758,#54759,
#54760,#54761,#54762,#54763,#54764,#54765,#54766,#54767,#54768,#54769,#54770,
#54771,#54772,#54773,#54774,#54775,#54776,#54777,#54778,#54779,#54780,#54781,
#54782,#54783,#54784,#54785,#54786,#54787,#54788,#54789,#54790,#54791,#54792,
#54793,#54794,#54795,#54796,#54797,#54798,#54799,#54800,#54801,#54802,#54803,
#54804,#54805,#54806,#54807,#54808,#54809,#54810,#54811,#54812,#54813,#54814,
#54815,#54816,#54817,#54818,#54819,#54820,#54821,#54822,#54823,#54824,#54825,
#54826,#54827,#54828,#54829,#54830,#54831,#54832,#54833,#54834,#54835,#54836,
#54837,#54838,#54839,#54840,#54841,#54842,#54843,#54844,#54845,#54846,#54847,
#54848,#54849,#54850,#54851,#54852,#54853,#54854,#54855,#54856,#54857,#54858,
#54859,#54860,#54861,#54862,#54863,#54864,#54865,#54866,#54867,#54868,#54869,
#54870,#54871,#54872,#54873,#54874,#54875,#54876,#54877,#54878,#54879,#54880,
#54881,#54882,#54883),(#54884,#54885,#54886,#54887,#54888,#54889,#54890,
#54891,#54892,#54893,#54894,#54895,#54896,#54897,#54898,#54899,#54900,#54901,
#54902,#54903,#54904,#54905,#54906,#54907,#54908,#54909,#54910,#54911,#54912,
#54913,#54914,#54915,#54916,#54917,#54918,#54919,#54920,#54921,#54922,#54923,
#54924,#54925,#54926,#54927,#54928,#54929,#54930,#54931,#54932,#54933,#54934,
#54935,#54936,#54937,#54938,#54939,#54940,#54941,#54942,#54943,#54944,#54945,
#54946,#54947,#54948,#54949,#54950,#54951,#54952,#54953,#54954,#54955,#54956,
#54957,#54958,#54959,#54960,#54961,#54962,#54963,#54964,#54965,#54966,#54967,
#54968,#54969,#54970,#54971,#54972,#54973,#54974,#54975,#54976,#54977,#54978,
#54979,#54980,#54981,#54982,#54983,#54984,#54985,#54986,#54987,#54988,#54989,
#54990,#54991,#54992,#54993,#54994,#54995,#54996,#54997,#54998,#54999,#55000,
#55001,#55002,#55003,#55004,#55005,#55006,#55007,#55008,#55009,#55010,#55011,
#55012,#55013,#55014,#55015,#55016,#55017,#55018,#55019,#55020,#55021,#55022,
#55023,#55024,#55025,#55026,#55027,#55028,#55029,#55030,#55031,#55032,#55033,
#55034,#55035,#55036,#55037,#55038,#55039,#55040,#55041,#55042,#55043,#55044,
#55045,#55046,#55047,#55048,#55049,#55050,#55051,#55052,#55053,#55054,#55055,
#55056,#55057,#55058,#55059,#55060,#55061,#55062,#55063,#55064,#55065,#55066,
#55067,#55068,#55069,#55070,#55071,#55072,#55073,#55074,#55075,#55076,#55077,
#55078,#55079,#55080,#55081,#55082,#55083,#55084,#55085,#55086,#55087,#55088,
#55089,#55090,#55091,#55092,#55093,#55094,#55095,#55096,#55097,#55098,#55099,
#55100,#55101,#55102,#55103,#55104,#55105,#55106,#55107,#55108,#55109,#55110,
#55111,#55112,#55113,#55114,#55115,#55116,#55117,#55118,#55119,#55120,#55121,
#55122,#55123,#55124,#55125,#55126,#55127,#55128,#55129,#55130,#55131,#55132,
#55133,#55134,#55135,#55136,#55137,#55138,#55139,#55140,#55141,#55142,#55143,
#55144,#55145,#55146,#55147,#55148,#55149,#55150,#55151,#55152,#55153,#55154,
#55155,#55156,#55157,#55158,#55159,#55160,#55161,#55162,#55163,#55164,#55165,
#55166,#55167,#55168,#55169,#55170,#55171,#55172,#55173,#55174,#55175,#55176,
#55177,#55178,#55179,#55180,#55181,#55182,#55183,#55184,#55185,#55186,#55187,
#55188,#55189,#55190,#55191,#55192,#55193,#55194,#55195,#55196,#55197,#55198,
#55199,#55200,#55201,#55202,#55203,#55204,#55205,#55206,#55207,#55208,#55209,
#55210,#55211,#55212,#55213,#55214,#55215,#55216,#55217,#55218,#55219,#55220,
#55221,#55222,#55223,#55224,#55225,#55226,#55227,#55228,#55229,#55230,#55231,
#55232,#55233,#55234,#55235,#55236,#55237,#55238,#55239,#55240,#55241,#55242,
#55243,#55244,#55245,#55246,#55247,#55248,#55249,#55250,#55251,#55252,#55253,
#55254,#55255,#55256,#55257,#55258,#55259,#55260,#55261,#55262,#55263,#55264,
#55265,#55266,#55267,#55268,#55269,#55270,#55271,#55272,#55273,#55274,#55275,
#55276,#55277,#55278,#55279,#55280,#55281,#55282,#55283,#55284,#55285,#55286,
#55287,#55288,#55289,#55290,#55291,#55292,#55293,#55294,#55295,#55296,#55297,
#55298,#55299,#55300,#55301,#55302,#55303,#55304,#55305,#55306,#55307,#55308,
#55309,#55310,#55311,#55312,#55313,#55314,#55315,#55316,#55317,#55318,#55319,
#55320,#55321,#55322,#55323,#55324,#55325,#55326,#55327,#55328,#55329,#55330,
#55331,#55332,#55333,#55334,#55335,#55336,#55337,#55338,#55339,#55340,#55341,
#55342,#55343,#55344,#55345,#55346,#55347,#55348,#55349,#55350,#55351,#55352,
#55353,#55354,#55355,#55356,#55357,#55358,#55359,#55360,#55361,#55362,#55363,
#55364,#55365,#55366,#55367,#55368,#55369,#55370,#55371,#55372,#55373,#55374,
#55375,#55376,#55377,#55378,#55379,#55380,#55381,#55382,#55383,#55384,#55385,
#55386,#55387,#55388,#55389,#55390,#55391)),.UNSPECIFIED.,.F.,.F.,.F.,(4,
4),(4,1,1,1,1,1,1,1,1,1,1,1,1,1,1,1,1,1,1,1,1,1,1,1,1,1,1,1,1,1,1,1,1,1,
1,1,1,1,1,1,1,1,1,1,1,1,1,1,1,1,1,1,1,1,1,1,1,1,1,1,1,1,1,1,1,1,1,1,1,1,
1,1,1,1,1,1,1,1,1,1,1,1,1,1,1,1,1,1,1,1,1,1,1,1,1,1,1,1,1,1,1,1,1,1,1,1,
1,1,1,1,1,1,1,1,1,1,1,1,1,1,1,1,1,1,1,1,1,1,1,1,1,1,1,1,1,1,1,1,1,1,1,1,
1,1,1,1,1,1,1,1,1,1,1,1,1,1,1,1,1,1,1,1,1,1,1,1,1,1,1,1,1,1,1,1,1,1,1,1,
1,1,1,1,1,1,1,1,1,1,1,1,1,1,1,1,1,1,1,1,1,1,1,1,1,1,1,1,1,1,1,1,1,1,1,1,
1,1,1,1,1,1,1,1,1,1,1,1,1,1,1,1,1,1,1,1,1,1,1,1,1,1,1,1,1,1,1,1,1,1,1,1,
1,1,1,1,1,1,1,1,1,1,1,1,1,1,1,1,1,1,1,1,1,1,1,1,1,1,1,1,1,1,1,1,1,1,1,1,
1,1,1,1,1,1,1,1,1,1,1,1,1,1,1,1,1,1,1,1,1,1,1,1,1,1,1,1,1,1,1,1,1,1,1,1,
1,1,1,1,1,1,1,1,1,1,1,1,1,1,1,1,1,1,1,1,1,1,1,1,1,1,1,1,1,1,1,1,1,1,1,1,
1,1,1,1,1,1,1,1,1,1,1,1,1,1,1,1,1,1,1,1,1,1,1,1,1,1,1,1,1,1,1,1,1,1,1,1,
1,1,1,1,1,1,1,1,1,1,1,1,1,1,1,1,1,1,1,1,1,1,1,1,1,1,1,1,1,1,1,1,1,1,1,1,
1,1,1,1,1,1,1,1,1,1,1,1,1,1,1,1,1,1,1,1,1,1,1,1,1,1,1,1,1,1,1,1,1,1,1,1,
1,1,1,1,1,1,1,1,1,1,1,1,1,1,1,1,1,1,1,1,1,1,1,1,1,1,1,1,1,1,1,1,1,1,1,1,
1,1,1,4),(0.,0.115296848757168),(10.2062663725606,10.7060917058189,11.2059170390771,
12.2055677055937,13.2052183721102,14.2048690386268,15.2045197051434,16.2041703716599,
17.2038210381765,18.203471704693,19.2031223712096,20.2027730377261,21.2024237042427,
22.2020743707592,23.2017250372758,24.2013757037923,25.2010263703089,26.2006770368254,
27.200327703342,28.1999783698585,29.1996290363751,30.1992797028916,31.1989303694082,
32.1985810359247,33.1982317024413,34.1978823689578,35.1975330354744,36.1971837019909,
37.1968343685075,38.196485035024,39.1961357015406,40.1957863680571,41.1954370345737,
42.1950877010902,43.1947383676068,44.1943890341233,45.1940397006399,46.1936903671564,
47.193341033673,48.1929917001895,49.1926423667061,50.1922930332226,51.1919436997392,
52.1915943662557,53.1912450327723,54.1908956992888,55.1905463658054,56.1901970323219,
57.1898476988385,58.189498365355,59.1891490318716,60.1887996983882,61.1884503649047,
62.1881010314213,63.1877516979378,64.1874023644544,65.1870530309709,66.1867036974875,
67.186354364004,68.1860050305206,69.1856556970371,70.1853063635537,71.1849570300702,
72.1846076965868,73.1842583631033,74.1839090296199,75.1835596961364,76.183210362653,
77.1828610291695,78.1825116956861,79.1821623622026,80.1818130287192,81.1814636952357,
82.1811143617523,83.1807650282688,84.1804156947854,85.1800663613019,86.1797170278185,
87.179367694335,88.1790183608516,89.1786690273681,90.1783196938847,91.1779703604012,
92.1776210269178,93.1772716934343,94.1769223599509,95.1765730264674,96.176223692984,
97.1758743595006,98.1755250260171,99.1751756925336,100.17482635905,101.174477025567,
102.174127692083,103.1737783586,104.173429025116,105.173079691633,106.17273035815,
107.172381024666,108.172031691183,109.171682357699,110.171333024216,111.170983690732,
112.170634357249,113.170285023765,114.169935690282,115.169586356798,116.169237023315,
117.168887689832,118.168538356348,119.168189022865,120.167839689381,121.167490355898,
122.167141022414,123.166791688931,124.166442355447,125.166093021964,126.165743688481,
127.165394354997,128.165045021514,129.16469568803,130.164346354547,131.163997021063,
132.16364768758,133.163298354096,134.162949020613,135.16259968713,136.162250353646,
137.161901020163,138.161551686679,139.161202353196,140.160853019712,141.160503686229,
142.160154352745,143.159805019262,144.159455685778,145.159106352295,146.158757018812,
147.158407685328,148.158058351845,149.157709018361,150.157359684878,151.157010351394,
152.156661017911,153.156311684427,154.155962350944,155.155613017461,156.155263683977,
157.154914350494,158.15456501701,159.154215683527,160.153866350043,161.15351701656,
162.153167683076,163.152818349593,164.152469016109,165.152119682626,166.151770349143,
167.151421015659,168.151071682176,169.150722348692,170.150373015209,171.150023681725,
172.149674348242,173.149325014758,174.148975681275,175.148626347792,176.148277014308,
177.147927680825,178.147578347341,179.147229013858,180.146879680374,181.146530346891,
182.146181013407,183.145831679924,184.145482346441,185.145133012957,186.144783679474,
187.14443434599,188.144085012507,189.143735679023,190.14338634554,191.143037012056,
192.142687678573,193.142338345089,194.141989011606,195.141639678123,196.141290344639,
197.140941011156,198.140591677672,199.140242344189,200.139893010705,201.139543677222,
202.139194343738,203.138845010255,204.138495676772,205.138146343288,206.137797009805,
207.137447676321,208.137098342838,209.136749009354,210.136399675871,211.136050342387,
212.135701008904,213.135351675421,214.135002341937,215.134653008454,216.13430367497,
217.133954341487,218.133605008003,219.13325567452,220.132906341036,221.132557007553,
222.132207674069,223.131858340586,224.131509007103,225.131159673619,226.130810340136,
227.130461006652,228.130111673169,229.129762339685,230.129413006202,231.129063672718,
232.128714339235,233.128365005752,234.128015672268,235.127666338785,236.127317005301,
237.126967671818,238.126618338334,239.126269004851,240.125919671367,241.125570337884,
242.1252210044,243.124871670917,244.124522337434,245.12417300395,246.123823670467,
247.123474336983,248.1231250035,249.122775670016,250.122426336533,251.122077003049,
252.121727669566,253.121378336083,254.121029002599,255.120679669116,256.120330335632,
257.119981002149,258.119631668665,259.119282335182,260.118933001698,261.118583668215,
262.118234334731,263.117885001248,264.117535667765,265.117186334281,266.116837000798,
267.116487667314,268.116138333831,269.115789000347,270.115439666864,271.11509033338,
272.114740999897,273.114391666414,274.11404233293,275.113692999447,276.113343665963,
277.11299433248,278.112644998996,279.112295665513,280.111946332029,281.111596998546,
282.111247665063,283.110898331579,284.110548998096,285.110199664612,286.109850331129,
287.109500997645,288.109151664162,289.108802330678,290.108452997195,291.108103663712,
292.107754330228,293.107404996745,294.107055663261,295.106706329778,296.106356996294,
297.106007662811,298.105658329327,299.105308995844,300.10495966236,301.104610328877,
302.104260995394,303.10391166191,304.103562328427,305.103212994943,306.10286366146,
307.102514327976,308.102164994493,309.101815661009,310.101466327526,311.101116994043,
312.100767660559,313.100418327076,314.100068993592,315.099719660109,316.099370326625,
317.099020993142,318.098671659658,319.098322326175,320.097972992691,321.097623659208,
322.097274325725,323.096924992241,324.096575658758,325.096226325274,326.095876991791,
327.095527658307,328.095178324824,329.09482899134,330.094479657857,331.094130324374,
332.09378099089,333.093431657407,334.093082323923,335.09273299044,336.092383656956,
337.092034323473,338.091684989989,339.091335656506,340.090986323022,341.090636989539,
342.090287656056,343.089938322572,344.089588989089,345.089239655605,346.088890322122,
347.088540988638,348.088191655155,349.087842321671,350.087492988188,351.087143654705,
352.086794321221,353.086444987738,354.086095654254,355.085746320771,356.085396987287,
357.085047653804,358.08469832032,359.084348986837,360.083999653354,361.08365031987,
362.083300986387,363.082951652903,364.08260231942,365.082252985936,366.081903652453,
367.081554318969,368.081204985486,369.080855652002,370.080506318519,371.080156985036,
372.079807651552,373.079458318069,374.079108984585,375.078759651102,376.078410317618,
377.078060984135,378.077711650651,379.077362317168,380.077012983685,381.076663650201,
382.076314316718,383.075964983234,384.075615649751,385.075266316267,386.074916982784,
387.0745676493,388.074218315817,389.073868982334,390.07351964885,391.073170315367,
392.072820981883,393.0724716484,394.072122314916,395.071772981433,396.071423647949,
397.071074314466,398.070724980982,399.070375647499,400.070026314016,401.069676980532,
402.069327647049,403.068978313565,404.068628980082,405.068279646598,406.067930313115,
407.067580979631,408.067231646148,409.066882312665,410.066532979181,411.066183645698,
412.065834312214,413.065484978731,414.065135645247,415.064786311764,416.06443697828,
417.064087644797,418.063738311314,419.06338897783,420.063039644347,421.062690310863,
422.06234097738,423.061991643896,424.061642310413,425.061292976929,426.060943643446,
427.060594309962,428.060244976479,429.059895642996,430.059546309512,431.059196976029,
432.058847642545,433.058498309062,434.058148975578,435.057799642095,436.057450308611,
437.057100975128,438.056751641645,439.056402308161,440.056052974678,441.055703641194,
442.055354307711,443.055004974227,444.054655640744,445.05430630726,446.053956973777,
447.053607640293,448.05325830681,449.052908973327,450.052559639843,451.05221030636,
452.051860972876,453.051511639393,454.051162305909,455.050812972426,456.050463638942,
457.050114305459,458.049764971976,459.049415638492,460.049066305009,461.048716971525,
462.048367638042,463.048018304558,464.047668971075,465.047319637591,466.046970304108,
467.046620970625,468.046271637141,469.045922303658,470.045572970174,471.045223636691,
472.044874303207,473.044524969724,474.04417563624,475.043826302757,476.043476969273,
477.04312763579,478.042778302307,479.042428968823,480.04207963534,481.041730301856,
482.041380968373,483.041031634889,484.040682301406,485.040332967922,486.039983634439,
487.039634300956,488.039284967472,489.038935633989,490.038586300505,491.038236967022,
492.037887633538,493.037538300055,494.037188966571,495.036839633088,496.036490299605,
497.036140966121,498.035791632638,499.035442299154,500.035092965671,501.034743632187,
502.034394298704,503.03404496522,504.033695631737,505.033346298253,506.03299696477,
507.032647631287,508.032298297803,509.03194896432,510.031599630836,511.031250297353,
512.030900963869,512.530726297128,513.030551630386),.UNSPECIFIED.);
#261=B_SPLINE_SURFACE_WITH_KNOTS('',3,3,((#55434,#55435,#55436,#55437,#55438,
#55439,#55440,#55441,#55442,#55443,#55444,#55445,#55446,#55447,#55448,#55449,
#55450,#55451,#55452,#55453,#55454,#55455,#55456,#55457,#55458,#55459,#55460,
#55461,#55462,#55463,#55464,#55465,#55466,#55467,#55468,#55469,#55470,#55471,
#55472,#55473,#55474,#55475,#55476,#55477,#55478,#55479,#55480,#55481,#55482,
#55483,#55484,#55485,#55486,#55487,#55488,#55489,#55490,#55491,#55492,#55493,
#55494,#55495,#55496,#55497,#55498,#55499,#55500,#55501,#55502,#55503,#55504,
#55505,#55506,#55507,#55508,#55509,#55510,#55511,#55512,#55513,#55514,#55515,
#55516,#55517,#55518,#55519,#55520,#55521,#55522,#55523,#55524,#55525,#55526,
#55527,#55528,#55529,#55530,#55531,#55532,#55533,#55534,#55535,#55536,#55537,
#55538,#55539,#55540,#55541,#55542,#55543,#55544,#55545,#55546,#55547,#55548,
#55549,#55550,#55551,#55552,#55553,#55554,#55555,#55556,#55557,#55558,#55559,
#55560,#55561,#55562,#55563,#55564,#55565,#55566,#55567,#55568,#55569,#55570,
#55571,#55572,#55573,#55574,#55575,#55576,#55577,#55578,#55579,#55580,#55581,
#55582,#55583,#55584,#55585,#55586,#55587,#55588,#55589,#55590,#55591,#55592,
#55593,#55594,#55595,#55596,#55597,#55598,#55599,#55600,#55601,#55602,#55603,
#55604,#55605,#55606,#55607,#55608,#55609,#55610,#55611,#55612,#55613,#55614,
#55615,#55616,#55617,#55618,#55619,#55620,#55621,#55622,#55623,#55624,#55625,
#55626,#55627,#55628,#55629,#55630,#55631,#55632,#55633,#55634,#55635,#55636,
#55637,#55638,#55639,#55640,#55641,#55642,#55643,#55644,#55645,#55646,#55647,
#55648,#55649,#55650,#55651,#55652,#55653,#55654,#55655,#55656,#55657,#55658,
#55659,#55660,#55661,#55662,#55663,#55664,#55665,#55666,#55667,#55668,#55669,
#55670,#55671,#55672,#55673,#55674,#55675,#55676,#55677,#55678,#55679,#55680,
#55681,#55682,#55683,#55684,#55685,#55686,#55687,#55688,#55689,#55690,#55691,
#55692,#55693,#55694,#55695,#55696,#55697,#55698,#55699,#55700,#55701,#55702,
#55703,#55704,#55705,#55706,#55707,#55708,#55709,#55710,#55711,#55712,#55713,
#55714,#55715,#55716,#55717,#55718,#55719,#55720,#55721,#55722,#55723,#55724,
#55725,#55726,#55727,#55728,#55729,#55730,#55731,#55732,#55733,#55734,#55735,
#55736,#55737,#55738,#55739,#55740,#55741,#55742,#55743,#55744,#55745,#55746,
#55747,#55748,#55749,#55750,#55751,#55752,#55753,#55754,#55755,#55756,#55757,
#55758,#55759,#55760,#55761,#55762,#55763,#55764,#55765,#55766,#55767,#55768,
#55769,#55770,#55771,#55772,#55773,#55774,#55775,#55776,#55777,#55778,#55779,
#55780,#55781,#55782,#55783,#55784,#55785,#55786,#55787,#55788,#55789,#55790,
#55791,#55792,#55793,#55794,#55795,#55796,#55797,#55798,#55799,#55800,#55801,
#55802,#55803,#55804,#55805,#55806,#55807,#55808,#55809,#55810,#55811,#55812,
#55813,#55814,#55815,#55816,#55817,#55818,#55819,#55820,#55821,#55822,#55823,
#55824,#55825,#55826,#55827,#55828,#55829,#55830,#55831,#55832,#55833,#55834,
#55835,#55836,#55837,#55838,#55839,#55840,#55841,#55842,#55843,#55844,#55845,
#55846,#55847,#55848,#55849,#55850,#55851,#55852,#55853,#55854,#55855,#55856,
#55857,#55858,#55859,#55860,#55861,#55862,#55863,#55864,#55865,#55866,#55867,
#55868,#55869,#55870,#55871,#55872,#55873,#55874,#55875,#55876,#55877,#55878,
#55879,#55880,#55881,#55882,#55883,#55884,#55885,#55886,#55887,#55888,#55889,
#55890,#55891,#55892,#55893,#55894,#55895,#55896,#55897,#55898,#55899,#55900,
#55901,#55902,#55903,#55904,#55905,#55906,#55907,#55908,#55909,#55910,#55911,
#55912,#55913,#55914,#55915,#55916,#55917,#55918,#55919,#55920,#55921,#55922,
#55923,#55924,#55925,#55926,#55927,#55928,#55929,#55930,#55931,#55932,#55933,
#55934,#55935,#55936,#55937,#55938,#55939,#55940,#55941,#55942,#55943),
(#55944,#55945,#55946,#55947,#55948,#55949,#55950,#55951,#55952,#55953,
#55954,#55955,#55956,#55957,#55958,#55959,#55960,#55961,#55962,#55963,#55964,
#55965,#55966,#55967,#55968,#55969,#55970,#55971,#55972,#55973,#55974,#55975,
#55976,#55977,#55978,#55979,#55980,#55981,#55982,#55983,#55984,#55985,#55986,
#55987,#55988,#55989,#55990,#55991,#55992,#55993,#55994,#55995,#55996,#55997,
#55998,#55999,#56000,#56001,#56002,#56003,#56004,#56005,#56006,#56007,#56008,
#56009,#56010,#56011,#56012,#56013,#56014,#56015,#56016,#56017,#56018,#56019,
#56020,#56021,#56022,#56023,#56024,#56025,#56026,#56027,#56028,#56029,#56030,
#56031,#56032,#56033,#56034,#56035,#56036,#56037,#56038,#56039,#56040,#56041,
#56042,#56043,#56044,#56045,#56046,#56047,#56048,#56049,#56050,#56051,#56052,
#56053,#56054,#56055,#56056,#56057,#56058,#56059,#56060,#56061,#56062,#56063,
#56064,#56065,#56066,#56067,#56068,#56069,#56070,#56071,#56072,#56073,#56074,
#56075,#56076,#56077,#56078,#56079,#56080,#56081,#56082,#56083,#56084,#56085,
#56086,#56087,#56088,#56089,#56090,#56091,#56092,#56093,#56094,#56095,#56096,
#56097,#56098,#56099,#56100,#56101,#56102,#56103,#56104,#56105,#56106,#56107,
#56108,#56109,#56110,#56111,#56112,#56113,#56114,#56115,#56116,#56117,#56118,
#56119,#56120,#56121,#56122,#56123,#56124,#56125,#56126,#56127,#56128,#56129,
#56130,#56131,#56132,#56133,#56134,#56135,#56136,#56137,#56138,#56139,#56140,
#56141,#56142,#56143,#56144,#56145,#56146,#56147,#56148,#56149,#56150,#56151,
#56152,#56153,#56154,#56155,#56156,#56157,#56158,#56159,#56160,#56161,#56162,
#56163,#56164,#56165,#56166,#56167,#56168,#56169,#56170,#56171,#56172,#56173,
#56174,#56175,#56176,#56177,#56178,#56179,#56180,#56181,#56182,#56183,#56184,
#56185,#56186,#56187,#56188,#56189,#56190,#56191,#56192,#56193,#56194,#56195,
#56196,#56197,#56198,#56199,#56200,#56201,#56202,#56203,#56204,#56205,#56206,
#56207,#56208,#56209,#56210,#56211,#56212,#56213,#56214,#56215,#56216,#56217,
#56218,#56219,#56220,#56221,#56222,#56223,#56224,#56225,#56226,#56227,#56228,
#56229,#56230,#56231,#56232,#56233,#56234,#56235,#56236,#56237,#56238,#56239,
#56240,#56241,#56242,#56243,#56244,#56245,#56246,#56247,#56248,#56249,#56250,
#56251,#56252,#56253,#56254,#56255,#56256,#56257,#56258,#56259,#56260,#56261,
#56262,#56263,#56264,#56265,#56266,#56267,#56268,#56269,#56270,#56271,#56272,
#56273,#56274,#56275,#56276,#56277,#56278,#56279,#56280,#56281,#56282,#56283,
#56284,#56285,#56286,#56287,#56288,#56289,#56290,#56291,#56292,#56293,#56294,
#56295,#56296,#56297,#56298,#56299,#56300,#56301,#56302,#56303,#56304,#56305,
#56306,#56307,#56308,#56309,#56310,#56311,#56312,#56313,#56314,#56315,#56316,
#56317,#56318,#56319,#56320,#56321,#56322,#56323,#56324,#56325,#56326,#56327,
#56328,#56329,#56330,#56331,#56332,#56333,#56334,#56335,#56336,#56337,#56338,
#56339,#56340,#56341,#56342,#56343,#56344,#56345,#56346,#56347,#56348,#56349,
#56350,#56351,#56352,#56353,#56354,#56355,#56356,#56357,#56358,#56359,#56360,
#56361,#56362,#56363,#56364,#56365,#56366,#56367,#56368,#56369,#56370,#56371,
#56372,#56373,#56374,#56375,#56376,#56377,#56378,#56379,#56380,#56381,#56382,
#56383,#56384,#56385,#56386,#56387,#56388,#56389,#56390,#56391,#56392,#56393,
#56394,#56395,#56396,#56397,#56398,#56399,#56400,#56401,#56402,#56403,#56404,
#56405,#56406,#56407,#56408,#56409,#56410,#56411,#56412,#56413,#56414,#56415,
#56416,#56417,#56418,#56419,#56420,#56421,#56422,#56423,#56424,#56425,#56426,
#56427,#56428,#56429,#56430,#56431,#56432,#56433,#56434,#56435,#56436,#56437,
#56438,#56439,#56440,#56441,#56442,#56443,#56444,#56445,#56446,#56447,#56448,
#56449,#56450,#56451,#56452,#56453),(#56454,#56455,#56456,#56457,#56458,
#56459,#56460,#56461,#56462,#56463,#56464,#56465,#56466,#56467,#56468,#56469,
#56470,#56471,#56472,#56473,#56474,#56475,#56476,#56477,#56478,#56479,#56480,
#56481,#56482,#56483,#56484,#56485,#56486,#56487,#56488,#56489,#56490,#56491,
#56492,#56493,#56494,#56495,#56496,#56497,#56498,#56499,#56500,#56501,#56502,
#56503,#56504,#56505,#56506,#56507,#56508,#56509,#56510,#56511,#56512,#56513,
#56514,#56515,#56516,#56517,#56518,#56519,#56520,#56521,#56522,#56523,#56524,
#56525,#56526,#56527,#56528,#56529,#56530,#56531,#56532,#56533,#56534,#56535,
#56536,#56537,#56538,#56539,#56540,#56541,#56542,#56543,#56544,#56545,#56546,
#56547,#56548,#56549,#56550,#56551,#56552,#56553,#56554,#56555,#56556,#56557,
#56558,#56559,#56560,#56561,#56562,#56563,#56564,#56565,#56566,#56567,#56568,
#56569,#56570,#56571,#56572,#56573,#56574,#56575,#56576,#56577,#56578,#56579,
#56580,#56581,#56582,#56583,#56584,#56585,#56586,#56587,#56588,#56589,#56590,
#56591,#56592,#56593,#56594,#56595,#56596,#56597,#56598,#56599,#56600,#56601,
#56602,#56603,#56604,#56605,#56606,#56607,#56608,#56609,#56610,#56611,#56612,
#56613,#56614,#56615,#56616,#56617,#56618,#56619,#56620,#56621,#56622,#56623,
#56624,#56625,#56626,#56627,#56628,#56629,#56630,#56631,#56632,#56633,#56634,
#56635,#56636,#56637,#56638,#56639,#56640,#56641,#56642,#56643,#56644,#56645,
#56646,#56647,#56648,#56649,#56650,#56651,#56652,#56653,#56654,#56655,#56656,
#56657,#56658,#56659,#56660,#56661,#56662,#56663,#56664,#56665,#56666,#56667,
#56668,#56669,#56670,#56671,#56672,#56673,#56674,#56675,#56676,#56677,#56678,
#56679,#56680,#56681,#56682,#56683,#56684,#56685,#56686,#56687,#56688,#56689,
#56690,#56691,#56692,#56693,#56694,#56695,#56696,#56697,#56698,#56699,#56700,
#56701,#56702,#56703,#56704,#56705,#56706,#56707,#56708,#56709,#56710,#56711,
#56712,#56713,#56714,#56715,#56716,#56717,#56718,#56719,#56720,#56721,#56722,
#56723,#56724,#56725,#56726,#56727,#56728,#56729,#56730,#56731,#56732,#56733,
#56734,#56735,#56736,#56737,#56738,#56739,#56740,#56741,#56742,#56743,#56744,
#56745,#56746,#56747,#56748,#56749,#56750,#56751,#56752,#56753,#56754,#56755,
#56756,#56757,#56758,#56759,#56760,#56761,#56762,#56763,#56764,#56765,#56766,
#56767,#56768,#56769,#56770,#56771,#56772,#56773,#56774,#56775,#56776,#56777,
#56778,#56779,#56780,#56781,#56782,#56783,#56784,#56785,#56786,#56787,#56788,
#56789,#56790,#56791,#56792,#56793,#56794,#56795,#56796,#56797,#56798,#56799,
#56800,#56801,#56802,#56803,#56804,#56805,#56806,#56807,#56808,#56809,#56810,
#56811,#56812,#56813,#56814,#56815,#56816,#56817,#56818,#56819,#56820,#56821,
#56822,#56823,#56824,#56825,#56826,#56827,#56828,#56829,#56830,#56831,#56832,
#56833,#56834,#56835,#56836,#56837,#56838,#56839,#56840,#56841,#56842,#56843,
#56844,#56845,#56846,#56847,#56848,#56849,#56850,#56851,#56852,#56853,#56854,
#56855,#56856,#56857,#56858,#56859,#56860,#56861,#56862,#56863,#56864,#56865,
#56866,#56867,#56868,#56869,#56870,#56871,#56872,#56873,#56874,#56875,#56876,
#56877,#56878,#56879,#56880,#56881,#56882,#56883,#56884,#56885,#56886,#56887,
#56888,#56889,#56890,#56891,#56892,#56893,#56894,#56895,#56896,#56897,#56898,
#56899,#56900,#56901,#56902,#56903,#56904,#56905,#56906,#56907,#56908,#56909,
#56910,#56911,#56912,#56913,#56914,#56915,#56916,#56917,#56918,#56919,#56920,
#56921,#56922,#56923,#56924,#56925,#56926,#56927,#56928,#56929,#56930,#56931,
#56932,#56933,#56934,#56935,#56936,#56937,#56938,#56939,#56940,#56941,#56942,
#56943,#56944,#56945,#56946,#56947,#56948,#56949,#56950,#56951,#56952,#56953,
#56954,#56955,#56956,#56957,#56958,#56959,#56960,#56961,#56962,#56963),
(#56964,#56965,#56966,#56967,#56968,#56969,#56970,#56971,#56972,#56973,
#56974,#56975,#56976,#56977,#56978,#56979,#56980,#56981,#56982,#56983,#56984,
#56985,#56986,#56987,#56988,#56989,#56990,#56991,#56992,#56993,#56994,#56995,
#56996,#56997,#56998,#56999,#57000,#57001,#57002,#57003,#57004,#57005,#57006,
#57007,#57008,#57009,#57010,#57011,#57012,#57013,#57014,#57015,#57016,#57017,
#57018,#57019,#57020,#57021,#57022,#57023,#57024,#57025,#57026,#57027,#57028,
#57029,#57030,#57031,#57032,#57033,#57034,#57035,#57036,#57037,#57038,#57039,
#57040,#57041,#57042,#57043,#57044,#57045,#57046,#57047,#57048,#57049,#57050,
#57051,#57052,#57053,#57054,#57055,#57056,#57057,#57058,#57059,#57060,#57061,
#57062,#57063,#57064,#57065,#57066,#57067,#57068,#57069,#57070,#57071,#57072,
#57073,#57074,#57075,#57076,#57077,#57078,#57079,#57080,#57081,#57082,#57083,
#57084,#57085,#57086,#57087,#57088,#57089,#57090,#57091,#57092,#57093,#57094,
#57095,#57096,#57097,#57098,#57099,#57100,#57101,#57102,#57103,#57104,#57105,
#57106,#57107,#57108,#57109,#57110,#57111,#57112,#57113,#57114,#57115,#57116,
#57117,#57118,#57119,#57120,#57121,#57122,#57123,#57124,#57125,#57126,#57127,
#57128,#57129,#57130,#57131,#57132,#57133,#57134,#57135,#57136,#57137,#57138,
#57139,#57140,#57141,#57142,#57143,#57144,#57145,#57146,#57147,#57148,#57149,
#57150,#57151,#57152,#57153,#57154,#57155,#57156,#57157,#57158,#57159,#57160,
#57161,#57162,#57163,#57164,#57165,#57166,#57167,#57168,#57169,#57170,#57171,
#57172,#57173,#57174,#57175,#57176,#57177,#57178,#57179,#57180,#57181,#57182,
#57183,#57184,#57185,#57186,#57187,#57188,#57189,#57190,#57191,#57192,#57193,
#57194,#57195,#57196,#57197,#57198,#57199,#57200,#57201,#57202,#57203,#57204,
#57205,#57206,#57207,#57208,#57209,#57210,#57211,#57212,#57213,#57214,#57215,
#57216,#57217,#57218,#57219,#57220,#57221,#57222,#57223,#57224,#57225,#57226,
#57227,#57228,#57229,#57230,#57231,#57232,#57233,#57234,#57235,#57236,#57237,
#57238,#57239,#57240,#57241,#57242,#57243,#57244,#57245,#57246,#57247,#57248,
#57249,#57250,#57251,#57252,#57253,#57254,#57255,#57256,#57257,#57258,#57259,
#57260,#57261,#57262,#57263,#57264,#57265,#57266,#57267,#57268,#57269,#57270,
#57271,#57272,#57273,#57274,#57275,#57276,#57277,#57278,#57279,#57280,#57281,
#57282,#57283,#57284,#57285,#57286,#57287,#57288,#57289,#57290,#57291,#57292,
#57293,#57294,#57295,#57296,#57297,#57298,#57299,#57300,#57301,#57302,#57303,
#57304,#57305,#57306,#57307,#57308,#57309,#57310,#57311,#57312,#57313,#57314,
#57315,#57316,#57317,#57318,#57319,#57320,#57321,#57322,#57323,#57324,#57325,
#57326,#57327,#57328,#57329,#57330,#57331,#57332,#57333,#57334,#57335,#57336,
#57337,#57338,#57339,#57340,#57341,#57342,#57343,#57344,#57345,#57346,#57347,
#57348,#57349,#57350,#57351,#57352,#57353,#57354,#57355,#57356,#57357,#57358,
#57359,#57360,#57361,#57362,#57363,#57364,#57365,#57366,#57367,#57368,#57369,
#57370,#57371,#57372,#57373,#57374,#57375,#57376,#57377,#57378,#57379,#57380,
#57381,#57382,#57383,#57384,#57385,#57386,#57387,#57388,#57389,#57390,#57391,
#57392,#57393,#57394,#57395,#57396,#57397,#57398,#57399,#57400,#57401,#57402,
#57403,#57404,#57405,#57406,#57407,#57408,#57409,#57410,#57411,#57412,#57413,
#57414,#57415,#57416,#57417,#57418,#57419,#57420,#57421,#57422,#57423,#57424,
#57425,#57426,#57427,#57428,#57429,#57430,#57431,#57432,#57433,#57434,#57435,
#57436,#57437,#57438,#57439,#57440,#57441,#57442,#57443,#57444,#57445,#57446,
#57447,#57448,#57449,#57450,#57451,#57452,#57453,#57454,#57455,#57456,#57457,
#57458,#57459,#57460,#57461,#57462,#57463,#57464,#57465,#57466,#57467,#57468,
#57469,#57470,#57471,#57472,#57473)),.UNSPECIFIED.,.F.,.F.,.F.,(4,4),(4,
1,1,1,1,1,1,1,1,1,1,1,1,1,1,1,1,1,1,1,1,1,1,1,1,1,1,1,1,1,1,1,1,1,1,1,1,
1,1,1,1,1,1,1,1,1,1,1,1,1,1,1,1,1,1,1,1,1,1,1,1,1,1,1,1,1,1,1,1,1,1,1,1,
1,1,1,1,1,1,1,1,1,1,1,1,1,1,1,1,1,1,1,1,1,1,1,1,1,1,1,1,1,1,1,1,1,1,1,1,
1,1,1,1,1,1,1,1,1,1,1,1,1,1,1,1,1,1,1,1,1,1,1,1,1,1,1,1,1,1,1,1,1,1,1,1,
1,1,1,1,1,1,1,1,1,1,1,1,1,1,1,1,1,1,1,1,1,1,1,1,1,1,1,1,1,1,1,1,1,1,1,1,
1,1,1,1,1,1,1,1,1,1,1,1,1,1,1,1,1,1,1,1,1,1,1,1,1,1,1,1,1,1,1,1,1,1,1,1,
1,1,1,1,1,1,1,1,1,1,1,1,1,1,1,1,1,1,1,1,1,1,1,1,1,1,1,1,1,1,1,1,1,1,1,1,
1,1,1,1,1,1,1,1,1,1,1,1,1,1,1,1,1,1,1,1,1,1,1,1,1,1,1,1,1,1,1,1,1,1,1,1,
1,1,1,1,1,1,1,1,1,1,1,1,1,1,1,1,1,1,1,1,1,1,1,1,1,1,1,1,1,1,1,1,1,1,1,1,
1,1,1,1,1,1,1,1,1,1,1,1,1,1,1,1,1,1,1,1,1,1,1,1,1,1,1,1,1,1,1,1,1,1,1,1,
1,1,1,1,1,1,1,1,1,1,1,1,1,1,1,1,1,1,1,1,1,1,1,1,1,1,1,1,1,1,1,1,1,1,1,1,
1,1,1,1,1,1,1,1,1,1,1,1,1,1,1,1,1,1,1,1,1,1,1,1,1,1,1,1,1,1,1,1,1,1,1,1,
1,1,1,1,1,1,1,1,1,1,1,1,1,1,1,1,1,1,1,1,1,1,1,1,1,1,1,1,1,1,1,1,1,1,1,1,
1,1,1,1,1,1,1,1,1,1,1,1,1,1,1,1,1,1,1,1,1,1,1,1,1,1,1,1,1,1,1,1,1,1,1,1,
1,1,4),(0.,0.115296848757168),(11.6154215191118,12.1151488743229,12.6148762295339,
13.614330939956,14.6137856503781,15.6132403608002,16.6126950712223,17.6121497816443,
18.6116044920664,19.6110592024885,20.6105139129106,21.6099686233327,22.6094233337548,
23.6088780441768,24.6083327545989,25.607787465021,26.6072421754431,27.6066968858652,
28.6061515962873,29.6056063067094,30.6050610171314,31.6045157275535,32.6039704379756,
33.6034251483977,34.6028798588198,35.6023345692419,36.601789279664,37.601243990086,
38.6006987005081,39.6001534109302,40.5996081213523,41.5990628317744,42.5985175421965,
43.5979722526185,44.5974269630406,45.5968816734627,46.5963363838848,47.5957910943069,
48.595245804729,49.5947005151511,50.5941552255731,51.5936099359952,52.5930646464173,
53.5925193568394,54.5919740672615,55.5914287776836,56.5908834881057,57.5903381985277,
58.5897929089498,59.5892476193719,60.588702329794,61.5881570402161,62.5876117506382,
63.5870664610603,64.5865211714823,65.5859758819044,66.5854305923265,67.5848853027486,
68.5843400131707,69.5837947235928,70.5832494340148,71.5827041444369,72.582158854859,
73.5816135652811,74.5810682757032,75.5805229861253,76.5799776965474,77.5794324069694,
78.5788871173915,79.5783418278136,80.5777965382357,81.5772512486578,82.5767059590799,
83.5761606695019,84.575615379924,85.5750700903461,86.5745248007682,87.5739795111903,
88.5734342216124,89.5728889320345,90.5723436424566,91.5717983528786,92.5712530633007,
93.5707077737228,94.5701624841449,95.569617194567,96.5690719049891,97.5685266154111,
98.5679813258332,99.5674360362553,100.566890746677,101.566345457099,102.565800167522,
103.565254877944,104.564709588366,105.564164298788,106.56361900921,107.563073719632,
108.562528430054,109.561983140476,110.561437850898,111.56089256132,112.560347271742,
113.559801982165,114.559256692587,115.558711403009,116.558166113431,117.557620823853,
118.557075534275,119.556530244697,120.555984955119,121.555439665541,122.554894375963,
123.554349086385,124.553803796807,125.55325850723,126.552713217652,127.552167928074,
128.551622638496,129.551077348918,130.55053205934,131.549986769762,132.549441480184,
133.548896190606,134.548350901028,135.54780561145,136.547260321872,137.546715032295,
138.546169742717,139.545624453139,140.545079163561,141.544533873983,142.543988584405,
143.543443294827,144.542898005249,145.542352715671,146.541807426093,147.541262136515,
148.540716846937,149.54017155736,150.539626267782,151.539080978204,152.538535688626,
153.537990399048,154.53744510947,155.536899819892,156.536354530314,157.535809240736,
158.535263951158,159.53471866158,160.534173372003,161.533628082425,162.533082792847,
163.532537503269,164.531992213691,165.531446924113,166.530901634535,167.530356344957,
168.529811055379,169.529265765801,170.528720476223,171.528175186645,172.527629897068,
173.52708460749,174.526539317912,175.525994028334,176.525448738756,177.524903449178,
178.5243581596,179.523812870022,180.523267580444,181.522722290866,182.522177001288,
183.52163171171,184.521086422133,185.520541132555,186.519995842977,187.519450553399,
188.518905263821,189.518359974243,190.517814684665,191.517269395087,192.516724105509,
193.516178815931,194.515633526353,195.515088236775,196.514542947198,197.51399765762,
198.513452368042,199.512907078464,200.512361788886,201.511816499308,202.51127120973,
203.510725920152,204.510180630574,205.509635340996,206.509090051418,207.508544761841,
208.507999472263,209.507454182685,210.506908893107,211.506363603529,212.505818313951,
213.505273024373,214.504727734795,215.504182445217,216.503637155639,217.503091866061,
218.502546576483,219.502001286906,220.501455997328,221.50091070775,222.500365418172,
223.499820128594,224.499274839016,225.498729549438,226.49818425986,227.497638970282,
228.497093680704,229.496548391126,230.496003101548,231.495457811971,232.494912522393,
233.494367232815,234.493821943237,235.493276653659,236.492731364081,237.492186074503,
238.491640784925,239.491095495347,240.490550205769,241.490004916191,242.489459626613,
243.488914337036,244.488369047458,245.48782375788,246.487278468302,247.486733178724,
248.486187889146,249.485642599568,250.48509730999,251.484552020412,252.484006730834,
253.483461441256,254.482916151679,255.482370862101,256.481825572523,257.481280282945,
258.480734993367,259.480189703789,260.479644414211,261.479099124633,262.478553835055,
263.478008545477,264.477463255899,265.476917966321,266.476372676744,267.475827387166,
268.475282097588,269.47473680801,270.474191518432,271.473646228854,272.473100939276,
273.472555649698,274.47201036012,275.471465070542,276.470919780964,277.470374491386,
278.469829201809,279.469283912231,280.468738622653,281.468193333075,282.467648043497,
283.467102753919,284.466557464341,285.466012174763,286.465466885185,287.464921595607,
288.464376306029,289.463831016451,290.463285726874,291.462740437296,292.462195147718,
293.46164985814,294.461104568562,295.460559278984,296.460013989406,297.459468699828,
298.45892341025,299.458378120672,300.457832831094,301.457287541517,302.456742251939,
303.456196962361,304.455651672783,305.455106383205,306.454561093627,307.454015804049,
308.453470514471,309.452925224893,310.452379935315,311.451834645737,312.451289356159,
313.450744066582,314.450198777004,315.449653487426,316.449108197848,317.44856290827,
318.448017618692,319.447472329114,320.446927039536,321.446381749958,322.44583646038,
323.445291170802,324.444745881224,325.444200591647,326.443655302069,327.443110012491,
328.442564722913,329.442019433335,330.441474143757,331.440928854179,332.440383564601,
333.439838275023,334.439292985445,335.438747695867,336.438202406289,337.437657116712,
338.437111827134,339.436566537556,340.436021247978,341.4354759584,342.434930668822,
343.434385379244,344.433840089666,345.433294800088,346.43274951051,347.432204220932,
348.431658931354,349.431113641777,350.430568352199,351.430023062621,352.429477773043,
353.428932483465,354.428387193887,355.427841904309,356.427296614731,357.426751325153,
358.426206035575,359.425660745997,360.42511545642,361.424570166842,362.424024877264,
363.423479587686,364.422934298108,365.42238900853,366.421843718952,367.421298429374,
368.420753139796,369.420207850218,370.41966256064,371.419117271062,372.418571981485,
373.418026691907,374.417481402329,375.416936112751,376.416390823173,377.415845533595,
378.415300244017,379.414754954439,380.414209664861,381.413664375283,382.413119085705,
383.412573796127,384.41202850655,385.411483216972,386.410937927394,387.410392637816,
388.409847348238,389.40930205866,390.408756769082,391.408211479504,392.407666189926,
393.407120900348,394.40657561077,395.406030321192,396.405485031615,397.404939742037,
398.404394452459,399.403849162881,400.403303873303,401.402758583725,402.402213294147,
403.401668004569,404.401122714991,405.400577425413,406.400032135835,407.399486846258,
408.39894155668,409.398396267102,410.397850977524,411.397305687946,412.396760398368,
413.39621510879,414.395669819212,415.395124529634,416.394579240056,417.394033950478,
418.3934886609,419.392943371323,420.392398081745,421.391852792167,422.391307502589,
423.390762213011,424.390216923433,425.389671633855,426.389126344277,427.388581054699,
428.388035765121,429.387490475543,430.386945185965,431.386399896388,432.38585460681,
433.385309317232,434.384764027654,435.384218738076,436.383673448498,437.38312815892,
438.382582869342,439.382037579764,440.381492290186,441.380947000608,442.380401711031,
443.379856421453,444.379311131875,445.378765842297,446.378220552719,447.377675263141,
448.377129973563,449.376584683985,450.376039394407,451.375494104829,452.374948815251,
453.374403525673,454.373858236095,455.373312946518,456.37276765694,457.372222367362,
458.371677077784,459.371131788206,460.370586498628,461.37004120905,462.369495919472,
463.368950629894,464.368405340316,465.367860050738,466.367314761161,467.366769471583,
468.366224182005,469.365678892427,470.365133602849,471.364588313271,472.364043023693,
473.363497734115,474.362952444537,475.362407154959,476.361861865381,477.361316575803,
478.360771286226,479.360225996648,480.35968070707,481.359135417492,482.358590127914,
483.358044838336,484.357499548758,485.35695425918,486.356408969602,487.355863680024,
488.355318390446,489.354773100868,490.354227811291,491.353682521713,492.353137232135,
493.352591942557,494.352046652979,495.351501363401,496.350956073823,497.350410784245,
498.349865494667,499.349320205089,500.348774915511,501.348229625934,502.347684336356,
503.347139046778,504.3465937572,505.346048467622,506.345503178044,507.344957888466,
508.344412598888,509.34386730931,510.343322019732,511.342776730154,512.342231440576,
513.341686150999,514.341140861421,515.340595571843,515.840322927054,516.340050282265),
 .UNSPECIFIED.);
#262=B_SPLINE_SURFACE_WITH_KNOTS('',3,3,((#58934,#58935,#58936,#58937,#58938,
#58939,#58940,#58941,#58942,#58943,#58944,#58945,#58946,#58947,#58948,#58949,
#58950,#58951,#58952,#58953,#58954,#58955,#58956,#58957,#58958,#58959,#58960,
#58961,#58962,#58963,#58964,#58965,#58966,#58967,#58968,#58969,#58970,#58971,
#58972,#58973,#58974,#58975,#58976,#58977,#58978,#58979,#58980,#58981,#58982,
#58983,#58984,#58985,#58986,#58987,#58988,#58989,#58990,#58991,#58992,#58993,
#58994,#58995,#58996,#58997,#58998,#58999,#59000,#59001,#59002,#59003,#59004,
#59005,#59006,#59007,#59008,#59009,#59010,#59011,#59012,#59013,#59014,#59015,
#59016,#59017,#59018,#59019,#59020,#59021,#59022,#59023,#59024,#59025,#59026,
#59027,#59028,#59029,#59030,#59031,#59032,#59033,#59034,#59035,#59036,#59037,
#59038,#59039,#59040,#59041,#59042,#59043,#59044,#59045,#59046,#59047,#59048,
#59049,#59050,#59051,#59052),(#59053,#59054,#59055,#59056,#59057,#59058,
#59059,#59060,#59061,#59062,#59063,#59064,#59065,#59066,#59067,#59068,#59069,
#59070,#59071,#59072,#59073,#59074,#59075,#59076,#59077,#59078,#59079,#59080,
#59081,#59082,#59083,#59084,#59085,#59086,#59087,#59088,#59089,#59090,#59091,
#59092,#59093,#59094,#59095,#59096,#59097,#59098,#59099,#59100,#59101,#59102,
#59103,#59104,#59105,#59106,#59107,#59108,#59109,#59110,#59111,#59112,#59113,
#59114,#59115,#59116,#59117,#59118,#59119,#59120,#59121,#59122,#59123,#59124,
#59125,#59126,#59127,#59128,#59129,#59130,#59131,#59132,#59133,#59134,#59135,
#59136,#59137,#59138,#59139,#59140,#59141,#59142,#59143,#59144,#59145,#59146,
#59147,#59148,#59149,#59150,#59151,#59152,#59153,#59154,#59155,#59156,#59157,
#59158,#59159,#59160,#59161,#59162,#59163,#59164,#59165,#59166,#59167,#59168,
#59169,#59170,#59171),(#59172,#59173,#59174,#59175,#59176,#59177,#59178,
#59179,#59180,#59181,#59182,#59183,#59184,#59185,#59186,#59187,#59188,#59189,
#59190,#59191,#59192,#59193,#59194,#59195,#59196,#59197,#59198,#59199,#59200,
#59201,#59202,#59203,#59204,#59205,#59206,#59207,#59208,#59209,#59210,#59211,
#59212,#59213,#59214,#59215,#59216,#59217,#59218,#59219,#59220,#59221,#59222,
#59223,#59224,#59225,#59226,#59227,#59228,#59229,#59230,#59231,#59232,#59233,
#59234,#59235,#59236,#59237,#59238,#59239,#59240,#59241,#59242,#59243,#59244,
#59245,#59246,#59247,#59248,#59249,#59250,#59251,#59252,#59253,#59254,#59255,
#59256,#59257,#59258,#59259,#59260,#59261,#59262,#59263,#59264,#59265,#59266,
#59267,#59268,#59269,#59270,#59271,#59272,#59273,#59274,#59275,#59276,#59277,
#59278,#59279,#59280,#59281,#59282,#59283,#59284,#59285,#59286,#59287,#59288,
#59289,#59290),(#59291,#59292,#59293,#59294,#59295,#59296,#59297,#59298,
#59299,#59300,#59301,#59302,#59303,#59304,#59305,#59306,#59307,#59308,#59309,
#59310,#59311,#59312,#59313,#59314,#59315,#59316,#59317,#59318,#59319,#59320,
#59321,#59322,#59323,#59324,#59325,#59326,#59327,#59328,#59329,#59330,#59331,
#59332,#59333,#59334,#59335,#59336,#59337,#59338,#59339,#59340,#59341,#59342,
#59343,#59344,#59345,#59346,#59347,#59348,#59349,#59350,#59351,#59352,#59353,
#59354,#59355,#59356,#59357,#59358,#59359,#59360,#59361,#59362,#59363,#59364,
#59365,#59366,#59367,#59368,#59369,#59370,#59371,#59372,#59373,#59374,#59375,
#59376,#59377,#59378,#59379,#59380,#59381,#59382,#59383,#59384,#59385,#59386,
#59387,#59388,#59389,#59390,#59391,#59392,#59393,#59394,#59395,#59396,#59397,
#59398,#59399,#59400,#59401,#59402,#59403,#59404,#59405,#59406,#59407,#59408,
#59409)),.UNSPECIFIED.,.F.,.F.,.F.,(4,4),(4,1,1,1,1,1,1,1,1,1,1,1,1,1,1,
1,1,1,1,1,1,1,1,1,1,1,1,1,1,1,1,1,1,1,1,1,1,1,1,1,1,1,1,1,1,1,1,1,1,1,1,
1,1,1,1,1,1,1,1,1,1,1,1,1,1,1,1,1,1,1,1,1,1,1,1,1,1,1,1,1,1,1,1,1,1,1,1,
1,1,1,1,1,1,1,1,1,1,1,1,1,1,1,1,1,1,1,1,1,1,1,1,1,1,1,1,1,4),(0.,0.0658467982010768),
(8.30747755240098,9.30028767054014,10.2930977886793,11.2859079068184,12.2787180249576,
13.2715281430967,14.2643382612359,15.2571483793751,16.2499584975142,17.2427686156534,
18.2355787337925,19.2283888519317,20.2211989700708,21.21400908821,22.2068192063491,
23.1996293244883,24.1924394426274,25.1852495607666,26.1780596789057,27.1708697970449,
28.163679915184,29.1564900333232,30.1493001514623,31.1421102696015,32.1349203877406,
33.1277305058798,34.120540624019,35.1133507421581,36.1061608602973,37.0989709784364,
38.0917810965756,39.0845912147147,40.0774013328539,41.070211450993,42.0630215691322,
43.0558316872713,44.0486418054105,45.0414519235496,46.0342620416888,47.0270721598279,
48.0198822779671,49.0126923961063,50.0055025142454,50.9983126323846,51.9911227505237,
52.9839328686629,53.976742986802,54.9695531049412,55.9623632230803,56.9551733412195,
57.9479834593586,58.9407935774978,59.9336036956369,60.9264138137761,61.9192239319152,
62.9120340500544,63.9048441681935,64.8976542863327,65.8904644044719,66.883274522611,
67.8760846407502,68.8688947588893,69.8617048770285,70.8545149951676,71.8473251133068,
72.8401352314459,73.8329453495851,74.8257554677242,75.8185655858634,76.8113757040025,
77.8041858221417,78.7969959402808,79.78980605842,80.7826161765591,81.7754262946983,
82.7682364128375,83.7610465309766,84.7538566491157,85.7466667672549,86.7394768853941,
87.7322870035332,88.7250971216724,89.7179072398115,90.7107173579507,91.7035274760898,
92.696337594229,93.6891477123681,94.6819578305073,95.6747679486464,96.6675780667856,
97.6603881849247,98.6531983030639,99.646008421203,100.638818539342,101.631628657481,
102.624438775621,103.61724889376,104.610059011899,105.602869130038,106.595679248177,
107.588489366316,108.581299484455,109.574109602595,110.566919720734,111.559729838873,
112.552539957012,113.545350075151,114.53816019329,115.530970311429,116.523780429569,
117.516590547708,118.509400665847,119.502210783986,120.495020902125,121.487831020264,
122.480641138404,123.473451256543),.UNSPECIFIED.);
#263=B_SPLINE_SURFACE_WITH_KNOTS('',3,3,((#59633,#59634,#59635,#59636,#59637,
#59638,#59639,#59640,#59641,#59642,#59643,#59644,#59645,#59646,#59647,#59648,
#59649,#59650,#59651,#59652,#59653,#59654,#59655,#59656,#59657,#59658,#59659,
#59660,#59661,#59662,#59663,#59664,#59665,#59666,#59667,#59668,#59669,#59670,
#59671,#59672,#59673,#59674,#59675,#59676,#59677,#59678,#59679,#59680,#59681,
#59682,#59683,#59684,#59685,#59686,#59687,#59688,#59689,#59690,#59691,#59692,
#59693,#59694,#59695,#59696,#59697,#59698,#59699,#59700,#59701,#59702,#59703,
#59704,#59705,#59706,#59707,#59708,#59709,#59710,#59711,#59712,#59713,#59714,
#59715,#59716,#59717,#59718,#59719,#59720,#59721,#59722,#59723,#59724,#59725,
#59726,#59727,#59728,#59729,#59730,#59731,#59732,#59733,#59734,#59735,#59736,
#59737,#59738,#59739,#59740,#59741,#59742,#59743,#59744,#59745,#59746,#59747,
#59748,#59749,#59750,#59751),(#59752,#59753,#59754,#59755,#59756,#59757,
#59758,#59759,#59760,#59761,#59762,#59763,#59764,#59765,#59766,#59767,#59768,
#59769,#59770,#59771,#59772,#59773,#59774,#59775,#59776,#59777,#59778,#59779,
#59780,#59781,#59782,#59783,#59784,#59785,#59786,#59787,#59788,#59789,#59790,
#59791,#59792,#59793,#59794,#59795,#59796,#59797,#59798,#59799,#59800,#59801,
#59802,#59803,#59804,#59805,#59806,#59807,#59808,#59809,#59810,#59811,#59812,
#59813,#59814,#59815,#59816,#59817,#59818,#59819,#59820,#59821,#59822,#59823,
#59824,#59825,#59826,#59827,#59828,#59829,#59830,#59831,#59832,#59833,#59834,
#59835,#59836,#59837,#59838,#59839,#59840,#59841,#59842,#59843,#59844,#59845,
#59846,#59847,#59848,#59849,#59850,#59851,#59852,#59853,#59854,#59855,#59856,
#59857,#59858,#59859,#59860,#59861,#59862,#59863,#59864,#59865,#59866,#59867,
#59868,#59869,#59870),(#59871,#59872,#59873,#59874,#59875,#59876,#59877,
#59878,#59879,#59880,#59881,#59882,#59883,#59884,#59885,#59886,#59887,#59888,
#59889,#59890,#59891,#59892,#59893,#59894,#59895,#59896,#59897,#59898,#59899,
#59900,#59901,#59902,#59903,#59904,#59905,#59906,#59907,#59908,#59909,#59910,
#59911,#59912,#59913,#59914,#59915,#59916,#59917,#59918,#59919,#59920,#59921,
#59922,#59923,#59924,#59925,#59926,#59927,#59928,#59929,#59930,#59931,#59932,
#59933,#59934,#59935,#59936,#59937,#59938,#59939,#59940,#59941,#59942,#59943,
#59944,#59945,#59946,#59947,#59948,#59949,#59950,#59951,#59952,#59953,#59954,
#59955,#59956,#59957,#59958,#59959,#59960,#59961,#59962,#59963,#59964,#59965,
#59966,#59967,#59968,#59969,#59970,#59971,#59972,#59973,#59974,#59975,#59976,
#59977,#59978,#59979,#59980,#59981,#59982,#59983,#59984,#59985,#59986,#59987,
#59988,#59989),(#59990,#59991,#59992,#59993,#59994,#59995,#59996,#59997,
#59998,#59999,#60000,#60001,#60002,#60003,#60004,#60005,#60006,#60007,#60008,
#60009,#60010,#60011,#60012,#60013,#60014,#60015,#60016,#60017,#60018,#60019,
#60020,#60021,#60022,#60023,#60024,#60025,#60026,#60027,#60028,#60029,#60030,
#60031,#60032,#60033,#60034,#60035,#60036,#60037,#60038,#60039,#60040,#60041,
#60042,#60043,#60044,#60045,#60046,#60047,#60048,#60049,#60050,#60051,#60052,
#60053,#60054,#60055,#60056,#60057,#60058,#60059,#60060,#60061,#60062,#60063,
#60064,#60065,#60066,#60067,#60068,#60069,#60070,#60071,#60072,#60073,#60074,
#60075,#60076,#60077,#60078,#60079,#60080,#60081,#60082,#60083,#60084,#60085,
#60086,#60087,#60088,#60089,#60090,#60091,#60092,#60093,#60094,#60095,#60096,
#60097,#60098,#60099,#60100,#60101,#60102,#60103,#60104,#60105,#60106,#60107,
#60108)),.UNSPECIFIED.,.F.,.F.,.F.,(4,4),(4,1,1,1,1,1,1,1,1,1,1,1,1,1,1,
1,1,1,1,1,1,1,1,1,1,1,1,1,1,1,1,1,1,1,1,1,1,1,1,1,1,1,1,1,1,1,1,1,1,1,1,
1,1,1,1,1,1,1,1,1,1,1,1,1,1,1,1,1,1,1,1,1,1,1,1,1,1,1,1,1,1,1,1,1,1,1,1,
1,1,1,1,1,1,1,1,1,1,1,1,1,1,1,1,1,1,1,1,1,1,1,1,1,1,1,1,1,4),(0.,0.0658467982010768),
(11.6150328478182,12.6078429659573,13.6006530840965,14.5934632022356,15.5862733203748,
16.5790834385139,17.5718935566531,18.5647036747922,19.5575137929314,20.5503239110706,
21.5431340292097,22.5359441473489,23.528754265488,24.5215643836272,25.5143745017663,
26.5071846199055,27.4999947380446,28.4928048561838,29.4856149743229,30.4784250924621,
31.4712352106012,32.4640453287404,33.4568554468795,34.4496655650187,35.4424756831578,
36.435285801297,37.4280959194362,38.4209060375753,39.4137161557145,40.4065262738536,
41.3993363919928,42.3921465101319,43.3849566282711,44.3777667464102,45.3705768645494,
46.3633869826885,47.3561971008277,48.3490072189668,49.341817337106,50.3346274552451,
51.3274375733843,52.3202476915234,53.3130578096626,54.3058679278017,55.2986780459409,
56.2914881640801,57.2842982822192,58.2771084003584,59.2699185184975,60.2627286366367,
61.2555387547758,62.248348872915,63.2411589910541,64.2339691091933,65.2267792273324,
66.2195893454716,67.2123994636107,68.2052095817499,69.198019699889,70.1908298180282,
71.1836399361674,72.1764500543065,73.1692601724456,74.1620702905848,75.154880408724,
76.1476905268631,77.1405006450023,78.1333107631414,79.1261208812806,80.1189309994197,
81.1117411175589,82.104551235698,83.0973613538372,84.0901714719763,85.0829815901155,
86.0757917082546,87.0686018263938,88.0614119445329,89.0542220626721,90.0470321808113,
91.0398422989504,92.0326524170896,93.0254625352287,94.0182726533679,95.011082771507,
96.0038928896462,96.9967030077853,97.9895131259245,98.9823232440636,99.9751333622028,
100.967943480342,101.960753598481,102.95356371662,103.946373834759,104.939183952899,
105.931994071038,106.924804189177,107.917614307316,108.910424425455,109.903234543594,
110.896044661733,111.888854779873,112.881664898012,113.874475016151,114.86728513429,
115.860095252429,116.852905370568,117.845715488708,118.838525606847,119.831335724986,
120.824145843125,121.816955961264,122.809766079403,123.802576197542,124.795386315682,
125.788196433821,126.78100655196),.UNSPECIFIED.);
#264=B_SPLINE_SURFACE_WITH_KNOTS('',3,3,((#62683,#62684,#62685,#62686,#62687,
#62688,#62689,#62690,#62691,#62692,#62693,#62694,#62695,#62696,#62697,#62698,
#62699,#62700,#62701,#62702,#62703,#62704,#62705,#62706,#62707,#62708,#62709,
#62710,#62711,#62712,#62713,#62714,#62715,#62716,#62717,#62718,#62719,#62720,
#62721,#62722,#62723,#62724,#62725,#62726,#62727,#62728,#62729,#62730,#62731,
#62732,#62733,#62734,#62735,#62736,#62737,#62738,#62739,#62740,#62741,#62742,
#62743,#62744,#62745,#62746,#62747,#62748,#62749,#62750,#62751,#62752,#62753,
#62754,#62755,#62756,#62757,#62758,#62759,#62760,#62761,#62762,#62763,#62764,
#62765,#62766,#62767,#62768,#62769,#62770,#62771,#62772,#62773,#62774,#62775,
#62776,#62777,#62778,#62779,#62780,#62781,#62782,#62783,#62784,#62785,#62786,
#62787,#62788),(#62789,#62790,#62791,#62792,#62793,#62794,#62795,#62796,
#62797,#62798,#62799,#62800,#62801,#62802,#62803,#62804,#62805,#62806,#62807,
#62808,#62809,#62810,#62811,#62812,#62813,#62814,#62815,#62816,#62817,#62818,
#62819,#62820,#62821,#62822,#62823,#62824,#62825,#62826,#62827,#62828,#62829,
#62830,#62831,#62832,#62833,#62834,#62835,#62836,#62837,#62838,#62839,#62840,
#62841,#62842,#62843,#62844,#62845,#62846,#62847,#62848,#62849,#62850,#62851,
#62852,#62853,#62854,#62855,#62856,#62857,#62858,#62859,#62860,#62861,#62862,
#62863,#62864,#62865,#62866,#62867,#62868,#62869,#62870,#62871,#62872,#62873,
#62874,#62875,#62876,#62877,#62878,#62879,#62880,#62881,#62882,#62883,#62884,
#62885,#62886,#62887,#62888,#62889,#62890,#62891,#62892,#62893,#62894),
(#62895,#62896,#62897,#62898,#62899,#62900,#62901,#62902,#62903,#62904,
#62905,#62906,#62907,#62908,#62909,#62910,#62911,#62912,#62913,#62914,#62915,
#62916,#62917,#62918,#62919,#62920,#62921,#62922,#62923,#62924,#62925,#62926,
#62927,#62928,#62929,#62930,#62931,#62932,#62933,#62934,#62935,#62936,#62937,
#62938,#62939,#62940,#62941,#62942,#62943,#62944,#62945,#62946,#62947,#62948,
#62949,#62950,#62951,#62952,#62953,#62954,#62955,#62956,#62957,#62958,#62959,
#62960,#62961,#62962,#62963,#62964,#62965,#62966,#62967,#62968,#62969,#62970,
#62971,#62972,#62973,#62974,#62975,#62976,#62977,#62978,#62979,#62980,#62981,
#62982,#62983,#62984,#62985,#62986,#62987,#62988,#62989,#62990,#62991,#62992,
#62993,#62994,#62995,#62996,#62997,#62998,#62999,#63000),(#63001,#63002,
#63003,#63004,#63005,#63006,#63007,#63008,#63009,#63010,#63011,#63012,#63013,
#63014,#63015,#63016,#63017,#63018,#63019,#63020,#63021,#63022,#63023,#63024,
#63025,#63026,#63027,#63028,#63029,#63030,#63031,#63032,#63033,#63034,#63035,
#63036,#63037,#63038,#63039,#63040,#63041,#63042,#63043,#63044,#63045,#63046,
#63047,#63048,#63049,#63050,#63051,#63052,#63053,#63054,#63055,#63056,#63057,
#63058,#63059,#63060,#63061,#63062,#63063,#63064,#63065,#63066,#63067,#63068,
#63069,#63070,#63071,#63072,#63073,#63074,#63075,#63076,#63077,#63078,#63079,
#63080,#63081,#63082,#63083,#63084,#63085,#63086,#63087,#63088,#63089,#63090,
#63091,#63092,#63093,#63094,#63095,#63096,#63097,#63098,#63099,#63100,#63101,
#63102,#63103,#63104,#63105,#63106)),.UNSPECIFIED.,.F.,.F.,.F.,(4,4),(4,
1,1,1,1,1,1,1,1,1,1,1,1,1,1,1,1,1,1,1,1,1,1,1,1,1,1,1,1,1,1,1,1,1,1,1,1,
1,1,1,1,1,1,1,1,1,1,1,1,1,1,1,1,1,1,1,1,1,1,1,1,1,1,1,1,1,1,1,1,1,1,1,1,
1,1,1,1,1,1,1,1,1,1,1,1,1,1,1,1,1,1,1,1,1,1,1,1,1,1,1,1,1,1,4),(0.,0.0460148164544132),
(11.6154215191105,12.6127573616628,13.610093204215,14.6074290467673,15.6047648893195,
16.6021007318718,17.599436574424,18.5967724169762,19.5941082595285,20.5914441020807,
21.588779944633,22.5861157871852,23.5834516297375,24.5807874722897,25.5781233148419,
26.5754591573942,27.5727949999464,28.5701308424987,29.5674666850509,30.5648025276032,
31.5621383701554,32.5594742127077,33.5568100552599,34.5541458978121,35.5514817403644,
36.5488175829166,37.5461534254689,38.5434892680211,39.5408251105734,40.5381609531256,
41.5354967956779,42.5328326382301,43.5301684807823,44.5275043233346,45.5248401658868,
46.5221760084391,47.5195118509913,48.5168476935436,49.5141835360958,50.5115193786481,
51.5088552212003,52.5061910637525,53.5035269063048,54.500862748857,55.4981985914093,
56.4955344339615,57.4928702765138,58.490206119066,59.4875419616182,60.4848778041705,
61.4822136467227,62.479549489275,63.4768853318272,64.4742211743795,65.4715570169317,
66.468892859484,67.4662287020362,68.4635645445884,69.4609003871407,70.4582362296929,
71.4555720722452,72.4529079147974,73.4502437573497,74.4475795999019,75.4449154424541,
76.4422512850064,77.4395871275586,78.4369229701109,79.4342588126631,80.4315946552154,
81.4289304977676,82.4262663403199,83.4236021828721,84.4209380254243,85.4182738679766,
86.4156097105288,87.4129455530811,88.4102813956333,89.4076172381856,90.4049530807378,
91.4022889232901,92.3996247658423,93.3969606083945,94.3942964509468,95.391632293499,
96.3889681360513,97.3863039786035,98.3836398211558,99.380975663708,100.37831150626,
101.375647348812,102.372983191365,103.370319033917,104.367654876469,105.364990719021,
106.362326561574,107.359662404126,108.356998246678,109.35433408923,110.351669931783,
111.349005774335,112.346341616887,113.343677459439,114.341013301992),
 .UNSPECIFIED.);
#265=B_SPLINE_SURFACE_WITH_KNOTS('',3,3,((#63226,#63227,#63228,#63229,#63230,
#63231,#63232,#63233,#63234,#63235,#63236,#63237,#63238,#63239,#63240,#63241,
#63242,#63243,#63244,#63245,#63246,#63247,#63248,#63249,#63250,#63251,#63252,
#63253,#63254,#63255,#63256,#63257,#63258,#63259,#63260,#63261,#63262,#63263,
#63264,#63265,#63266,#63267,#63268,#63269,#63270,#63271,#63272,#63273,#63274,
#63275,#63276,#63277,#63278,#63279,#63280,#63281,#63282,#63283,#63284,#63285,
#63286,#63287,#63288,#63289,#63290,#63291,#63292,#63293,#63294,#63295,#63296,
#63297,#63298,#63299,#63300,#63301,#63302,#63303,#63304,#63305,#63306,#63307,
#63308,#63309,#63310,#63311,#63312,#63313,#63314,#63315,#63316,#63317,#63318,
#63319,#63320,#63321,#63322,#63323,#63324,#63325,#63326,#63327,#63328,#63329,
#63330,#63331,#63332,#63333),(#63334,#63335,#63336,#63337,#63338,#63339,
#63340,#63341,#63342,#63343,#63344,#63345,#63346,#63347,#63348,#63349,#63350,
#63351,#63352,#63353,#63354,#63355,#63356,#63357,#63358,#63359,#63360,#63361,
#63362,#63363,#63364,#63365,#63366,#63367,#63368,#63369,#63370,#63371,#63372,
#63373,#63374,#63375,#63376,#63377,#63378,#63379,#63380,#63381,#63382,#63383,
#63384,#63385,#63386,#63387,#63388,#63389,#63390,#63391,#63392,#63393,#63394,
#63395,#63396,#63397,#63398,#63399,#63400,#63401,#63402,#63403,#63404,#63405,
#63406,#63407,#63408,#63409,#63410,#63411,#63412,#63413,#63414,#63415,#63416,
#63417,#63418,#63419,#63420,#63421,#63422,#63423,#63424,#63425,#63426,#63427,
#63428,#63429,#63430,#63431,#63432,#63433,#63434,#63435,#63436,#63437,#63438,
#63439,#63440,#63441),(#63442,#63443,#63444,#63445,#63446,#63447,#63448,
#63449,#63450,#63451,#63452,#63453,#63454,#63455,#63456,#63457,#63458,#63459,
#63460,#63461,#63462,#63463,#63464,#63465,#63466,#63467,#63468,#63469,#63470,
#63471,#63472,#63473,#63474,#63475,#63476,#63477,#63478,#63479,#63480,#63481,
#63482,#63483,#63484,#63485,#63486,#63487,#63488,#63489,#63490,#63491,#63492,
#63493,#63494,#63495,#63496,#63497,#63498,#63499,#63500,#63501,#63502,#63503,
#63504,#63505,#63506,#63507,#63508,#63509,#63510,#63511,#63512,#63513,#63514,
#63515,#63516,#63517,#63518,#63519,#63520,#63521,#63522,#63523,#63524,#63525,
#63526,#63527,#63528,#63529,#63530,#63531,#63532,#63533,#63534,#63535,#63536,
#63537,#63538,#63539,#63540,#63541,#63542,#63543,#63544,#63545,#63546,#63547,
#63548,#63549),(#63550,#63551,#63552,#63553,#63554,#63555,#63556,#63557,
#63558,#63559,#63560,#63561,#63562,#63563,#63564,#63565,#63566,#63567,#63568,
#63569,#63570,#63571,#63572,#63573,#63574,#63575,#63576,#63577,#63578,#63579,
#63580,#63581,#63582,#63583,#63584,#63585,#63586,#63587,#63588,#63589,#63590,
#63591,#63592,#63593,#63594,#63595,#63596,#63597,#63598,#63599,#63600,#63601,
#63602,#63603,#63604,#63605,#63606,#63607,#63608,#63609,#63610,#63611,#63612,
#63613,#63614,#63615,#63616,#63617,#63618,#63619,#63620,#63621,#63622,#63623,
#63624,#63625,#63626,#63627,#63628,#63629,#63630,#63631,#63632,#63633,#63634,
#63635,#63636,#63637,#63638,#63639,#63640,#63641,#63642,#63643,#63644,#63645,
#63646,#63647,#63648,#63649,#63650,#63651,#63652,#63653,#63654,#63655,#63656,
#63657)),.UNSPECIFIED.,.F.,.F.,.F.,(4,4),(4,1,1,1,1,1,1,1,1,1,1,1,1,1,1,
1,1,1,1,1,1,1,1,1,1,1,1,1,1,1,1,1,1,1,1,1,1,1,1,1,1,1,1,1,1,1,1,1,1,1,1,
1,1,1,1,1,1,1,1,1,1,1,1,1,1,1,1,1,1,1,1,1,1,1,1,1,1,1,1,1,1,1,1,1,1,1,1,
1,1,1,1,1,1,1,1,1,1,1,1,1,1,1,1,1,1,4),(0.,0.0460148164544132),(8.31058692273969,
9.30859389336977,10.3066008639999,11.30460783463,12.30261480526,13.3006217758901,
14.2986287465202,15.2966357171503,16.2946426877804,17.2926496584105,18.2906566290406,
19.2886635996707,20.2866705703008,21.2846775409308,22.2826845115609,23.280691482191,
24.2786984528211,25.2767054234512,26.2747123940813,27.2727193647114,28.2707263353415,
29.2687333059716,30.2667402766016,31.2647472472317,32.2627542178618,33.2607611884919,
34.258768159122,35.2567751297521,36.2547821003822,37.2527890710123,38.2507960416424,
39.2488030122724,40.2468099829025,41.2448169535326,42.2428239241627,43.2408308947928,
44.2388378654229,45.236844836053,46.2348518066831,47.2328587773132,48.2308657479432,
49.2288727185733,50.2268796892034,51.2248866598335,52.2228936304636,53.2209006010937,
54.2189075717238,55.2169145423539,56.214921512984,57.212928483614,58.2109354542441,
59.2089424248742,60.2069493955043,61.2049563661344,62.2029633367645,63.2009703073946,
64.1989772780247,65.1969842486548,66.1949912192848,67.1929981899149,68.191005160545,
69.1890121311751,70.1870191018052,71.1850260724353,72.1830330430654,73.1810400136955,
74.1790469843256,75.1770539549557,76.1750609255857,77.1730678962158,78.1710748668459,
79.169081837476,80.1670888081061,81.1650957787362,82.1631027493663,83.1611097199964,
84.1591166906264,85.1571236612565,86.1551306318866,87.1531376025167,88.1511445731468,
89.1491515437769,90.147158514407,91.1451654850371,92.1431724556672,93.1411794262973,
94.1391863969273,95.1371933675574,96.1352003381875,97.1332073088176,98.1312142794477,
99.1292212500778,100.127228220708,101.125235191338,102.123242161968,103.121249132598,
104.119256103228,105.117263073858,106.115270044488,107.113277015118,108.111283985749,
109.109290956379,110.107297927009,111.105304897639,112.103311868269,113.101318838899),
 .UNSPECIFIED.);
#266=B_SPLINE_CURVE_WITH_KNOTS('',3,(#20089,#20090,#20091,#20092,#20093,
#20094,#20095,#20096,#20097,#20098,#20099,#20100,#20101),.UNSPECIFIED.,
 .F.,.F.,(4,3,3,3,4),(-43.0846992492315,-42.6573287234279,-42.1670146001701,
-41.6767004769123,-41.5553414461756),.UNSPECIFIED.);
#267=B_SPLINE_CURVE_WITH_KNOTS('',3,(#20107,#20108,#20109,#20110,#20111,
#20112,#20113,#20114,#20115,#20116,#20117,#20118,#20119,#20120,#20121,#20122,
#20123,#20124,#20125,#20126,#20127,#20128,#20129,#20130,#20131,#20132,#20133,
#20134,#20135,#20136,#20137,#20138,#20139,#20140,#20141,#20142,#20143,#20144,
#20145,#20146),.UNSPECIFIED.,.F.,.F.,(4,3,3,3,3,3,3,3,3,3,3,3,3,4),(39.0086749840546,
39.2251298606233,39.7154439838811,40.2057581071389,40.6960722303967,41.1863863536545,
41.6767004769123,42.1670146001701,42.6573287234279,43.1476428466857,43.6379569699435,
44.1282710932012,44.618585216459,45.1088993397168),.UNSPECIFIED.);
#268=B_SPLINE_CURVE_WITH_KNOTS('',3,(#20148,#20149,#20150,#20151,#20152,
#20153,#20154,#20155,#20156,#20157,#20158,#20159,#20160,#20161,#20162,#20163,
#20164,#20165,#20166,#20167,#20168,#20169,#20170,#20171,#20172,#20173,#20174,
#20175,#20176,#20177,#20178,#20179,#20180,#20181,#20182,#20183,#20184,#20185,
#20186,#20187,#20188,#20189,#20190),.UNSPECIFIED.,.F.,.F.,(4,3,3,3,3,3,
3,3,3,3,3,3,3,3,4),(-41.5553414461756,-41.1863863536545,-40.6960722303967,
-40.2057581071389,-39.7154439838811,-39.2251298606233,-38.7348157373656,
-38.2445016141078,-37.75418749085,-37.2638733675922,-36.7735592443344,-36.2832451210766,
-35.7929309978188,-35.302616874561,-35.272156138996),.UNSPECIFIED.);
#269=B_SPLINE_CURVE_WITH_KNOTS('',3,(#20195,#20196,#20197,#20198,#20199,
#20200,#20201,#20202,#20203,#20204,#20205,#20206,#20207,#20208,#20209,#20210,
#20211,#20212,#20213,#20214,#20215,#20216,#20217,#20218,#20219,#20220,#20221,
#20222,#20223,#20224,#20225,#20226,#20227,#20228,#20229,#20230,#20231,#20232,
#20233,#20234,#20235,#20236,#20237),.UNSPECIFIED.,.F.,.F.,(4,3,3,3,3,3,
3,3,3,3,3,3,3,3,4),(32.725489676875,32.851046258272,33.3413603815298,33.8316745047876,
34.3219886280454,34.8123027513032,35.302616874561,35.7929309978188,36.2832451210766,
36.7735592443344,37.2638733675922,37.75418749085,38.2445016141078,38.7348157373655,
39.0086749840546),.UNSPECIFIED.);
#270=B_SPLINE_CURVE_WITH_KNOTS('',3,(#20238,#20239,#20240,#20241,#20242,
#20243,#20244,#20245,#20246,#20247,#20248,#20249,#20250,#20251,#20252,#20253,
#20254,#20255,#20256,#20257,#20258,#20259,#20260,#20261,#20262,#20263,#20264,
#20265,#20266,#20267,#20268,#20269,#20270,#20271,#20272,#20273,#20274,#20275,
#20276,#20277),.UNSPECIFIED.,.F.,.F.,(4,3,3,3,3,3,3,3,3,3,3,3,3,4),(-35.272156138996,
-34.8123027513032,-34.3219886280454,-33.8316745047876,-33.3413603815298,
-32.851046258272,-32.3607321350143,-31.8704180117565,-31.3801038884987,
-30.8897897652409,-30.3994756419831,-29.9091615187253,-29.4188473954675,
-28.9889708318164),.UNSPECIFIED.);
#271=B_SPLINE_CURVE_WITH_KNOTS('',3,(#20282,#20283,#20284,#20285,#20286,
#20287,#20288,#20289,#20290,#20291,#20292,#20293,#20294,#20295,#20296,#20297,
#20298,#20299,#20300,#20301,#20302,#20303,#20304,#20305,#20306,#20307,#20308,
#20309,#20310,#20311,#20312,#20313,#20314,#20315,#20316,#20317,#20318,#20319,
#20320,#20321,#20322,#20323,#20324),.UNSPECIFIED.,.F.,.F.,(4,3,3,3,3,3,
3,3,3,3,3,3,3,3,4),(26.4423043696954,26.4769626559207,26.9672767791785,
27.4575909024363,27.9479050256941,28.4382191489519,28.9285332722097,29.4188473954675,
29.9091615187253,30.3994756419831,30.8897897652409,31.3801038884987,31.8704180117565,
32.3607321350143,32.725489676875),.UNSPECIFIED.);
#272=B_SPLINE_CURVE_WITH_KNOTS('',3,(#20325,#20326,#20327,#20328,#20329,
#20330,#20331,#20332,#20333,#20334,#20335,#20336,#20337,#20338,#20339,#20340,
#20341,#20342,#20343,#20344,#20345,#20346,#20347,#20348,#20349,#20350,#20351,
#20352,#20353,#20354,#20355,#20356,#20357,#20358,#20359,#20360,#20361,#20362,
#20363,#20364,#20365,#20366,#20367),.UNSPECIFIED.,.F.,.F.,(4,3,3,3,3,3,
3,3,3,3,3,3,3,3,4),(-28.9889708318164,-28.9285332722097,-28.4382191489519,
-27.9479050256941,-27.4575909024363,-26.9672767791785,-26.4769626559208,
-25.986648532663,-25.4963344094052,-25.0060202861474,-24.5157061628896,
-24.0253920396318,-23.535077916374,-23.0447637931162,-22.7057855246369),
 .UNSPECIFIED.);
#273=B_SPLINE_CURVE_WITH_KNOTS('',3,(#20372,#20373,#20374,#20375,#20376,
#20377,#20378,#20379,#20380,#20381,#20382,#20383,#20384,#20385,#20386,#20387,
#20388,#20389,#20390,#20391,#20392,#20393,#20394,#20395,#20396,#20397,#20398,
#20399,#20400,#20401,#20402,#20403,#20404,#20405,#20406,#20407,#20408,#20409,
#20410,#20411),.UNSPECIFIED.,.F.,.F.,(4,3,3,3,3,3,3,3,3,3,3,3,3,4),(20.1591190625159,
20.5931931768272,21.083507300085,21.5738214233428,22.0641355466006,22.5544496698584,
23.0447637931162,23.535077916374,24.0253920396318,24.5157061628896,25.0060202861474,
25.4963344094052,25.986648532663,26.4423043696954),.UNSPECIFIED.);
#274=B_SPLINE_CURVE_WITH_KNOTS('',3,(#20412,#20413,#20414,#20415,#20416,
#20417,#20418,#20419,#20420,#20421,#20422,#20423,#20424,#20425,#20426,#20427,
#20428,#20429,#20430,#20431,#20432,#20433,#20434,#20435,#20436,#20437,#20438,
#20439,#20440,#20441,#20442,#20443,#20444,#20445,#20446,#20447,#20448,#20449,
#20450,#20451,#20452,#20453,#20454),.UNSPECIFIED.,.F.,.F.,(4,3,3,3,3,3,
3,3,3,3,3,3,3,3,4),(-22.7057855246369,-22.5544496698584,-22.0641355466006,
-21.5738214233428,-21.083507300085,-20.5931931768273,-20.1028790535695,
-19.6125649303117,-19.1222508070539,-18.6319366837961,-18.1416225605383,
-17.6513084372805,-17.1609943140227,-16.6706801907649,-16.4226002174572),
 .UNSPECIFIED.);
#275=B_SPLINE_CURVE_WITH_KNOTS('',3,(#20459,#20460,#20461,#20462,#20463,
#20464,#20465,#20466,#20467,#20468,#20469,#20470,#20471,#20472,#20473,#20474,
#20475,#20476,#20477,#20478,#20479,#20480,#20481,#20482,#20483,#20484,#20485,
#20486,#20487,#20488,#20489,#20490,#20491,#20492,#20493,#20494,#20495,#20496,
#20497,#20498,#20499,#20500,#20501),.UNSPECIFIED.,.F.,.F.,(4,3,3,3,3,3,
3,3,3,3,3,3,3,3,4),(13.8759337553363,14.219109574476,14.7094236977338,15.1997378209915,
15.6900519442493,16.1803660675071,16.6706801907649,17.1609943140227,17.6513084372805,
18.1416225605383,18.6319366837961,19.1222508070539,19.6125649303117,20.1028790535695,
20.1591190625159),.UNSPECIFIED.);
#276=B_SPLINE_CURVE_WITH_KNOTS('',3,(#20502,#20503,#20504,#20505,#20506,
#20507,#20508,#20509,#20510,#20511,#20512,#20513,#20514,#20515,#20516,#20517,
#20518,#20519,#20520,#20521,#20522,#20523,#20524,#20525,#20526,#20527,#20528,
#20529,#20530,#20531,#20532,#20533,#20534,#20535,#20536,#20537,#20538,#20539,
#20540,#20541,#20542,#20543,#20544),.UNSPECIFIED.,.F.,.F.,(4,3,3,3,3,3,
3,3,3,3,3,3,3,3,4),(-16.4226002174572,-16.1803660675071,-15.6900519442493,
-15.1997378209915,-14.7094236977338,-14.219109574476,-13.7287954512182,
-13.2384813279604,-12.7481672047026,-12.2578530814448,-11.767538958187,
-11.2772248349292,-10.7869107116714,-10.2965965884136,-10.1394149102777),
 .UNSPECIFIED.);
#277=B_SPLINE_CURVE_WITH_KNOTS('',3,(#20550,#20551,#20552,#20553,#20554,
#20555,#20556,#20557,#20558,#20559,#20560,#20561,#20562,#20563,#20564,#20565,
#20566,#20567,#20568,#20569,#20570,#20571,#20572,#20573,#20574),
 .UNSPECIFIED.,.F.,.F.,(4,3,3,3,3,3,3,3,4),(-3.85622960309808,-3.43219886280454,
-2.94188473954675,-2.45157061628896,-1.96125649303117,-1.47094236977338,
-0.980628246515584,-0.490314123257793,0.),.UNSPECIFIED.);
#278=B_SPLINE_CURVE_WITH_KNOTS('',3,(#20577,#20578,#20579,#20580,#20581,
#20582,#20583,#20584,#20585,#20586,#20587,#20588,#20589,#20590,#20591,#20592,
#20593,#20594,#20595,#20596,#20597,#20598,#20599,#20600,#20601,#20602,#20603,
#20604,#20605,#20606,#20607,#20608,#20609,#20610,#20611,#20612,#20613),
 .UNSPECIFIED.,.F.,.F.,(4,3,3,3,3,3,3,3,3,3,3,3,4),(2.02420009048538,2.45157061628896,
2.94188473954675,3.43219886280454,3.92251298606233,4.41282710932012,4.90314123257792,
5.39345535583571,5.8837694790935,6.37408360235129,6.86439772560908,7.35471184886687,
7.59274844815668),.UNSPECIFIED.);
#279=B_SPLINE_CURVE_WITH_KNOTS('',3,(#20619,#20620,#20621,#20622,#20623,
#20624,#20625,#20626,#20627,#20628,#20629),.UNSPECIFIED.,.F.,.F.,(4,1,1,
1,1,1,1,1,4),(53.4070751110265,53.5284341417632,54.018748265021,54.5090623882788,
54.9993765115366,55.4896906347944,55.9800047580521,56.4703188813099,56.9606330045677),
 .UNSPECIFIED.);
#280=B_SPLINE_CURVE_WITH_KNOTS('',3,(#20632,#20633,#20634,#20635,#20636,
#20637,#20638,#20639,#20640,#20641,#20642,#20643),.UNSPECIFIED.,.F.,.F.,
(4,1,1,1,1,1,1,1,1,4),(53.4070751110265,53.6235299875952,54.113844110853,
54.6041582341108,55.0944723573686,55.5847864806264,56.0751006038842,56.5654147271419,
57.0557288503997,57.4830993762033),.UNSPECIFIED.);
#281=B_SPLINE_CURVE_WITH_KNOTS('',3,(#20648,#20649,#20650,#20651,#20652,
#20653,#20654,#20655,#20656,#20657,#20658,#20659,#20660,#20661,#20662,#20663,
#20664),.UNSPECIFIED.,.F.,.F.,(4,1,1,1,1,1,1,1,1,1,1,1,1,1,4),(47.1238898038469,
47.1543505394119,47.6446646626697,48.1349787859275,48.6252929091853,49.1156070324431,
49.6059211557009,50.0962352789586,50.5865494022164,51.0768635254742,51.567177648732,
52.0574917719898,52.5478058952476,53.0381200185054,53.4070751110265),
 .UNSPECIFIED.);
#282=B_SPLINE_CURVE_WITH_KNOTS('',3,(#20665,#20666,#20667,#20668,#20669,
#20670,#20671,#20672,#20673,#20674,#20675,#20676,#20677,#20678,#20679,#20680,
#20681),.UNSPECIFIED.,.F.,.F.,(4,1,1,1,1,1,1,1,1,1,1,1,1,1,4),(47.1238898038469,
47.2494463852439,47.7397605085017,48.2300746317595,48.7203887550173,49.2107028782751,
49.7010170015329,50.1913311247907,50.6816452480484,51.1719593713062,51.662273494564,
52.1525876178218,52.6429017410796,53.1332158643374,53.4070751110265),
 .UNSPECIFIED.);
#283=B_SPLINE_CURVE_WITH_KNOTS('',3,(#20686,#20687,#20688,#20689,#20690,
#20691,#20692,#20693,#20694,#20695,#20696,#20697,#20698,#20699,#20700,#20701),
 .UNSPECIFIED.,.F.,.F.,(4,1,1,1,1,1,1,1,1,1,1,1,1,4),(40.8407044966673,
41.2705810603184,41.7608951835762,42.251209306834,42.7415234300918,43.2318375533496,
43.7221516766074,44.2124657998651,44.7027799231229,45.1930940463807,45.6834081696385,
46.1737222928963,46.6640364161541,47.1238898038469),.UNSPECIFIED.);
#284=B_SPLINE_CURVE_WITH_KNOTS('',3,(#20702,#20703,#20704,#20705,#20706,
#20707,#20708,#20709,#20710,#20711,#20712,#20713,#20714,#20715,#20716,#20717,
#20718),.UNSPECIFIED.,.F.,.F.,(4,1,1,1,1,1,1,1,1,1,1,1,1,1,4),(40.8407044966673,
40.8753627828926,41.3656769061504,41.8559910294082,42.346305152666,42.8366192759238,
43.3269333991816,43.8172475224394,44.3075616456971,44.7978757689549,45.2881898922127,
45.7785040154705,46.2688181387283,46.7591322619861,47.1238898038469),
 .UNSPECIFIED.);
#285=B_SPLINE_CURVE_WITH_KNOTS('',3,(#20723,#20724,#20725,#20726,#20727,
#20728,#20729,#20730,#20731,#20732,#20733,#20734,#20735,#20736,#20737,#20738,
#20739),.UNSPECIFIED.,.F.,.F.,(4,1,1,1,1,1,1,1,1,1,1,1,1,1,4),(34.5575191894877,
34.8964974579671,35.3868115812249,35.8771257044827,36.3674398277405,36.8577539509983,
37.3480680742561,37.8383821975139,38.3286963207716,38.8190104440294,39.3093245672872,
39.799638690545,40.2899528138028,40.7802669370606,40.8407044966673),
 .UNSPECIFIED.);
#286=B_SPLINE_CURVE_WITH_KNOTS('',3,(#20740,#20741,#20742,#20743,#20744,
#20745,#20746,#20747,#20748,#20749,#20750,#20751,#20752,#20753,#20754,#20755),
 .UNSPECIFIED.,.F.,.F.,(4,1,1,1,1,1,1,1,1,1,1,1,1,4),(34.5575191894877,
34.9915933037991,35.4819074270569,35.9722215503147,36.4625356735725,36.9528497968303,
37.4431639200881,37.9334780433459,38.4237921666036,38.9141062898614,39.4044204131192,
39.894734536377,40.3850486596348,40.8407044966673),.UNSPECIFIED.);
#287=B_SPLINE_CURVE_WITH_KNOTS('',3,(#20760,#20761,#20762,#20763,#20764,
#20765,#20766,#20767,#20768,#20769,#20770,#20771,#20772,#20773,#20774,#20775,
#20776),.UNSPECIFIED.,.F.,.F.,(4,1,1,1,1,1,1,1,1,1,1,1,1,1,4),(28.2743338823081,
28.5224138556158,29.0127279788736,29.5030421021314,29.9933562253892,30.483670348647,
30.9739844719048,31.4642985951626,31.9546127184203,32.4449268416781,32.9352409649359,
33.4255550881937,33.9158692114515,34.4061833347093,34.5575191894877),
 .UNSPECIFIED.);
#288=B_SPLINE_CURVE_WITH_KNOTS('',3,(#20777,#20778,#20779,#20780,#20781,
#20782,#20783,#20784,#20785,#20786,#20787,#20788,#20789,#20790,#20791,#20792,
#20793),.UNSPECIFIED.,.F.,.F.,(4,1,1,1,1,1,1,1,1,1,1,1,1,1,4),(28.2743338823081,
28.6175097014478,29.1078238247056,29.5981379479634,30.0884520712212,30.578766194479,
31.0690803177368,31.5593944409946,32.0497085642524,32.5400226875101,33.0303368107679,
33.5206509340257,34.0109650572835,34.5012791805413,34.5575191894877),
 .UNSPECIFIED.);
#289=B_SPLINE_CURVE_WITH_KNOTS('',3,(#20798,#20799,#20800,#20801,#20802,
#20803,#20804,#20805,#20806,#20807,#20808,#20809,#20810,#20811,#20812,#20813,
#20814),.UNSPECIFIED.,.F.,.F.,(4,1,1,1,1,1,1,1,1,1,1,1,1,1,4),(21.9911485751285,
22.1483302532645,22.6386443765223,23.1289584997801,23.6192726230379,24.1095867462957,
24.5999008695535,25.0902149928113,25.5805291160691,26.0708432393268,26.5611573625846,
27.0514714858424,27.5417856091002,28.032099732358,28.2743338823081),
 .UNSPECIFIED.);
#290=B_SPLINE_CURVE_WITH_KNOTS('',3,(#20815,#20816,#20817,#20818,#20819,
#20820,#20821,#20822,#20823,#20824,#20825,#20826,#20827,#20828,#20829,#20830,
#20831),.UNSPECIFIED.,.F.,.F.,(4,1,1,1,1,1,1,1,1,1,1,1,1,1,4),(21.9911485751285,
22.2434260990965,22.7337402223543,23.2240543456121,23.7143684688699,24.2046825921277,
24.6949967153855,25.1853108386433,25.6756249619011,26.1659390851589,26.6562532084167,
27.1465673316744,27.6368814549322,28.12719557819,28.2743338823081),
 .UNSPECIFIED.);
#291=B_SPLINE_CURVE_WITH_KNOTS('',3,(#20837,#20838,#20839,#20840,#20841,
#20842),.UNSPECIFIED.,.F.,.F.,(4,1,1,4),(14.3984001269719,14.8887142502297,
15.3790283734874,15.7079632679489),.UNSPECIFIED.);
#292=B_SPLINE_CURVE_WITH_KNOTS('',3,(#20845,#20846,#20847,#20848,#20849,
#20850,#20851),.UNSPECIFIED.,.F.,.F.,(4,1,1,1,4),(13.8759337553363,14.3033042811398,
14.7936184043976,15.2839325276554,15.7079632679489),.UNSPECIFIED.);
#293=B_SPLINE_CURVE_WITH_KNOTS('',3,(#20857,#20858,#20859,#20860,#20861,
#20862,#20863,#20864,#20865,#20866,#20867,#20868,#20869,#20870,#20871,#20872),
 .UNSPECIFIED.,.F.,.F.,(4,3,3,3,3,4),(114.407157784405,114.712345376808,
115.709844032258,116.707342687709,117.704841343159,118.70233999861),
 .UNSPECIFIED.);
#294=B_SPLINE_CURVE_WITH_KNOTS('',3,(#20880,#20881,#20882,#20883,#20884,
#20885,#20886,#20887,#20888,#20889,#20890,#20891,#20892,#20893,#20894,#20895,
#20896,#20897,#20898,#20899,#20900,#20901),.UNSPECIFIED.,.F.,.F.,(4,3,3,
3,3,3,3,4),(-116.687727133335,-115.709844032258,-114.712345376808,-113.714846721357,
-112.717348065907,-111.719849410456,-110.722350755006,-110.660533485745),
 .UNSPECIFIED.);
#295=B_SPLINE_CURVE_WITH_KNOTS('',3,(#20906,#20907,#20908,#20909,#20910,
#20911,#20912,#20913,#20914,#20915,#20916,#20917,#20918,#20919,#20920,#20921,
#20922,#20923,#20924,#20925,#20926,#20927),.UNSPECIFIED.,.F.,.F.,(4,3,3,
3,3,3,3,4),(108.123972477225,108.727353444105,109.724852099555,110.722350755006,
111.719849410456,112.717348065907,113.714846721357,114.407157784405),
 .UNSPECIFIED.);
#296=B_SPLINE_CURVE_WITH_KNOTS('',3,(#20928,#20929,#20930,#20931,#20932,
#20933,#20934,#20935,#20936,#20937,#20938,#20939,#20940,#20941,#20942,#20943,
#20944,#20945,#20946,#20947,#20948,#20949),.UNSPECIFIED.,.F.,.F.,(4,3,3,
3,3,3,3,4),(-110.660533485745,-109.724852099555,-108.727353444105,-107.729854788654,
-106.732356133204,-105.734857477753,-104.737358822303,-104.377348178566),
 .UNSPECIFIED.);
#297=B_SPLINE_CURVE_WITH_KNOTS('',3,(#20954,#20955,#20956,#20957,#20958,
#20959,#20960,#20961,#20962,#20963,#20964,#20965,#20966,#20967,#20968,#20969,
#20970,#20971,#20972,#20973,#20974,#20975),.UNSPECIFIED.,.F.,.F.,(4,3,3,
3,3,3,3,4),(101.840787170045,102.742361511402,103.739860166852,104.737358822303,
105.734857477753,106.732356133204,107.729854788654,108.123972477225),
 .UNSPECIFIED.);
#298=B_SPLINE_CURVE_WITH_KNOTS('',3,(#20976,#20977,#20978,#20979,#20980,
#20981,#20982,#20983,#20984,#20985,#20986,#20987,#20988,#20989,#20990,#20991,
#20992,#20993,#20994,#20995,#20996,#20997),.UNSPECIFIED.,.F.,.F.,(4,3,3,
3,3,3,3,4),(-104.377348178566,-103.739860166852,-102.742361511402,-101.744862855951,
-100.747364200501,-99.7498655450501,-98.7523668895996,-98.094162871386),
 .UNSPECIFIED.);
#299=B_SPLINE_CURVE_WITH_KNOTS('',3,(#21002,#21003,#21004,#21005,#21006,
#21007,#21008,#21009,#21010,#21011,#21012,#21013,#21014,#21015,#21016,#21017,
#21018,#21019,#21020,#21021,#21022,#21023,#21024,#21025,#21026),
 .UNSPECIFIED.,.F.,.F.,(4,3,3,3,3,3,3,3,4),(95.5576018628658,95.7598709232481,
96.7573695786986,97.7548682341491,98.7523668895996,99.7498655450502,100.747364200501,
101.744862855951,101.840787170045),.UNSPECIFIED.);
#300=B_SPLINE_CURVE_WITH_KNOTS('',3,(#21027,#21028,#21029,#21030,#21031,
#21032,#21033,#21034,#21035,#21036,#21037,#21038,#21039,#21040,#21041,#21042,
#21043,#21044,#21045,#21046,#21047,#21048),.UNSPECIFIED.,.F.,.F.,(4,3,3,
3,3,3,3,4),(-98.094162871386,-97.7548682341491,-96.7573695786986,-95.7598709232481,
-94.7623722677976,-93.7648736123471,-92.7673749568966,-91.8109775642064),
 .UNSPECIFIED.);
#301=B_SPLINE_CURVE_WITH_KNOTS('',3,(#21053,#21054,#21055,#21056,#21057,
#21058,#21059,#21060,#21061,#21062,#21063,#21064,#21065,#21066,#21067,#21068,
#21069,#21070,#21071,#21072,#21073,#21074),.UNSPECIFIED.,.F.,.F.,(4,3,3,
3,3,3,3,4),(89.2744165556862,89.7748789905451,90.7723776459956,91.7698763014461,
92.7673749568966,93.7648736123471,94.7623722677976,95.5576018628658),
 .UNSPECIFIED.);
#302=B_SPLINE_CURVE_WITH_KNOTS('',3,(#21075,#21076,#21077,#21078,#21079,
#21080,#21081,#21082,#21083,#21084,#21085,#21086,#21087,#21088,#21089,#21090,
#21091,#21092,#21093,#21094,#21095,#21096,#21097,#21098,#21099),
 .UNSPECIFIED.,.F.,.F.,(4,3,3,3,3,3,3,3,4),(-91.8109775642064,-91.7698763014461,
-90.7723776459956,-89.7748789905451,-88.7773803350946,-87.7798816796441,
-86.7823830241936,-85.7848843687431,-85.5277922570269),.UNSPECIFIED.);
#303=B_SPLINE_CURVE_WITH_KNOTS('',3,(#21104,#21105,#21106,#21107,#21108,
#21109,#21110,#21111,#21112,#21113,#21114,#21115,#21116,#21117,#21118,#21119,
#21120,#21121,#21122,#21123,#21124,#21125),.UNSPECIFIED.,.F.,.F.,(4,3,3,
3,3,3,3,4),(82.9912312485066,83.7898870578421,84.7873857132926,85.7848843687431,
86.7823830241936,87.7798816796441,88.7773803350946,89.2744165556862),
 .UNSPECIFIED.);
#304=B_SPLINE_CURVE_WITH_KNOTS('',3,(#21126,#21127,#21128,#21129,#21130,
#21131,#21132,#21133,#21134,#21135,#21136,#21137,#21138,#21139,#21140,#21141,
#21142,#21143,#21144,#21145,#21146,#21147),.UNSPECIFIED.,.F.,.F.,(4,3,3,
3,3,3,3,4),(-85.5277922570269,-84.7873857132926,-83.7898870578422,-82.7923884023916,
-81.7948897469411,-80.7973910914906,-79.7998924360401,-79.2446069498473),
 .UNSPECIFIED.);
#305=B_SPLINE_CURVE_WITH_KNOTS('',3,(#21152,#21153,#21154,#21155,#21156,
#21157,#21158,#21159,#21160,#21161,#21162,#21163,#21164,#21165,#21166,#21167,
#21168,#21169,#21170,#21171,#21172,#21173,#21174,#21175,#21176),
 .UNSPECIFIED.,.F.,.F.,(4,3,3,3,3,3,3,3,4),(76.708045941327,76.8073964696886,
77.8048951251391,78.8023937805896,79.7998924360401,80.7973910914906,81.7948897469411,
82.7923884023916,82.9912312485066),.UNSPECIFIED.);
#306=B_SPLINE_CURVE_WITH_KNOTS('',3,(#21177,#21178,#21179,#21180,#21181,
#21182,#21183,#21184,#21185,#21186,#21187,#21188,#21189,#21190,#21191,#21192,
#21193,#21194,#21195,#21196,#21197,#21198),.UNSPECIFIED.,.F.,.F.,(4,3,3,
3,3,3,3,4),(-79.2446069498473,-78.8023937805896,-77.8048951251391,-76.8073964696886,
-75.8098978142381,-74.8123991587876,-73.8149005033371,-72.9614216426677),
 .UNSPECIFIED.);
#307=B_SPLINE_CURVE_WITH_KNOTS('',3,(#21203,#21204,#21205,#21206,#21207,
#21208,#21209,#21210,#21211,#21212,#21213,#21214,#21215,#21216,#21217,#21218,
#21219,#21220,#21221,#21222,#21223,#21224),.UNSPECIFIED.,.F.,.F.,(4,3,3,
3,3,3,3,4),(70.4248606341474,70.8224045369856,71.8199031924361,72.8174018478866,
73.8149005033371,74.8123991587876,75.8098978142381,76.708045941327),
 .UNSPECIFIED.);
#308=B_SPLINE_CURVE_WITH_KNOTS('',3,(#21225,#21226,#21227,#21228,#21229,
#21230,#21231,#21232,#21233,#21234,#21235,#21236,#21237,#21238,#21239,#21240,
#21241,#21242,#21243,#21244,#21245,#21246,#21247,#21248,#21249),
 .UNSPECIFIED.,.F.,.F.,(4,3,3,3,3,3,3,3,4),(-72.9614216426677,-72.8174018478866,
-71.8199031924361,-70.8224045369856,-69.8249058815351,-68.8274072260846,
-67.8299085706341,-66.8324099151836,-66.6782363354882),.UNSPECIFIED.);
#309=B_SPLINE_CURVE_WITH_KNOTS('',3,(#21254,#21255,#21256,#21257,#21258,
#21259,#21260,#21261,#21262,#21263,#21264,#21265,#21266,#21267,#21268,#21269,
#21270,#21271,#21272,#21273,#21274,#21275),.UNSPECIFIED.,.F.,.F.,(4,3,3,
3,3,3,3,4),(64.1416753269678,64.8374126042826,65.8349112597331,66.8324099151836,
67.8299085706341,68.8274072260846,69.8249058815351,70.4248606341474),
 .UNSPECIFIED.);
#310=B_SPLINE_CURVE_WITH_KNOTS('',3,(#21276,#21277,#21278,#21279,#21280,
#21281,#21282,#21283,#21284,#21285,#21286,#21287,#21288,#21289,#21290,#21291,
#21292,#21293,#21294,#21295,#21296,#21297),.UNSPECIFIED.,.F.,.F.,(4,3,3,
3,3,3,3,4),(-66.6782363354882,-65.8349112597331,-64.8374126042826,-63.8399139488321,
-62.8424152933816,-61.8449166379311,-60.8474179824806,-60.3950510283085),
 .UNSPECIFIED.);
#311=B_SPLINE_CURVE_WITH_KNOTS('',3,(#21302,#21303,#21304,#21305,#21306,
#21307,#21308,#21309,#21310,#21311,#21312,#21313,#21314,#21315,#21316,#21317,
#21318,#21319,#21320,#21321,#21322,#21323),.UNSPECIFIED.,.F.,.F.,(4,3,3,
3,3,3,3,4),(57.8584900197882,58.8524206715796,59.8499193270301,60.8474179824806,
61.8449166379311,62.8424152933816,63.8399139488321,64.1416753269678),
 .UNSPECIFIED.);
#312=B_SPLINE_CURVE_WITH_KNOTS('',3,(#21324,#21325,#21326,#21327,#21328,
#21329,#21330,#21331,#21332,#21333,#21334,#21335,#21336,#21337,#21338,#21339,
#21340,#21341,#21342,#21343,#21344,#21345),.UNSPECIFIED.,.F.,.F.,(4,3,3,
3,3,3,3,4),(-60.3950510283085,-59.8499193270301,-58.8524206715796,-57.8549220161291,
-56.8574233606786,-55.8599247052281,-54.8624260497776,-54.1118657211289),
 .UNSPECIFIED.);
#313=B_SPLINE_CURVE_WITH_KNOTS('',3,(#21350,#21351,#21352,#21353,#21354,
#21355,#21356,#21357,#21358,#21359,#21360,#21361,#21362,#21363,#21364,#21365,
#21366,#21367,#21368,#21369,#21370,#21371,#21372,#21373,#21374),
 .UNSPECIFIED.,.F.,.F.,(4,3,3,3,3,3,3,3,4),(51.5753047126086,51.8699300834261,
52.8674287388766,53.8649273943271,54.8624260497776,55.8599247052281,56.8574233606786,
57.8549220161291,57.8584900197882),.UNSPECIFIED.);
#314=B_SPLINE_CURVE_WITH_KNOTS('',3,(#21375,#21376,#21377,#21378,#21379,
#21380,#21381,#21382,#21383,#21384,#21385,#21386,#21387,#21388,#21389,#21390,
#21391,#21392,#21393,#21394,#21395,#21396,#21397,#21398,#21399),
 .UNSPECIFIED.,.F.,.F.,(4,3,3,3,3,3,3,3,4),(-54.1118657211289,-53.8649273943271,
-52.8674287388766,-51.8699300834261,-50.8724314279756,-49.8749327725251,
-48.8774341170746,-47.8799354616241,-47.8286804139493),.UNSPECIFIED.);
#315=B_SPLINE_CURVE_WITH_KNOTS('',3,(#21404,#21405,#21406,#21407,#21408,
#21409,#21410,#21411,#21412,#21413,#21414,#21415,#21416,#21417,#21418,#21419,
#21420,#21421,#21422,#21423,#21424,#21425),.UNSPECIFIED.,.F.,.F.,(4,3,3,
3,3,3,3,4),(45.292119405429,45.8849381507231,46.8824368061736,47.8799354616241,
48.8774341170746,49.8749327725251,50.8724314279756,51.5753047126086),
 .UNSPECIFIED.);
#316=B_SPLINE_CURVE_WITH_KNOTS('',3,(#21426,#21427,#21428,#21429,#21430,
#21431,#21432,#21433,#21434,#21435,#21436,#21437,#21438,#21439,#21440,#21441,
#21442,#21443,#21444,#21445,#21446,#21447),.UNSPECIFIED.,.F.,.F.,(4,3,3,
3,3,3,3,4),(-47.8286804139493,-46.8824368061736,-45.8849381507231,-44.8874394952726,
-43.8899408398221,-42.8924421843716,-41.8949435289211,-41.5454951067697),
 .UNSPECIFIED.);
#317=B_SPLINE_CURVE_WITH_KNOTS('',3,(#21452,#21453,#21454,#21455,#21456,
#21457,#21458,#21459,#21460,#21461,#21462,#21463,#21464,#21465,#21466,#21467,
#21468,#21469,#21470,#21471,#21472,#21473),.UNSPECIFIED.,.F.,.F.,(4,3,3,
3,3,3,3,4),(39.0089340982495,39.8999462180201,40.8974448734706,41.8949435289211,
42.8924421843716,43.8899408398221,44.8874394952726,45.292119405429),
 .UNSPECIFIED.);
#318=B_SPLINE_CURVE_WITH_KNOTS('',3,(#21474,#21475,#21476,#21477,#21478,
#21479,#21480,#21481,#21482,#21483,#21484,#21485,#21486,#21487,#21488,#21489,
#21490,#21491,#21492,#21493,#21494,#21495),.UNSPECIFIED.,.F.,.F.,(4,3,3,
3,3,3,3,4),(-41.5454951067697,-40.8974448734706,-39.8999462180201,-38.9024475625696,
-37.9049489071191,-36.9074502516685,-35.909951596218,-35.2623097995902),
 .UNSPECIFIED.);
#319=B_SPLINE_CURVE_WITH_KNOTS('',3,(#21500,#21501,#21502,#21503,#21504,
#21505,#21506,#21507,#21508,#21509,#21510,#21511,#21512,#21513,#21514,#21515,
#21516,#21517,#21518,#21519,#21520,#21521,#21522,#21523,#21524),
 .UNSPECIFIED.,.F.,.F.,(4,3,3,3,3,3,3,3,4),(32.7257487910699,32.9174556298666,
33.9149542853171,34.9124529407676,35.9099515962181,36.9074502516685,37.9049489071191,
38.9024475625696,39.0089340982495),.UNSPECIFIED.);
#320=B_SPLINE_CURVE_WITH_KNOTS('',3,(#21525,#21526,#21527,#21528,#21529,
#21530,#21531,#21532,#21533,#21534,#21535,#21536,#21537,#21538,#21539,#21540,
#21541,#21542,#21543,#21544,#21545,#21546),.UNSPECIFIED.,.F.,.F.,(4,3,3,
3,3,3,3,4),(-35.2623097995902,-34.9124529407676,-33.9149542853171,-32.9174556298665,
-31.919956974416,-30.9224583189655,-29.9249596635151,-28.9791244924106),
 .UNSPECIFIED.);
#321=B_SPLINE_CURVE_WITH_KNOTS('',3,(#21551,#21552,#21553,#21554,#21555,
#21556,#21557,#21558,#21559,#21560,#21561,#21562,#21563,#21564,#21565,#21566,
#21567,#21568,#21569,#21570,#21571,#21572),.UNSPECIFIED.,.F.,.F.,(4,3,3,
3,3,3,3,4),(26.4425634838902,26.9324636971635,27.929962352614,28.9274610080645,
29.924959663515,30.9224583189655,31.9199569744161,32.7257487910699),
 .UNSPECIFIED.);
#322=B_SPLINE_CURVE_WITH_KNOTS('',3,(#21573,#21574,#21575,#21576,#21577,
#21578,#21579,#21580,#21581,#21582,#21583,#21584,#21585,#21586,#21587,#21588,
#21589,#21590,#21591,#21592,#21593,#21594,#21595,#21596,#21597),
 .UNSPECIFIED.,.F.,.F.,(4,3,3,3,3,3,3,3,4),(-28.9791244924106,-28.9274610080645,
-27.929962352614,-26.9324636971635,-25.934965041713,-24.9374663862625,-23.939967730812,
-22.9424690753615,-22.6959391852309),.UNSPECIFIED.);
#323=B_SPLINE_CURVE_WITH_KNOTS('',3,(#21602,#21603,#21604,#21605,#21606,
#21607,#21608,#21609,#21610,#21611,#21612,#21613,#21614,#21615,#21616,#21617,
#21618,#21619,#21620,#21621,#21622,#21623),.UNSPECIFIED.,.F.,.F.,(4,3,3,
3,3,3,3,4),(20.1593781767107,20.9474717644605,21.944970419911,22.9424690753615,
23.939967730812,24.9374663862625,25.934965041713,26.4425634838902),
 .UNSPECIFIED.);
#324=B_SPLINE_CURVE_WITH_KNOTS('',3,(#21624,#21625,#21626,#21627,#21628,
#21629,#21630,#21631,#21632,#21633,#21634,#21635,#21636,#21637,#21638,#21639,
#21640,#21641,#21642,#21643,#21644,#21645),.UNSPECIFIED.,.F.,.F.,(4,3,3,
3,3,3,3,4),(-22.6959391852309,-21.944970419911,-20.9474717644605,-19.94997310901,
-18.9524744535595,-17.954975798109,-16.9574771426585,-16.4127538780514),
 .UNSPECIFIED.);
#325=B_SPLINE_CURVE_WITH_KNOTS('',3,(#21650,#21651,#21652,#21653,#21654,
#21655,#21656,#21657,#21658,#21659,#21660,#21661,#21662,#21663,#21664,#21665,
#21666,#21667,#21668,#21669,#21670,#21671,#21672,#21673,#21674),
 .UNSPECIFIED.,.F.,.F.,(4,3,3,3,3,3,3,3,4),(13.8761928695311,13.964981176307,
14.9624798317575,15.959978487208,16.9574771426585,17.954975798109,18.9524744535595,
19.94997310901,20.1593781767107),.UNSPECIFIED.);
#326=B_SPLINE_CURVE_WITH_KNOTS('',3,(#21675,#21676,#21677,#21678,#21679,
#21680,#21681,#21682,#21683,#21684,#21685,#21686,#21687,#21688,#21689,#21690,
#21691,#21692,#21693,#21694,#21695,#21696),.UNSPECIFIED.,.F.,.F.,(4,3,3,
3,3,3,3,4),(-16.4127538780514,-15.959978487208,-14.9624798317575,-13.964981176307,
-12.9674825208565,-11.969983865406,-10.9724852099555,-10.1295685708718),
 .UNSPECIFIED.);
#327=B_SPLINE_CURVE_WITH_KNOTS('',3,(#21702,#21703,#21704,#21705,#21706,
#21707,#21708,#21709,#21710,#21711,#21712,#21713,#21714),.UNSPECIFIED.,
 .F.,.F.,(4,3,3,3,4),(-3.84638326369218,-2.9924959663515,-1.994997310901,
-0.997498655450501,0.),.UNSPECIFIED.);
#328=B_SPLINE_CURVE_WITH_KNOTS('',3,(#21717,#21718,#21719,#21720,#21721,
#21722,#21723,#21724,#21725,#21726,#21727,#21728,#21729,#21730,#21731,#21732,
#21733,#21734,#21735),.UNSPECIFIED.,.F.,.F.,(4,3,3,3,3,3,4),(2.01461286527449,
2.9924959663515,3.989994621802,4.98749327725251,5.98499193270301,6.98249058815351,
7.59300756235149),.UNSPECIFIED.);
#329=B_SPLINE_CURVE_WITH_KNOTS('',3,(#21741,#21742,#21743,#21744,#21745),
 .UNSPECIFIED.,.F.,.F.,(4,1,4),(128.805298797182,129.566421347416,130.563920002866),
 .UNSPECIFIED.);
#330=B_SPLINE_CURVE_WITH_KNOTS('',3,(#21748,#21749,#21750,#21751,#21752,
#21753),.UNSPECIFIED.,.F.,.F.,(4,1,1,4),(128.805298797182,129.110486389585,
130.107985045035,131.085868146112),.UNSPECIFIED.);
#331=B_SPLINE_CURVE_WITH_KNOTS('',3,(#21758,#21759,#21760,#21761,#21762,
#21763,#21764,#21765,#21766,#21767,#21768),.UNSPECIFIED.,.F.,.F.,(4,1,1,
1,1,1,1,1,4),(122.522113490002,122.583930759262,123.581429414713,124.578928070163,
125.576426725614,126.573925381064,127.571424036515,128.568922691965,128.805298797182),
 .UNSPECIFIED.);
#332=B_SPLINE_CURVE_WITH_KNOTS('',3,(#21769,#21770,#21771,#21772,#21773,
#21774,#21775,#21776,#21777,#21778),.UNSPECIFIED.,.F.,.F.,(4,1,1,1,1,1,
1,4),(122.522113490002,123.125494456882,124.122993112332,125.120491767783,
126.117990423233,127.115489078684,128.112987734134,128.805298797182),
 .UNSPECIFIED.);
#333=B_SPLINE_CURVE_WITH_KNOTS('',3,(#21783,#21784,#21785,#21786,#21787,
#21788,#21789,#21790,#21791,#21792),.UNSPECIFIED.,.F.,.F.,(4,1,1,1,1,1,
1,4),(116.238928182822,116.598938826559,117.59643748201,118.59393613746,
119.591434792911,120.588933448361,121.586432103812,122.522113490002),
 .UNSPECIFIED.);
#334=B_SPLINE_CURVE_WITH_KNOTS('',3,(#21793,#21794,#21795,#21796,#21797,
#21798,#21799,#21800,#21801,#21802),.UNSPECIFIED.,.F.,.F.,(4,1,1,1,1,1,
1,4),(116.238928182822,117.140502524179,118.138001179629,119.13549983508,
120.13299849053,121.130497145981,122.127995801431,122.522113490002),
 .UNSPECIFIED.);
#335=B_SPLINE_CURVE_WITH_KNOTS('',3,(#21807,#21808,#21809,#21810,#21811,
#21812,#21813,#21814,#21815,#21816),.UNSPECIFIED.,.F.,.F.,(4,1,1,1,1,1,
1,4),(109.955742875643,110.613946893856,111.611445549307,112.608944204757,
113.606442860208,114.603941515658,115.601440171109,116.238928182822),
 .UNSPECIFIED.);
#336=B_SPLINE_CURVE_WITH_KNOTS('',3,(#21817,#21818,#21819,#21820,#21821,
#21822,#21823,#21824,#21825,#21826,#21827),.UNSPECIFIED.,.F.,.F.,(4,1,1,
1,1,1,1,1,4),(109.955742875643,110.158011936025,111.155510591476,112.153009246926,
113.150507902377,114.148006557827,115.145505213278,116.143003868728,116.238928182822),
 .UNSPECIFIED.);
#337=B_SPLINE_CURVE_WITH_KNOTS('',3,(#21832,#21833,#21834,#21835,#21836,
#21837,#21838,#21839,#21840,#21841),.UNSPECIFIED.,.F.,.F.,(4,1,1,1,1,1,
1,4),(103.672557568463,104.628954961153,105.626453616604,106.623952272054,
107.621450927505,108.618949582955,109.616448238406,109.955742875643),
 .UNSPECIFIED.);
#338=B_SPLINE_CURVE_WITH_KNOTS('',3,(#21842,#21843,#21844,#21845,#21846,
#21847,#21848,#21849,#21850,#21851),.UNSPECIFIED.,.F.,.F.,(4,1,1,1,1,1,
1,4),(103.672557568463,104.173020003322,105.170518658772,106.168017314223,
107.165515969673,108.163014625124,109.160513280574,109.955742875643),
 .UNSPECIFIED.);
#339=B_SPLINE_CURVE_WITH_KNOTS('',3,(#21856,#21857,#21858,#21859,#21860,
#21861,#21862,#21863,#21864,#21865,#21866),.UNSPECIFIED.,.F.,.F.,(4,1,1,
1,1,1,1,1,4),(97.3893722612835,97.6464643729998,98.6439630284503,99.6414616839008,
100.638960339351,101.636458994802,102.633957650252,103.631456305703,103.672557568463),
 .UNSPECIFIED.);
#340=B_SPLINE_CURVE_WITH_KNOTS('',3,(#21867,#21868,#21869,#21870,#21871,
#21872,#21873,#21874,#21875,#21876),.UNSPECIFIED.,.F.,.F.,(4,1,1,1,1,1,
1,4),(97.3893722612835,98.188028070619,99.1855267260695,100.18302538152,
101.18052403697,102.178022692421,103.175521347871,103.672557568463),
 .UNSPECIFIED.);
#341=B_SPLINE_CURVE_WITH_KNOTS('',3,(#21881,#21882,#21883,#21884,#21885,
#21886,#21887,#21888,#21889,#21890),.UNSPECIFIED.,.F.,.F.,(4,1,1,1,1,1,
1,4),(91.106186954104,91.6614724402968,92.6589710957473,93.6564697511978,
94.6539684066483,95.6514670620988,96.6489657175493,97.3893722612835),
 .UNSPECIFIED.);
#342=B_SPLINE_CURVE_WITH_KNOTS('',3,(#21891,#21892,#21893,#21894,#21895,
#21896,#21897,#21898,#21899,#21900,#21901),.UNSPECIFIED.,.F.,.F.,(4,1,1,
1,1,1,1,1,4),(91.106186954104,91.2055374824655,92.203036137916,93.2005347933665,
94.198033448817,95.1955321042675,96.193030759718,97.1905294151685,97.3893722612835),
 .UNSPECIFIED.);
#343=B_SPLINE_CURVE_WITH_KNOTS('',3,(#21906,#21907,#21908,#21909,#21910,
#21911,#21912,#21913,#21914,#21915),.UNSPECIFIED.,.F.,.F.,(4,1,1,1,1,1,
1,4),(84.8230016469244,85.6764805075938,86.6739791630443,87.6714778184948,
88.6689764739453,89.6664751293958,90.6639737848463,91.106186954104),
 .UNSPECIFIED.);
#344=B_SPLINE_CURVE_WITH_KNOTS('',3,(#21916,#21917,#21918,#21919,#21920,
#21921,#21922,#21923,#21924,#21925),.UNSPECIFIED.,.F.,.F.,(4,1,1,1,1,1,
1,4),(84.8230016469244,85.2205455497625,86.218044205213,87.2155428606635,
88.213041516114,89.2105401715645,90.208038827015,91.106186954104),
 .UNSPECIFIED.);
#345=B_SPLINE_CURVE_WITH_KNOTS('',3,(#21930,#21931,#21932,#21933,#21934,
#21935,#21936,#21937,#21938,#21939,#21940),.UNSPECIFIED.,.F.,.F.,(4,1,1,
1,1,1,1,1,4),(78.5398163397448,78.6939899194402,79.6914885748908,80.6889872303413,
81.6864858857918,82.6839845412423,83.6814831966928,84.6789818521433,84.8230016469244),
 .UNSPECIFIED.);
#346=B_SPLINE_CURVE_WITH_KNOTS('',3,(#21941,#21942,#21943,#21944,#21945,
#21946,#21947,#21948,#21949,#21950),.UNSPECIFIED.,.F.,.F.,(4,1,1,1,1,1,
1,4),(78.5398163397448,79.2355536170595,80.23305227251,81.2305509279605,
82.228049583411,83.2255482388615,84.223046894312,84.8230016469244),
 .UNSPECIFIED.);
#347=B_SPLINE_CURVE_WITH_KNOTS('',3,(#21955,#21956,#21957,#21958,#21959,
#21960,#21961,#21962,#21963,#21964),.UNSPECIFIED.,.F.,.F.,(4,1,1,1,1,1,
1,4),(72.2566310325652,72.7089979867372,73.7064966421877,74.7039952976382,
75.7014939530887,76.6989926085392,77.6964912639897,78.5398163397448),
 .UNSPECIFIED.);
#348=B_SPLINE_CURVE_WITH_KNOTS('',3,(#21965,#21966,#21967,#21968,#21969,
#21970,#21971,#21972,#21973,#21974),.UNSPECIFIED.,.F.,.F.,(4,1,1,1,1,1,
1,4),(72.2566310325652,73.2505616843565,74.248060339807,75.2455589952575,
76.243057650708,77.2405563061585,78.238054961609,78.5398163397448),
 .UNSPECIFIED.);
#349=B_SPLINE_CURVE_WITH_KNOTS('',3,(#21979,#21980,#21981,#21982,#21983,
#21984,#21985,#21986,#21987,#21988),.UNSPECIFIED.,.F.,.F.,(4,1,1,1,1,1,
1,4),(65.9734457253856,66.7240060540342,67.7215047094847,68.7190033649352,
69.7165020203857,70.7140006758362,71.7114993312867,72.2566310325652),
 .UNSPECIFIED.);
#350=B_SPLINE_CURVE_WITH_KNOTS('',3,(#21989,#21990,#21991,#21992,#21993,
#21994,#21995,#21996,#21997,#21998,#21999),.UNSPECIFIED.,.F.,.F.,(4,1,1,
1,1,1,1,1,4),(65.9734457253856,66.2680710962029,67.2655697516534,68.2630684071039,
69.2605670625544,70.2580657180049,71.2555643734554,72.2530630289059,72.2566310325652),
 .UNSPECIFIED.);
#351=B_SPLINE_CURVE_WITH_KNOTS('',3,(#22004,#22005,#22006,#22007,#22008,
#22009,#22010,#22011,#22012,#22013,#22014),.UNSPECIFIED.,.F.,.F.,(4,1,1,
1,1,1,1,1,4),(59.690260418206,59.7415154658807,60.7390141213312,61.7365127767817,
62.7340114322322,63.7315100876827,64.7290087431332,65.7265073985837,65.9734457253856),
 .UNSPECIFIED.);
#352=B_SPLINE_CURVE_WITH_KNOTS('',3,(#22015,#22016,#22017,#22018,#22019,
#22020,#22021,#22022,#22023,#22024),.UNSPECIFIED.,.F.,.F.,(4,1,1,1,1,1,
1,4),(59.690260418206,60.2830791634999,61.2805778189504,62.2780764744009,
63.2755751298514,64.2730737853019,65.2705724407524,65.9734457253856),
 .UNSPECIFIED.);
#353=B_SPLINE_CURVE_WITH_KNOTS('',3,(#22029,#22030,#22031,#22032,#22033,
#22034,#22035,#22036,#22037,#22038),.UNSPECIFIED.,.F.,.F.,(4,1,1,1,1,1,
1,4),(53.4070751110264,53.7565235331777,54.7540221886282,55.7515208440787,
56.7490194995292,57.7465181549797,58.7440168104302,59.690260418206),
 .UNSPECIFIED.);
#354=B_SPLINE_CURVE_WITH_KNOTS('',3,(#22039,#22040,#22041,#22042,#22043,
#22044,#22045,#22046,#22047,#22048),.UNSPECIFIED.,.F.,.F.,(4,1,1,1,1,1,
1,4),(53.4070751110264,54.2980872307969,55.2955858862474,56.2930845416979,
57.2905831971484,58.2880818525989,59.2855805080494,59.690260418206),
 .UNSPECIFIED.);
#355=B_SPLINE_CURVE_WITH_KNOTS('',3,(#22053,#22054,#22055,#22056,#22057,
#22058,#22059,#22060,#22061,#22062),.UNSPECIFIED.,.F.,.F.,(4,1,1,1,1,1,
1,4),(47.1238898038468,47.7715316004747,48.7690302559252,49.7665289113757,
50.7640275668262,51.7615262222767,52.7590248777272,53.4070751110264),
 .UNSPECIFIED.);
#356=B_SPLINE_CURVE_WITH_KNOTS('',3,(#22063,#22064,#22065,#22066,#22067,
#22068,#22069,#22070,#22071,#22072,#22073),.UNSPECIFIED.,.F.,.F.,(4,1,1,
1,1,1,1,1,4),(47.1238898038468,47.3155966426434,48.3130952980939,49.3105939535444,
50.3080926089949,51.3055912644454,52.3030899198959,53.3005885753464,53.4070751110264),
 .UNSPECIFIED.);
#357=B_SPLINE_CURVE_WITH_KNOTS('',3,(#22078,#22079,#22080,#22081,#22082,
#22083,#22084,#22085,#22086,#22087),.UNSPECIFIED.,.F.,.F.,(4,1,1,1,1,1,
1,4),(40.8407044966672,41.7865396677717,42.7840383232222,43.7815369786727,
44.7790356341232,45.7765342895737,46.7740329450242,47.1238898038468),
 .UNSPECIFIED.);
#358=B_SPLINE_CURVE_WITH_KNOTS('',3,(#22088,#22089,#22090,#22091,#22092,
#22093,#22094,#22095,#22096,#22097),.UNSPECIFIED.,.F.,.F.,(4,1,1,1,1,1,
1,4),(40.8407044966672,41.3306047099404,42.3281033653909,43.3256020208414,
44.3231006762919,45.3205993317424,46.3180979871929,47.1238898038468),
 .UNSPECIFIED.);
#359=B_SPLINE_CURVE_WITH_KNOTS('',3,(#22102,#22103,#22104,#22105,#22106,
#22107,#22108,#22109,#22110,#22111,#22112),.UNSPECIFIED.,.F.,.F.,(4,1,1,
1,1,1,1,1,4),(34.5575191894877,34.8040490796182,35.8015477350687,36.7990463905192,
37.7965450459697,38.7940437014202,39.7915423568707,40.7890410123212,40.8407044966672),
 .UNSPECIFIED.);
#360=B_SPLINE_CURVE_WITH_KNOTS('',3,(#22113,#22114,#22115,#22116,#22117,
#22118,#22119,#22120,#22121,#22122),.UNSPECIFIED.,.F.,.F.,(4,1,1,1,1,1,
1,4),(34.5575191894877,35.3456127772374,36.3431114326879,37.3406100881384,
38.3381087435889,39.3356073990394,40.3331060544899,40.8407044966672),
 .UNSPECIFIED.);
#361=B_SPLINE_CURVE_WITH_KNOTS('',3,(#22127,#22128,#22129,#22130,#22131,
#22132,#22133,#22134,#22135,#22136),.UNSPECIFIED.,.F.,.F.,(4,1,1,1,1,1,
1,4),(28.2743338823081,28.8190571469152,29.8165558023657,30.8140544578162,
31.8115531132667,32.8090517687172,33.8065504241677,34.5575191894877),
 .UNSPECIFIED.);
#362=B_SPLINE_CURVE_WITH_KNOTS('',3,(#22137,#22138,#22139,#22140,#22141,
#22142,#22143,#22144,#22145,#22146,#22147),.UNSPECIFIED.,.F.,.F.,(4,1,1,
1,1,1,1,1,4),(28.2743338823081,28.3631221890839,29.3606208445344,30.3581194999849,
31.3556181554354,32.3531168108859,33.3506154663364,34.3481141217869,34.5575191894877),
 .UNSPECIFIED.);
#363=B_SPLINE_CURVE_WITH_KNOTS('',3,(#22152,#22153,#22154,#22155,#22156,
#22157,#22158,#22159,#22160,#22161),.UNSPECIFIED.,.F.,.F.,(4,1,1,1,1,1,
1,4),(21.9911485751284,22.8340652142122,23.8315638696627,24.8290625251132,
25.8265611805637,26.8240598360142,27.8215584914647,28.2743338823081),
 .UNSPECIFIED.);
#364=B_SPLINE_CURVE_WITH_KNOTS('',3,(#22162,#22163,#22164,#22165,#22166,
#22167,#22168,#22169,#22170,#22171),.UNSPECIFIED.,.F.,.F.,(4,1,1,1,1,1,
1,4),(21.9911485751284,22.3781302563809,23.3756289118314,24.3731275672819,
25.3706262227324,26.3681248781829,27.3656235336334,28.2743338823081),
 .UNSPECIFIED.);
#365=B_SPLINE_CURVE_WITH_KNOTS('',3,(#22177,#22178,#22179,#22180,#22181),
 .UNSPECIFIED.,.F.,.F.,(4,1,4),(14.3981410127769,15.3956396682274,15.7079632679489),
 .UNSPECIFIED.);
#366=B_SPLINE_CURVE_WITH_KNOTS('',3,(#22184,#22185,#22186,#22187,#22188),
 .UNSPECIFIED.,.F.,.F.,(4,1,4),(13.8761928695311,14.8540759706082,15.7079632679489),
 .UNSPECIFIED.);
#367=B_SPLINE_CURVE_WITH_KNOTS('',3,(#22194,#22195,#22196,#22197,#22198,
#22199,#22200,#22201,#22202,#22203,#22204,#22205,#22206,#22207,#22208,#22209),
 .UNSPECIFIED.,.F.,.F.,(4,3,3,3,3,4),(114.407157784405,114.712345376808,
115.709844032258,116.707342687709,117.704841343159,118.70233999861),
 .UNSPECIFIED.);
#368=B_SPLINE_CURVE_WITH_KNOTS('',3,(#22217,#22218,#22219,#22220,#22221,
#22222,#22223,#22224,#22225,#22226,#22227,#22228,#22229,#22230,#22231,#22232,
#22233,#22234,#22235,#22236,#22237,#22238),.UNSPECIFIED.,.F.,.F.,(4,3,3,
3,3,3,3,4),(-116.687727133335,-115.709844032258,-114.712345376808,-113.714846721357,
-112.717348065907,-111.719849410456,-110.722350755006,-110.660533485745),
 .UNSPECIFIED.);
#369=B_SPLINE_CURVE_WITH_KNOTS('',3,(#22243,#22244,#22245,#22246,#22247,
#22248,#22249,#22250,#22251,#22252,#22253,#22254,#22255,#22256,#22257,#22258,
#22259,#22260,#22261,#22262,#22263,#22264),.UNSPECIFIED.,.F.,.F.,(4,3,3,
3,3,3,3,4),(108.123972477225,108.727353444105,109.724852099555,110.722350755006,
111.719849410456,112.717348065907,113.714846721357,114.407157784405),
 .UNSPECIFIED.);
#370=B_SPLINE_CURVE_WITH_KNOTS('',3,(#22265,#22266,#22267,#22268,#22269,
#22270,#22271,#22272,#22273,#22274,#22275,#22276,#22277,#22278,#22279,#22280,
#22281,#22282,#22283,#22284,#22285,#22286),.UNSPECIFIED.,.F.,.F.,(4,3,3,
3,3,3,3,4),(-110.660533485745,-109.724852099555,-108.727353444105,-107.729854788654,
-106.732356133204,-105.734857477753,-104.737358822303,-104.377348178566),
 .UNSPECIFIED.);
#371=B_SPLINE_CURVE_WITH_KNOTS('',3,(#22291,#22292,#22293,#22294,#22295,
#22296,#22297,#22298,#22299,#22300,#22301,#22302,#22303,#22304,#22305,#22306,
#22307,#22308,#22309,#22310,#22311,#22312),.UNSPECIFIED.,.F.,.F.,(4,3,3,
3,3,3,3,4),(101.840787170045,102.742361511402,103.739860166852,104.737358822303,
105.734857477753,106.732356133204,107.729854788654,108.123972477225),
 .UNSPECIFIED.);
#372=B_SPLINE_CURVE_WITH_KNOTS('',3,(#22313,#22314,#22315,#22316,#22317,
#22318,#22319,#22320,#22321,#22322,#22323,#22324,#22325,#22326,#22327,#22328,
#22329,#22330,#22331,#22332,#22333,#22334),.UNSPECIFIED.,.F.,.F.,(4,3,3,
3,3,3,3,4),(-104.377348178566,-103.739860166852,-102.742361511402,-101.744862855951,
-100.747364200501,-99.7498655450501,-98.7523668895996,-98.094162871386),
 .UNSPECIFIED.);
#373=B_SPLINE_CURVE_WITH_KNOTS('',3,(#22339,#22340,#22341,#22342,#22343,
#22344,#22345,#22346,#22347,#22348,#22349,#22350,#22351,#22352,#22353,#22354,
#22355,#22356,#22357,#22358,#22359,#22360,#22361,#22362,#22363),
 .UNSPECIFIED.,.F.,.F.,(4,3,3,3,3,3,3,3,4),(95.5576018628657,95.7598709232481,
96.7573695786986,97.7548682341491,98.7523668895996,99.7498655450501,100.747364200501,
101.744862855951,101.840787170045),.UNSPECIFIED.);
#374=B_SPLINE_CURVE_WITH_KNOTS('',3,(#22364,#22365,#22366,#22367,#22368,
#22369,#22370,#22371,#22372,#22373,#22374,#22375,#22376,#22377,#22378,#22379,
#22380,#22381,#22382,#22383,#22384,#22385),.UNSPECIFIED.,.F.,.F.,(4,3,3,
3,3,3,3,4),(-98.094162871386,-97.7548682341491,-96.7573695786986,-95.7598709232481,
-94.7623722677976,-93.7648736123471,-92.7673749568966,-91.8109775642064),
 .UNSPECIFIED.);
#375=B_SPLINE_CURVE_WITH_KNOTS('',3,(#22390,#22391,#22392,#22393,#22394,
#22395,#22396,#22397,#22398,#22399,#22400,#22401,#22402,#22403,#22404,#22405,
#22406,#22407,#22408,#22409,#22410,#22411),.UNSPECIFIED.,.F.,.F.,(4,3,3,
3,3,3,3,4),(89.2744165556862,89.7748789905451,90.7723776459956,91.7698763014461,
92.7673749568966,93.7648736123471,94.7623722677976,95.5576018628657),
 .UNSPECIFIED.);
#376=B_SPLINE_CURVE_WITH_KNOTS('',3,(#22412,#22413,#22414,#22415,#22416,
#22417,#22418,#22419,#22420,#22421,#22422,#22423,#22424,#22425,#22426,#22427,
#22428,#22429,#22430,#22431,#22432,#22433,#22434,#22435,#22436),
 .UNSPECIFIED.,.F.,.F.,(4,3,3,3,3,3,3,3,4),(-91.8109775642064,-91.7698763014461,
-90.7723776459956,-89.7748789905451,-88.7773803350946,-87.7798816796441,
-86.7823830241936,-85.7848843687431,-85.5277922570269),.UNSPECIFIED.);
#377=B_SPLINE_CURVE_WITH_KNOTS('',3,(#22441,#22442,#22443,#22444,#22445,
#22446,#22447,#22448,#22449,#22450,#22451,#22452,#22453,#22454,#22455,#22456,
#22457,#22458,#22459,#22460,#22461,#22462),.UNSPECIFIED.,.F.,.F.,(4,3,3,
3,3,3,3,4),(82.9912312485066,83.7898870578421,84.7873857132926,85.7848843687431,
86.7823830241936,87.7798816796441,88.7773803350946,89.2744165556862),
 .UNSPECIFIED.);
#378=B_SPLINE_CURVE_WITH_KNOTS('',3,(#22463,#22464,#22465,#22466,#22467,
#22468,#22469,#22470,#22471,#22472,#22473,#22474,#22475,#22476,#22477,#22478,
#22479,#22480,#22481,#22482,#22483,#22484),.UNSPECIFIED.,.F.,.F.,(4,3,3,
3,3,3,3,4),(-85.5277922570269,-84.7873857132926,-83.7898870578422,-82.7923884023916,
-81.7948897469411,-80.7973910914906,-79.7998924360401,-79.2446069498473),
 .UNSPECIFIED.);
#379=B_SPLINE_CURVE_WITH_KNOTS('',3,(#22489,#22490,#22491,#22492,#22493,
#22494,#22495,#22496,#22497,#22498,#22499,#22500,#22501,#22502,#22503,#22504,
#22505,#22506,#22507,#22508,#22509,#22510,#22511,#22512,#22513),
 .UNSPECIFIED.,.F.,.F.,(4,3,3,3,3,3,3,3,4),(76.708045941327,76.8073964696886,
77.8048951251391,78.8023937805896,79.7998924360401,80.7973910914906,81.7948897469411,
82.7923884023916,82.9912312485066),.UNSPECIFIED.);
#380=B_SPLINE_CURVE_WITH_KNOTS('',3,(#22514,#22515,#22516,#22517,#22518,
#22519,#22520,#22521,#22522,#22523,#22524,#22525,#22526,#22527,#22528,#22529,
#22530,#22531,#22532,#22533,#22534,#22535),.UNSPECIFIED.,.F.,.F.,(4,3,3,
3,3,3,3,4),(-79.2446069498473,-78.8023937805896,-77.8048951251391,-76.8073964696886,
-75.8098978142381,-74.8123991587876,-73.8149005033371,-72.9614216426677),
 .UNSPECIFIED.);
#381=B_SPLINE_CURVE_WITH_KNOTS('',3,(#22540,#22541,#22542,#22543,#22544,
#22545,#22546,#22547,#22548,#22549,#22550,#22551,#22552,#22553,#22554,#22555,
#22556,#22557,#22558,#22559,#22560,#22561),.UNSPECIFIED.,.F.,.F.,(4,3,3,
3,3,3,3,4),(70.4248606341474,70.8224045369856,71.8199031924361,72.8174018478866,
73.8149005033371,74.8123991587876,75.8098978142381,76.708045941327),
 .UNSPECIFIED.);
#382=B_SPLINE_CURVE_WITH_KNOTS('',3,(#22562,#22563,#22564,#22565,#22566,
#22567,#22568,#22569,#22570,#22571,#22572,#22573,#22574,#22575,#22576,#22577,
#22578,#22579,#22580,#22581,#22582,#22583,#22584,#22585,#22586),
 .UNSPECIFIED.,.F.,.F.,(4,3,3,3,3,3,3,3,4),(-72.9614216426677,-72.8174018478866,
-71.8199031924361,-70.8224045369856,-69.8249058815351,-68.8274072260846,
-67.8299085706341,-66.8324099151836,-66.6782363354882),.UNSPECIFIED.);
#383=B_SPLINE_CURVE_WITH_KNOTS('',3,(#22591,#22592,#22593,#22594,#22595,
#22596,#22597,#22598,#22599,#22600,#22601,#22602,#22603,#22604,#22605,#22606,
#22607,#22608,#22609,#22610,#22611,#22612),.UNSPECIFIED.,.F.,.F.,(4,3,3,
3,3,3,3,4),(64.1416753269678,64.8374126042826,65.8349112597331,66.8324099151836,
67.8299085706341,68.8274072260846,69.8249058815351,70.4248606341474),
 .UNSPECIFIED.);
#384=B_SPLINE_CURVE_WITH_KNOTS('',3,(#22613,#22614,#22615,#22616,#22617,
#22618,#22619,#22620,#22621,#22622,#22623,#22624,#22625,#22626,#22627,#22628,
#22629,#22630,#22631,#22632,#22633,#22634),.UNSPECIFIED.,.F.,.F.,(4,3,3,
3,3,3,3,4),(-66.6782363354882,-65.8349112597331,-64.8374126042826,-63.8399139488321,
-62.8424152933816,-61.8449166379311,-60.8474179824806,-60.3950510283085),
 .UNSPECIFIED.);
#385=B_SPLINE_CURVE_WITH_KNOTS('',3,(#22639,#22640,#22641,#22642,#22643,
#22644,#22645,#22646,#22647,#22648,#22649,#22650,#22651,#22652,#22653,#22654,
#22655,#22656,#22657,#22658,#22659,#22660),.UNSPECIFIED.,.F.,.F.,(4,3,3,
3,3,3,3,4),(57.8584900197882,58.8524206715796,59.8499193270301,60.8474179824806,
61.8449166379311,62.8424152933816,63.8399139488321,64.1416753269678),
 .UNSPECIFIED.);
#386=B_SPLINE_CURVE_WITH_KNOTS('',3,(#22661,#22662,#22663,#22664,#22665,
#22666,#22667,#22668,#22669,#22670,#22671,#22672,#22673,#22674,#22675,#22676,
#22677,#22678,#22679,#22680,#22681,#22682),.UNSPECIFIED.,.F.,.F.,(4,3,3,
3,3,3,3,4),(-60.3950510283085,-59.8499193270301,-58.8524206715796,-57.8549220161291,
-56.8574233606786,-55.8599247052281,-54.8624260497776,-54.1118657211289),
 .UNSPECIFIED.);
#387=B_SPLINE_CURVE_WITH_KNOTS('',3,(#22687,#22688,#22689,#22690,#22691,
#22692,#22693,#22694,#22695,#22696,#22697,#22698,#22699,#22700,#22701,#22702,
#22703,#22704,#22705,#22706,#22707,#22708,#22709,#22710,#22711),
 .UNSPECIFIED.,.F.,.F.,(4,3,3,3,3,3,3,3,4),(51.5753047126086,51.8699300834261,
52.8674287388766,53.8649273943271,54.8624260497776,55.8599247052281,56.8574233606786,
57.8549220161291,57.8584900197882),.UNSPECIFIED.);
#388=B_SPLINE_CURVE_WITH_KNOTS('',3,(#22712,#22713,#22714,#22715,#22716,
#22717,#22718,#22719,#22720,#22721,#22722,#22723,#22724,#22725,#22726,#22727,
#22728,#22729,#22730,#22731,#22732,#22733,#22734,#22735,#22736),
 .UNSPECIFIED.,.F.,.F.,(4,3,3,3,3,3,3,3,4),(-54.1118657211289,-53.8649273943271,
-52.8674287388766,-51.8699300834261,-50.8724314279756,-49.8749327725251,
-48.8774341170746,-47.8799354616241,-47.8286804139493),.UNSPECIFIED.);
#389=B_SPLINE_CURVE_WITH_KNOTS('',3,(#22741,#22742,#22743,#22744,#22745,
#22746,#22747,#22748,#22749,#22750,#22751,#22752,#22753,#22754,#22755,#22756,
#22757,#22758,#22759,#22760,#22761,#22762),.UNSPECIFIED.,.F.,.F.,(4,3,3,
3,3,3,3,4),(45.292119405429,45.8849381507231,46.8824368061736,47.8799354616241,
48.8774341170746,49.8749327725251,50.8724314279756,51.5753047126086),
 .UNSPECIFIED.);
#390=B_SPLINE_CURVE_WITH_KNOTS('',3,(#22763,#22764,#22765,#22766,#22767,
#22768,#22769,#22770,#22771,#22772,#22773,#22774,#22775,#22776,#22777,#22778,
#22779,#22780,#22781,#22782,#22783,#22784),.UNSPECIFIED.,.F.,.F.,(4,3,3,
3,3,3,3,4),(-47.8286804139493,-46.8824368061736,-45.8849381507231,-44.8874394952726,
-43.8899408398221,-42.8924421843716,-41.8949435289211,-41.5454951067697),
 .UNSPECIFIED.);
#391=B_SPLINE_CURVE_WITH_KNOTS('',3,(#22789,#22790,#22791,#22792,#22793,
#22794,#22795,#22796,#22797,#22798,#22799,#22800,#22801,#22802,#22803,#22804,
#22805,#22806,#22807,#22808,#22809,#22810),.UNSPECIFIED.,.F.,.F.,(4,3,3,
3,3,3,3,4),(39.0089340982494,39.8999462180201,40.8974448734706,41.8949435289211,
42.8924421843716,43.8899408398221,44.8874394952726,45.292119405429),
 .UNSPECIFIED.);
#392=B_SPLINE_CURVE_WITH_KNOTS('',3,(#22811,#22812,#22813,#22814,#22815,
#22816,#22817,#22818,#22819,#22820,#22821,#22822,#22823,#22824,#22825,#22826,
#22827,#22828,#22829,#22830,#22831,#22832),.UNSPECIFIED.,.F.,.F.,(4,3,3,
3,3,3,3,4),(-41.5454951067697,-40.8974448734706,-39.8999462180201,-38.9024475625696,
-37.9049489071191,-36.9074502516685,-35.909951596218,-35.2623097995902),
 .UNSPECIFIED.);
#393=B_SPLINE_CURVE_WITH_KNOTS('',3,(#22837,#22838,#22839,#22840,#22841,
#22842,#22843,#22844,#22845,#22846,#22847,#22848,#22849,#22850,#22851,#22852,
#22853,#22854,#22855,#22856,#22857,#22858,#22859,#22860,#22861),
 .UNSPECIFIED.,.F.,.F.,(4,3,3,3,3,3,3,3,4),(32.7257487910699,32.9174556298666,
33.9149542853171,34.9124529407676,35.9099515962181,36.9074502516685,37.9049489071191,
38.9024475625696,39.0089340982494),.UNSPECIFIED.);
#394=B_SPLINE_CURVE_WITH_KNOTS('',3,(#22862,#22863,#22864,#22865,#22866,
#22867,#22868,#22869,#22870,#22871,#22872,#22873,#22874,#22875,#22876,#22877,
#22878,#22879,#22880,#22881,#22882,#22883),.UNSPECIFIED.,.F.,.F.,(4,3,3,
3,3,3,3,4),(-35.2623097995902,-34.9124529407676,-33.9149542853171,-32.9174556298665,
-31.919956974416,-30.9224583189655,-29.9249596635151,-28.9791244924106),
 .UNSPECIFIED.);
#395=B_SPLINE_CURVE_WITH_KNOTS('',3,(#22888,#22889,#22890,#22891,#22892,
#22893,#22894,#22895,#22896,#22897,#22898,#22899,#22900,#22901,#22902,#22903,
#22904,#22905,#22906,#22907,#22908,#22909),.UNSPECIFIED.,.F.,.F.,(4,3,3,
3,3,3,3,4),(26.4425634838902,26.9324636971635,27.929962352614,28.9274610080645,
29.924959663515,30.9224583189655,31.9199569744161,32.7257487910699),
 .UNSPECIFIED.);
#396=B_SPLINE_CURVE_WITH_KNOTS('',3,(#22910,#22911,#22912,#22913,#22914,
#22915,#22916,#22917,#22918,#22919,#22920,#22921,#22922,#22923,#22924,#22925,
#22926,#22927,#22928,#22929,#22930,#22931,#22932,#22933,#22934),
 .UNSPECIFIED.,.F.,.F.,(4,3,3,3,3,3,3,3,4),(-28.9791244924106,-28.9274610080645,
-27.929962352614,-26.9324636971635,-25.934965041713,-24.9374663862625,-23.939967730812,
-22.9424690753615,-22.6959391852309),.UNSPECIFIED.);
#397=B_SPLINE_CURVE_WITH_KNOTS('',3,(#22939,#22940,#22941,#22942,#22943,
#22944,#22945,#22946,#22947,#22948,#22949,#22950,#22951,#22952,#22953,#22954,
#22955,#22956,#22957,#22958,#22959,#22960),.UNSPECIFIED.,.F.,.F.,(4,3,3,
3,3,3,3,4),(20.1593781767106,20.9474717644605,21.944970419911,22.9424690753615,
23.939967730812,24.9374663862625,25.934965041713,26.4425634838902),
 .UNSPECIFIED.);
#398=B_SPLINE_CURVE_WITH_KNOTS('',3,(#22961,#22962,#22963,#22964,#22965,
#22966,#22967,#22968,#22969,#22970,#22971,#22972,#22973,#22974,#22975,#22976,
#22977,#22978,#22979,#22980,#22981,#22982),.UNSPECIFIED.,.F.,.F.,(4,3,3,
3,3,3,3,4),(-22.6959391852309,-21.944970419911,-20.9474717644605,-19.94997310901,
-18.9524744535595,-17.954975798109,-16.9574771426585,-16.4127538780514),
 .UNSPECIFIED.);
#399=B_SPLINE_CURVE_WITH_KNOTS('',3,(#22987,#22988,#22989,#22990,#22991,
#22992,#22993,#22994,#22995,#22996,#22997,#22998,#22999,#23000,#23001,#23002,
#23003,#23004,#23005,#23006,#23007,#23008,#23009,#23010,#23011),
 .UNSPECIFIED.,.F.,.F.,(4,3,3,3,3,3,3,3,4),(13.8761928695311,13.964981176307,
14.9624798317575,15.959978487208,16.9574771426585,17.954975798109,18.9524744535595,
19.94997310901,20.1593781767106),.UNSPECIFIED.);
#400=B_SPLINE_CURVE_WITH_KNOTS('',3,(#23012,#23013,#23014,#23015,#23016,
#23017,#23018,#23019,#23020,#23021,#23022,#23023,#23024,#23025,#23026,#23027,
#23028,#23029,#23030,#23031,#23032,#23033),.UNSPECIFIED.,.F.,.F.,(4,3,3,
3,3,3,3,4),(-16.4127538780514,-15.959978487208,-14.9624798317575,-13.964981176307,
-12.9674825208565,-11.969983865406,-10.9724852099555,-10.1295685708718),
 .UNSPECIFIED.);
#401=B_SPLINE_CURVE_WITH_KNOTS('',3,(#23039,#23040,#23041,#23042,#23043,
#23044,#23045,#23046,#23047,#23048,#23049,#23050,#23051),.UNSPECIFIED.,
 .F.,.F.,(4,3,3,3,4),(-3.84638326369218,-2.9924959663515,-1.994997310901,
-0.997498655450501,0.),.UNSPECIFIED.);
#402=B_SPLINE_CURVE_WITH_KNOTS('',3,(#23054,#23055,#23056,#23057,#23058,
#23059,#23060,#23061,#23062,#23063,#23064,#23065,#23066,#23067,#23068,#23069,
#23070,#23071,#23072),.UNSPECIFIED.,.F.,.F.,(4,3,3,3,3,3,4),(2.01461286527449,
2.99249596635151,3.98999462180201,4.98749327725251,5.98499193270301,6.98249058815351,
7.59300756235149),.UNSPECIFIED.);
#403=B_SPLINE_CURVE_WITH_KNOTS('',3,(#23078,#23079,#23080,#23081,#23082),
 .UNSPECIFIED.,.F.,.F.,(4,1,4),(128.805298797182,129.566421347416,130.563920002866),
 .UNSPECIFIED.);
#404=B_SPLINE_CURVE_WITH_KNOTS('',3,(#23085,#23086,#23087,#23088,#23089,
#23090),.UNSPECIFIED.,.F.,.F.,(4,1,1,4),(128.805298797182,129.110486389585,
130.107985045035,131.085868146112),.UNSPECIFIED.);
#405=B_SPLINE_CURVE_WITH_KNOTS('',3,(#23095,#23096,#23097,#23098,#23099,
#23100,#23101,#23102,#23103,#23104,#23105),.UNSPECIFIED.,.F.,.F.,(4,1,1,
1,1,1,1,1,4),(122.522113490002,122.583930759262,123.581429414713,124.578928070163,
125.576426725614,126.573925381064,127.571424036515,128.568922691965,128.805298797182),
 .UNSPECIFIED.);
#406=B_SPLINE_CURVE_WITH_KNOTS('',3,(#23106,#23107,#23108,#23109,#23110,
#23111,#23112,#23113,#23114,#23115),.UNSPECIFIED.,.F.,.F.,(4,1,1,1,1,1,
1,4),(122.522113490002,123.125494456882,124.122993112332,125.120491767783,
126.117990423233,127.115489078684,128.112987734134,128.805298797182),
 .UNSPECIFIED.);
#407=B_SPLINE_CURVE_WITH_KNOTS('',3,(#23120,#23121,#23122,#23123,#23124,
#23125,#23126,#23127,#23128,#23129),.UNSPECIFIED.,.F.,.F.,(4,1,1,1,1,1,
1,4),(116.238928182822,116.598938826559,117.59643748201,118.59393613746,
119.591434792911,120.588933448361,121.586432103812,122.522113490002),
 .UNSPECIFIED.);
#408=B_SPLINE_CURVE_WITH_KNOTS('',3,(#23130,#23131,#23132,#23133,#23134,
#23135,#23136,#23137,#23138,#23139),.UNSPECIFIED.,.F.,.F.,(4,1,1,1,1,1,
1,4),(116.238928182822,117.140502524179,118.138001179629,119.13549983508,
120.13299849053,121.130497145981,122.127995801431,122.522113490002),
 .UNSPECIFIED.);
#409=B_SPLINE_CURVE_WITH_KNOTS('',3,(#23144,#23145,#23146,#23147,#23148,
#23149,#23150,#23151,#23152,#23153),.UNSPECIFIED.,.F.,.F.,(4,1,1,1,1,1,
1,4),(109.955742875643,110.613946893856,111.611445549307,112.608944204757,
113.606442860208,114.603941515658,115.601440171109,116.238928182822),
 .UNSPECIFIED.);
#410=B_SPLINE_CURVE_WITH_KNOTS('',3,(#23154,#23155,#23156,#23157,#23158,
#23159,#23160,#23161,#23162,#23163,#23164),.UNSPECIFIED.,.F.,.F.,(4,1,1,
1,1,1,1,1,4),(109.955742875643,110.158011936025,111.155510591476,112.153009246926,
113.150507902377,114.148006557827,115.145505213278,116.143003868728,116.238928182822),
 .UNSPECIFIED.);
#411=B_SPLINE_CURVE_WITH_KNOTS('',3,(#23169,#23170,#23171,#23172,#23173,
#23174,#23175,#23176,#23177,#23178),.UNSPECIFIED.,.F.,.F.,(4,1,1,1,1,1,
1,4),(103.672557568463,104.628954961153,105.626453616604,106.623952272054,
107.621450927505,108.618949582955,109.616448238406,109.955742875643),
 .UNSPECIFIED.);
#412=B_SPLINE_CURVE_WITH_KNOTS('',3,(#23179,#23180,#23181,#23182,#23183,
#23184,#23185,#23186,#23187,#23188),.UNSPECIFIED.,.F.,.F.,(4,1,1,1,1,1,
1,4),(103.672557568463,104.173020003322,105.170518658772,106.168017314223,
107.165515969673,108.163014625124,109.160513280574,109.955742875643),
 .UNSPECIFIED.);
#413=B_SPLINE_CURVE_WITH_KNOTS('',3,(#23193,#23194,#23195,#23196,#23197,
#23198,#23199,#23200,#23201,#23202,#23203),.UNSPECIFIED.,.F.,.F.,(4,1,1,
1,1,1,1,1,4),(97.3893722612835,97.6464643729998,98.6439630284503,99.6414616839008,
100.638960339351,101.636458994802,102.633957650252,103.631456305703,103.672557568463),
 .UNSPECIFIED.);
#414=B_SPLINE_CURVE_WITH_KNOTS('',3,(#23204,#23205,#23206,#23207,#23208,
#23209,#23210,#23211,#23212,#23213),.UNSPECIFIED.,.F.,.F.,(4,1,1,1,1,1,
1,4),(97.3893722612835,98.188028070619,99.1855267260695,100.18302538152,
101.18052403697,102.178022692421,103.175521347871,103.672557568463),
 .UNSPECIFIED.);
#415=B_SPLINE_CURVE_WITH_KNOTS('',3,(#23218,#23219,#23220,#23221,#23222,
#23223,#23224,#23225,#23226,#23227),.UNSPECIFIED.,.F.,.F.,(4,1,1,1,1,1,
1,4),(91.1061869541039,91.6614724402968,92.6589710957473,93.6564697511978,
94.6539684066483,95.6514670620988,96.6489657175493,97.3893722612835),
 .UNSPECIFIED.);
#416=B_SPLINE_CURVE_WITH_KNOTS('',3,(#23228,#23229,#23230,#23231,#23232,
#23233,#23234,#23235,#23236,#23237,#23238),.UNSPECIFIED.,.F.,.F.,(4,1,1,
1,1,1,1,1,4),(91.106186954104,91.2055374824655,92.203036137916,93.2005347933665,
94.198033448817,95.1955321042675,96.193030759718,97.1905294151685,97.3893722612835),
 .UNSPECIFIED.);
#417=B_SPLINE_CURVE_WITH_KNOTS('',3,(#23243,#23244,#23245,#23246,#23247,
#23248,#23249,#23250,#23251,#23252),.UNSPECIFIED.,.F.,.F.,(4,1,1,1,1,1,
1,4),(84.8230016469243,85.6764805075938,86.6739791630443,87.6714778184948,
88.6689764739453,89.6664751293958,90.6639737848463,91.1061869541039),
 .UNSPECIFIED.);
#418=B_SPLINE_CURVE_WITH_KNOTS('',3,(#23253,#23254,#23255,#23256,#23257,
#23258,#23259,#23260,#23261,#23262),.UNSPECIFIED.,.F.,.F.,(4,1,1,1,1,1,
1,4),(84.8230016469244,85.2205455497625,86.218044205213,87.2155428606635,
88.213041516114,89.2105401715645,90.208038827015,91.106186954104),
 .UNSPECIFIED.);
#419=B_SPLINE_CURVE_WITH_KNOTS('',3,(#23267,#23268,#23269,#23270,#23271,
#23272,#23273,#23274,#23275,#23276,#23277),.UNSPECIFIED.,.F.,.F.,(4,1,1,
1,1,1,1,1,4),(78.5398163397448,78.6939899194402,79.6914885748908,80.6889872303413,
81.6864858857918,82.6839845412423,83.6814831966928,84.6789818521433,84.8230016469243),
 .UNSPECIFIED.);
#420=B_SPLINE_CURVE_WITH_KNOTS('',3,(#23278,#23279,#23280,#23281,#23282,
#23283,#23284,#23285,#23286,#23287),.UNSPECIFIED.,.F.,.F.,(4,1,1,1,1,1,
1,4),(78.5398163397448,79.2355536170595,80.23305227251,81.2305509279605,
82.228049583411,83.2255482388615,84.223046894312,84.8230016469244),
 .UNSPECIFIED.);
#421=B_SPLINE_CURVE_WITH_KNOTS('',3,(#23292,#23293,#23294,#23295,#23296,
#23297,#23298,#23299,#23300,#23301),.UNSPECIFIED.,.F.,.F.,(4,1,1,1,1,1,
1,4),(72.2566310325652,72.7089979867372,73.7064966421877,74.7039952976382,
75.7014939530887,76.6989926085392,77.6964912639897,78.5398163397448),
 .UNSPECIFIED.);
#422=B_SPLINE_CURVE_WITH_KNOTS('',3,(#23302,#23303,#23304,#23305,#23306,
#23307,#23308,#23309,#23310,#23311),.UNSPECIFIED.,.F.,.F.,(4,1,1,1,1,1,
1,4),(72.2566310325652,73.2505616843565,74.248060339807,75.2455589952575,
76.243057650708,77.2405563061585,78.238054961609,78.5398163397448),
 .UNSPECIFIED.);
#423=B_SPLINE_CURVE_WITH_KNOTS('',3,(#23316,#23317,#23318,#23319,#23320,
#23321,#23322,#23323,#23324,#23325),.UNSPECIFIED.,.F.,.F.,(4,1,1,1,1,1,
1,4),(65.9734457253856,66.7240060540342,67.7215047094847,68.7190033649352,
69.7165020203857,70.7140006758362,71.7114993312867,72.2566310325652),
 .UNSPECIFIED.);
#424=B_SPLINE_CURVE_WITH_KNOTS('',3,(#23326,#23327,#23328,#23329,#23330,
#23331,#23332,#23333,#23334,#23335,#23336),.UNSPECIFIED.,.F.,.F.,(4,1,1,
1,1,1,1,1,4),(65.9734457253856,66.2680710962029,67.2655697516534,68.2630684071039,
69.2605670625544,70.2580657180049,71.2555643734554,72.2530630289059,72.2566310325652),
 .UNSPECIFIED.);
#425=B_SPLINE_CURVE_WITH_KNOTS('',3,(#23341,#23342,#23343,#23344,#23345,
#23346,#23347,#23348,#23349,#23350,#23351),.UNSPECIFIED.,.F.,.F.,(4,1,1,
1,1,1,1,1,4),(59.690260418206,59.7415154658807,60.7390141213312,61.7365127767817,
62.7340114322322,63.7315100876827,64.7290087431332,65.7265073985837,65.9734457253856),
 .UNSPECIFIED.);
#426=B_SPLINE_CURVE_WITH_KNOTS('',3,(#23352,#23353,#23354,#23355,#23356,
#23357,#23358,#23359,#23360,#23361),.UNSPECIFIED.,.F.,.F.,(4,1,1,1,1,1,
1,4),(59.690260418206,60.2830791634999,61.2805778189504,62.2780764744009,
63.2755751298514,64.2730737853019,65.2705724407524,65.9734457253856),
 .UNSPECIFIED.);
#427=B_SPLINE_CURVE_WITH_KNOTS('',3,(#23366,#23367,#23368,#23369,#23370,
#23371,#23372,#23373,#23374,#23375),.UNSPECIFIED.,.F.,.F.,(4,1,1,1,1,1,
1,4),(53.4070751110263,53.7565235331777,54.7540221886282,55.7515208440787,
56.7490194995292,57.7465181549797,58.7440168104302,59.690260418206),
 .UNSPECIFIED.);
#428=B_SPLINE_CURVE_WITH_KNOTS('',3,(#23376,#23377,#23378,#23379,#23380,
#23381,#23382,#23383,#23384,#23385),.UNSPECIFIED.,.F.,.F.,(4,1,1,1,1,1,
1,4),(53.4070751110264,54.2980872307969,55.2955858862474,56.2930845416979,
57.2905831971484,58.2880818525989,59.2855805080494,59.690260418206),
 .UNSPECIFIED.);
#429=B_SPLINE_CURVE_WITH_KNOTS('',3,(#23390,#23391,#23392,#23393,#23394,
#23395,#23396,#23397,#23398,#23399),.UNSPECIFIED.,.F.,.F.,(4,1,1,1,1,1,
1,4),(47.1238898038468,47.7715316004747,48.7690302559252,49.7665289113757,
50.7640275668262,51.7615262222767,52.7590248777272,53.4070751110263),
 .UNSPECIFIED.);
#430=B_SPLINE_CURVE_WITH_KNOTS('',3,(#23400,#23401,#23402,#23403,#23404,
#23405,#23406,#23407,#23408,#23409,#23410),.UNSPECIFIED.,.F.,.F.,(4,1,1,
1,1,1,1,1,4),(47.1238898038468,47.3155966426434,48.3130952980939,49.3105939535444,
50.3080926089949,51.3055912644454,52.3030899198959,53.3005885753464,53.4070751110264),
 .UNSPECIFIED.);
#431=B_SPLINE_CURVE_WITH_KNOTS('',3,(#23415,#23416,#23417,#23418,#23419,
#23420,#23421,#23422,#23423,#23424),.UNSPECIFIED.,.F.,.F.,(4,1,1,1,1,1,
1,4),(40.8407044966672,41.7865396677717,42.7840383232222,43.7815369786727,
44.7790356341232,45.7765342895737,46.7740329450242,47.1238898038468),
 .UNSPECIFIED.);
#432=B_SPLINE_CURVE_WITH_KNOTS('',3,(#23425,#23426,#23427,#23428,#23429,
#23430,#23431,#23432,#23433,#23434),.UNSPECIFIED.,.F.,.F.,(4,1,1,1,1,1,
1,4),(40.8407044966672,41.3306047099404,42.3281033653909,43.3256020208414,
44.3231006762919,45.3205993317424,46.3180979871929,47.1238898038468),
 .UNSPECIFIED.);
#433=B_SPLINE_CURVE_WITH_KNOTS('',3,(#23439,#23440,#23441,#23442,#23443,
#23444,#23445,#23446,#23447,#23448,#23449),.UNSPECIFIED.,.F.,.F.,(4,1,1,
1,1,1,1,1,4),(34.5575191894876,34.8040490796182,35.8015477350687,36.7990463905192,
37.7965450459697,38.7940437014202,39.7915423568707,40.7890410123212,40.8407044966672),
 .UNSPECIFIED.);
#434=B_SPLINE_CURVE_WITH_KNOTS('',3,(#23450,#23451,#23452,#23453,#23454,
#23455,#23456,#23457,#23458,#23459),.UNSPECIFIED.,.F.,.F.,(4,1,1,1,1,1,
1,4),(34.5575191894877,35.3456127772374,36.3431114326879,37.3406100881384,
38.3381087435889,39.3356073990394,40.3331060544899,40.8407044966672),
 .UNSPECIFIED.);
#435=B_SPLINE_CURVE_WITH_KNOTS('',3,(#23464,#23465,#23466,#23467,#23468,
#23469,#23470,#23471,#23472,#23473),.UNSPECIFIED.,.F.,.F.,(4,1,1,1,1,1,
1,4),(28.2743338823081,28.8190571469152,29.8165558023657,30.8140544578162,
31.8115531132667,32.8090517687172,33.8065504241677,34.5575191894876),
 .UNSPECIFIED.);
#436=B_SPLINE_CURVE_WITH_KNOTS('',3,(#23474,#23475,#23476,#23477,#23478,
#23479,#23480,#23481,#23482,#23483,#23484),.UNSPECIFIED.,.F.,.F.,(4,1,1,
1,1,1,1,1,4),(28.2743338823081,28.3631221890839,29.3606208445344,30.3581194999849,
31.3556181554354,32.3531168108859,33.3506154663364,34.3481141217869,34.5575191894877),
 .UNSPECIFIED.);
#437=B_SPLINE_CURVE_WITH_KNOTS('',3,(#23489,#23490,#23491,#23492,#23493,
#23494,#23495,#23496,#23497,#23498),.UNSPECIFIED.,.F.,.F.,(4,1,1,1,1,1,
1,4),(21.9911485751284,22.8340652142122,23.8315638696627,24.8290625251132,
25.8265611805637,26.8240598360142,27.8215584914647,28.2743338823081),
 .UNSPECIFIED.);
#438=B_SPLINE_CURVE_WITH_KNOTS('',3,(#23499,#23500,#23501,#23502,#23503,
#23504,#23505,#23506,#23507,#23508),.UNSPECIFIED.,.F.,.F.,(4,1,1,1,1,1,
1,4),(21.9911485751284,22.3781302563809,23.3756289118314,24.3731275672819,
25.3706262227324,26.3681248781829,27.3656235336334,28.2743338823081),
 .UNSPECIFIED.);
#439=B_SPLINE_CURVE_WITH_KNOTS('',3,(#23514,#23515,#23516,#23517,#23518),
 .UNSPECIFIED.,.F.,.F.,(4,1,4),(14.3981410127769,15.3956396682274,15.7079632679489),
 .UNSPECIFIED.);
#440=B_SPLINE_CURVE_WITH_KNOTS('',3,(#23521,#23522,#23523,#23524,#23525),
 .UNSPECIFIED.,.F.,.F.,(4,1,4),(13.8761928695311,14.8540759706082,15.7079632679488),
 .UNSPECIFIED.);
#441=B_SPLINE_CURVE_WITH_KNOTS('',3,(#23531,#23532,#23533,#23534,#23535,
#23536,#23537,#23538,#23539,#23540,#23541,#23542,#23543,#23544,#23545,#23546),
 .UNSPECIFIED.,.F.,.F.,(4,3,3,3,3,4),(114.407157784405,114.712345376808,
115.709844032258,116.707342687709,117.704841343159,118.70233999861),
 .UNSPECIFIED.);
#442=B_SPLINE_CURVE_WITH_KNOTS('',3,(#23554,#23555,#23556,#23557,#23558,
#23559,#23560,#23561,#23562,#23563,#23564,#23565,#23566,#23567,#23568,#23569,
#23570,#23571,#23572,#23573,#23574,#23575),.UNSPECIFIED.,.F.,.F.,(4,3,3,
3,3,3,3,4),(-116.687727133335,-115.709844032258,-114.712345376808,-113.714846721357,
-112.717348065907,-111.719849410456,-110.722350755006,-110.660533485745),
 .UNSPECIFIED.);
#443=B_SPLINE_CURVE_WITH_KNOTS('',3,(#23580,#23581,#23582,#23583,#23584,
#23585,#23586,#23587,#23588,#23589,#23590,#23591,#23592,#23593,#23594,#23595,
#23596,#23597,#23598,#23599,#23600,#23601),.UNSPECIFIED.,.F.,.F.,(4,3,3,
3,3,3,3,4),(108.123972477225,108.727353444105,109.724852099555,110.722350755006,
111.719849410456,112.717348065907,113.714846721357,114.407157784405),
 .UNSPECIFIED.);
#444=B_SPLINE_CURVE_WITH_KNOTS('',3,(#23602,#23603,#23604,#23605,#23606,
#23607,#23608,#23609,#23610,#23611,#23612,#23613,#23614,#23615,#23616,#23617,
#23618,#23619,#23620,#23621,#23622,#23623),.UNSPECIFIED.,.F.,.F.,(4,3,3,
3,3,3,3,4),(-110.660533485745,-109.724852099555,-108.727353444105,-107.729854788654,
-106.732356133204,-105.734857477753,-104.737358822303,-104.377348178566),
 .UNSPECIFIED.);
#445=B_SPLINE_CURVE_WITH_KNOTS('',3,(#23628,#23629,#23630,#23631,#23632,
#23633,#23634,#23635,#23636,#23637,#23638,#23639,#23640,#23641,#23642,#23643,
#23644,#23645,#23646,#23647,#23648,#23649),.UNSPECIFIED.,.F.,.F.,(4,3,3,
3,3,3,3,4),(101.840787170045,102.742361511402,103.739860166852,104.737358822303,
105.734857477753,106.732356133204,107.729854788654,108.123972477225),
 .UNSPECIFIED.);
#446=B_SPLINE_CURVE_WITH_KNOTS('',3,(#23650,#23651,#23652,#23653,#23654,
#23655,#23656,#23657,#23658,#23659,#23660,#23661,#23662,#23663,#23664,#23665,
#23666,#23667,#23668,#23669,#23670,#23671),.UNSPECIFIED.,.F.,.F.,(4,3,3,
3,3,3,3,4),(-104.377348178566,-103.739860166852,-102.742361511402,-101.744862855951,
-100.747364200501,-99.7498655450501,-98.7523668895996,-98.094162871386),
 .UNSPECIFIED.);
#447=B_SPLINE_CURVE_WITH_KNOTS('',3,(#23676,#23677,#23678,#23679,#23680,
#23681,#23682,#23683,#23684,#23685,#23686,#23687,#23688,#23689,#23690,#23691,
#23692,#23693,#23694,#23695,#23696,#23697,#23698,#23699,#23700),
 .UNSPECIFIED.,.F.,.F.,(4,3,3,3,3,3,3,3,4),(95.5576018628657,95.7598709232481,
96.7573695786986,97.7548682341491,98.7523668895996,99.7498655450501,100.747364200501,
101.744862855951,101.840787170045),.UNSPECIFIED.);
#448=B_SPLINE_CURVE_WITH_KNOTS('',3,(#23701,#23702,#23703,#23704,#23705,
#23706,#23707,#23708,#23709,#23710,#23711,#23712,#23713,#23714,#23715,#23716,
#23717,#23718,#23719,#23720,#23721,#23722),.UNSPECIFIED.,.F.,.F.,(4,3,3,
3,3,3,3,4),(-98.094162871386,-97.7548682341491,-96.7573695786986,-95.7598709232481,
-94.7623722677976,-93.7648736123471,-92.7673749568966,-91.8109775642064),
 .UNSPECIFIED.);
#449=B_SPLINE_CURVE_WITH_KNOTS('',3,(#23727,#23728,#23729,#23730,#23731,
#23732,#23733,#23734,#23735,#23736,#23737,#23738,#23739,#23740,#23741,#23742,
#23743,#23744,#23745,#23746,#23747,#23748),.UNSPECIFIED.,.F.,.F.,(4,3,3,
3,3,3,3,4),(89.2744165556862,89.7748789905451,90.7723776459956,91.7698763014461,
92.7673749568966,93.7648736123471,94.7623722677976,95.5576018628657),
 .UNSPECIFIED.);
#450=B_SPLINE_CURVE_WITH_KNOTS('',3,(#23749,#23750,#23751,#23752,#23753,
#23754,#23755,#23756,#23757,#23758,#23759,#23760,#23761,#23762,#23763,#23764,
#23765,#23766,#23767,#23768,#23769,#23770,#23771,#23772,#23773),
 .UNSPECIFIED.,.F.,.F.,(4,3,3,3,3,3,3,3,4),(-91.8109775642064,-91.7698763014461,
-90.7723776459956,-89.7748789905451,-88.7773803350946,-87.7798816796441,
-86.7823830241936,-85.7848843687431,-85.5277922570269),.UNSPECIFIED.);
#451=B_SPLINE_CURVE_WITH_KNOTS('',3,(#23778,#23779,#23780,#23781,#23782,
#23783,#23784,#23785,#23786,#23787,#23788,#23789,#23790,#23791,#23792,#23793,
#23794,#23795,#23796,#23797,#23798,#23799),.UNSPECIFIED.,.F.,.F.,(4,3,3,
3,3,3,3,4),(82.9912312485066,83.7898870578421,84.7873857132926,85.7848843687431,
86.7823830241936,87.7798816796441,88.7773803350946,89.2744165556862),
 .UNSPECIFIED.);
#452=B_SPLINE_CURVE_WITH_KNOTS('',3,(#23800,#23801,#23802,#23803,#23804,
#23805,#23806,#23807,#23808,#23809,#23810,#23811,#23812,#23813,#23814,#23815,
#23816,#23817,#23818,#23819,#23820,#23821),.UNSPECIFIED.,.F.,.F.,(4,3,3,
3,3,3,3,4),(-85.5277922570269,-84.7873857132926,-83.7898870578422,-82.7923884023916,
-81.7948897469411,-80.7973910914906,-79.7998924360401,-79.2446069498473),
 .UNSPECIFIED.);
#453=B_SPLINE_CURVE_WITH_KNOTS('',3,(#23826,#23827,#23828,#23829,#23830,
#23831,#23832,#23833,#23834,#23835,#23836,#23837,#23838,#23839,#23840,#23841,
#23842,#23843,#23844,#23845,#23846,#23847,#23848,#23849,#23850),
 .UNSPECIFIED.,.F.,.F.,(4,3,3,3,3,3,3,3,4),(76.708045941327,76.8073964696886,
77.8048951251391,78.8023937805896,79.7998924360401,80.7973910914906,81.7948897469411,
82.7923884023916,82.9912312485066),.UNSPECIFIED.);
#454=B_SPLINE_CURVE_WITH_KNOTS('',3,(#23851,#23852,#23853,#23854,#23855,
#23856,#23857,#23858,#23859,#23860,#23861,#23862,#23863,#23864,#23865,#23866,
#23867,#23868,#23869,#23870,#23871,#23872),.UNSPECIFIED.,.F.,.F.,(4,3,3,
3,3,3,3,4),(-79.2446069498473,-78.8023937805896,-77.8048951251391,-76.8073964696886,
-75.8098978142381,-74.8123991587876,-73.8149005033371,-72.9614216426677),
 .UNSPECIFIED.);
#455=B_SPLINE_CURVE_WITH_KNOTS('',3,(#23877,#23878,#23879,#23880,#23881,
#23882,#23883,#23884,#23885,#23886,#23887,#23888,#23889,#23890,#23891,#23892,
#23893,#23894,#23895,#23896,#23897,#23898),.UNSPECIFIED.,.F.,.F.,(4,3,3,
3,3,3,3,4),(70.4248606341474,70.8224045369856,71.8199031924361,72.8174018478866,
73.8149005033371,74.8123991587876,75.8098978142381,76.708045941327),
 .UNSPECIFIED.);
#456=B_SPLINE_CURVE_WITH_KNOTS('',3,(#23899,#23900,#23901,#23902,#23903,
#23904,#23905,#23906,#23907,#23908,#23909,#23910,#23911,#23912,#23913,#23914,
#23915,#23916,#23917,#23918,#23919,#23920,#23921,#23922,#23923),
 .UNSPECIFIED.,.F.,.F.,(4,3,3,3,3,3,3,3,4),(-72.9614216426677,-72.8174018478866,
-71.8199031924361,-70.8224045369856,-69.8249058815351,-68.8274072260846,
-67.8299085706341,-66.8324099151836,-66.6782363354882),.UNSPECIFIED.);
#457=B_SPLINE_CURVE_WITH_KNOTS('',3,(#23928,#23929,#23930,#23931,#23932,
#23933,#23934,#23935,#23936,#23937,#23938,#23939,#23940,#23941,#23942,#23943,
#23944,#23945,#23946,#23947,#23948,#23949),.UNSPECIFIED.,.F.,.F.,(4,3,3,
3,3,3,3,4),(64.1416753269678,64.8374126042826,65.8349112597331,66.8324099151836,
67.8299085706341,68.8274072260846,69.8249058815351,70.4248606341474),
 .UNSPECIFIED.);
#458=B_SPLINE_CURVE_WITH_KNOTS('',3,(#23950,#23951,#23952,#23953,#23954,
#23955,#23956,#23957,#23958,#23959,#23960,#23961,#23962,#23963,#23964,#23965,
#23966,#23967,#23968,#23969,#23970,#23971),.UNSPECIFIED.,.F.,.F.,(4,3,3,
3,3,3,3,4),(-66.6782363354882,-65.8349112597331,-64.8374126042826,-63.8399139488321,
-62.8424152933816,-61.8449166379311,-60.8474179824806,-60.3950510283085),
 .UNSPECIFIED.);
#459=B_SPLINE_CURVE_WITH_KNOTS('',3,(#23976,#23977,#23978,#23979,#23980,
#23981,#23982,#23983,#23984,#23985,#23986,#23987,#23988,#23989,#23990,#23991,
#23992,#23993,#23994,#23995,#23996,#23997),.UNSPECIFIED.,.F.,.F.,(4,3,3,
3,3,3,3,4),(57.8584900197882,58.8524206715796,59.8499193270301,60.8474179824806,
61.8449166379311,62.8424152933816,63.8399139488321,64.1416753269678),
 .UNSPECIFIED.);
#460=B_SPLINE_CURVE_WITH_KNOTS('',3,(#23998,#23999,#24000,#24001,#24002,
#24003,#24004,#24005,#24006,#24007,#24008,#24009,#24010,#24011,#24012,#24013,
#24014,#24015,#24016,#24017,#24018,#24019),.UNSPECIFIED.,.F.,.F.,(4,3,3,
3,3,3,3,4),(-60.3950510283085,-59.8499193270301,-58.8524206715796,-57.8549220161291,
-56.8574233606786,-55.8599247052281,-54.8624260497776,-54.1118657211289),
 .UNSPECIFIED.);
#461=B_SPLINE_CURVE_WITH_KNOTS('',3,(#24024,#24025,#24026,#24027,#24028,
#24029,#24030,#24031,#24032,#24033,#24034,#24035,#24036,#24037,#24038,#24039,
#24040,#24041,#24042,#24043,#24044,#24045,#24046,#24047,#24048),
 .UNSPECIFIED.,.F.,.F.,(4,3,3,3,3,3,3,3,4),(51.5753047126086,51.8699300834261,
52.8674287388766,53.8649273943271,54.8624260497776,55.8599247052281,56.8574233606786,
57.8549220161291,57.8584900197882),.UNSPECIFIED.);
#462=B_SPLINE_CURVE_WITH_KNOTS('',3,(#24049,#24050,#24051,#24052,#24053,
#24054,#24055,#24056,#24057,#24058,#24059,#24060,#24061,#24062,#24063,#24064,
#24065,#24066,#24067,#24068,#24069,#24070,#24071,#24072,#24073),
 .UNSPECIFIED.,.F.,.F.,(4,3,3,3,3,3,3,3,4),(-54.1118657211289,-53.8649273943271,
-52.8674287388766,-51.8699300834261,-50.8724314279756,-49.8749327725251,
-48.8774341170746,-47.8799354616241,-47.8286804139493),.UNSPECIFIED.);
#463=B_SPLINE_CURVE_WITH_KNOTS('',3,(#24078,#24079,#24080,#24081,#24082,
#24083,#24084,#24085,#24086,#24087,#24088,#24089,#24090,#24091,#24092,#24093,
#24094,#24095,#24096,#24097,#24098,#24099),.UNSPECIFIED.,.F.,.F.,(4,3,3,
3,3,3,3,4),(45.292119405429,45.8849381507231,46.8824368061736,47.8799354616241,
48.8774341170746,49.8749327725251,50.8724314279756,51.5753047126086),
 .UNSPECIFIED.);
#464=B_SPLINE_CURVE_WITH_KNOTS('',3,(#24100,#24101,#24102,#24103,#24104,
#24105,#24106,#24107,#24108,#24109,#24110,#24111,#24112,#24113,#24114,#24115,
#24116,#24117,#24118,#24119,#24120,#24121),.UNSPECIFIED.,.F.,.F.,(4,3,3,
3,3,3,3,4),(-47.8286804139493,-46.8824368061736,-45.8849381507231,-44.8874394952726,
-43.8899408398221,-42.8924421843716,-41.8949435289211,-41.5454951067697),
 .UNSPECIFIED.);
#465=B_SPLINE_CURVE_WITH_KNOTS('',3,(#24126,#24127,#24128,#24129,#24130,
#24131,#24132,#24133,#24134,#24135,#24136,#24137,#24138,#24139,#24140,#24141,
#24142,#24143,#24144,#24145,#24146,#24147),.UNSPECIFIED.,.F.,.F.,(4,3,3,
3,3,3,3,4),(39.0089340982494,39.8999462180201,40.8974448734706,41.8949435289211,
42.8924421843716,43.8899408398221,44.8874394952726,45.292119405429),
 .UNSPECIFIED.);
#466=B_SPLINE_CURVE_WITH_KNOTS('',3,(#24148,#24149,#24150,#24151,#24152,
#24153,#24154,#24155,#24156,#24157,#24158,#24159,#24160,#24161,#24162,#24163,
#24164,#24165,#24166,#24167,#24168,#24169),.UNSPECIFIED.,.F.,.F.,(4,3,3,
3,3,3,3,4),(-41.5454951067697,-40.8974448734706,-39.8999462180201,-38.9024475625696,
-37.9049489071191,-36.9074502516685,-35.909951596218,-35.2623097995902),
 .UNSPECIFIED.);
#467=B_SPLINE_CURVE_WITH_KNOTS('',3,(#24174,#24175,#24176,#24177,#24178,
#24179,#24180,#24181,#24182,#24183,#24184,#24185,#24186,#24187,#24188,#24189,
#24190,#24191,#24192,#24193,#24194,#24195,#24196,#24197,#24198),
 .UNSPECIFIED.,.F.,.F.,(4,3,3,3,3,3,3,3,4),(32.7257487910699,32.9174556298665,
33.9149542853171,34.9124529407676,35.9099515962181,36.9074502516685,37.904948907119,
38.9024475625696,39.0089340982494),.UNSPECIFIED.);
#468=B_SPLINE_CURVE_WITH_KNOTS('',3,(#24199,#24200,#24201,#24202,#24203,
#24204,#24205,#24206,#24207,#24208,#24209,#24210,#24211,#24212,#24213,#24214,
#24215,#24216,#24217,#24218,#24219,#24220),.UNSPECIFIED.,.F.,.F.,(4,3,3,
3,3,3,3,4),(-35.2623097995902,-34.9124529407676,-33.9149542853171,-32.9174556298665,
-31.919956974416,-30.9224583189655,-29.9249596635151,-28.9791244924106),
 .UNSPECIFIED.);
#469=B_SPLINE_CURVE_WITH_KNOTS('',3,(#24225,#24226,#24227,#24228,#24229,
#24230,#24231,#24232,#24233,#24234,#24235,#24236,#24237,#24238,#24239,#24240,
#24241,#24242,#24243,#24244,#24245,#24246),.UNSPECIFIED.,.F.,.F.,(4,3,3,
3,3,3,3,4),(26.4425634838902,26.9324636971635,27.929962352614,28.9274610080645,
29.924959663515,30.9224583189655,31.919956974416,32.7257487910699),
 .UNSPECIFIED.);
#470=B_SPLINE_CURVE_WITH_KNOTS('',3,(#24247,#24248,#24249,#24250,#24251,
#24252,#24253,#24254,#24255,#24256,#24257,#24258,#24259,#24260,#24261,#24262,
#24263,#24264,#24265,#24266,#24267,#24268,#24269,#24270,#24271),
 .UNSPECIFIED.,.F.,.F.,(4,3,3,3,3,3,3,3,4),(-28.9791244924106,-28.9274610080645,
-27.929962352614,-26.9324636971635,-25.934965041713,-24.9374663862625,-23.939967730812,
-22.9424690753615,-22.6959391852309),.UNSPECIFIED.);
#471=B_SPLINE_CURVE_WITH_KNOTS('',3,(#24276,#24277,#24278,#24279,#24280,
#24281,#24282,#24283,#24284,#24285,#24286,#24287,#24288,#24289,#24290,#24291,
#24292,#24293,#24294,#24295,#24296,#24297),.UNSPECIFIED.,.F.,.F.,(4,3,3,
3,3,3,3,4),(20.1593781767106,20.9474717644605,21.944970419911,22.9424690753615,
23.939967730812,24.9374663862625,25.934965041713,26.4425634838902),
 .UNSPECIFIED.);
#472=B_SPLINE_CURVE_WITH_KNOTS('',3,(#24298,#24299,#24300,#24301,#24302,
#24303,#24304,#24305,#24306,#24307,#24308,#24309,#24310,#24311,#24312,#24313,
#24314,#24315,#24316,#24317,#24318,#24319),.UNSPECIFIED.,.F.,.F.,(4,3,3,
3,3,3,3,4),(-22.6959391852309,-21.944970419911,-20.9474717644605,-19.94997310901,
-18.9524744535595,-17.954975798109,-16.9574771426585,-16.4127538780514),
 .UNSPECIFIED.);
#473=B_SPLINE_CURVE_WITH_KNOTS('',3,(#24324,#24325,#24326,#24327,#24328,
#24329,#24330,#24331,#24332,#24333,#24334,#24335,#24336,#24337,#24338,#24339,
#24340,#24341,#24342,#24343,#24344,#24345,#24346,#24347,#24348),
 .UNSPECIFIED.,.F.,.F.,(4,3,3,3,3,3,3,3,4),(13.8761928695311,13.964981176307,
14.9624798317575,15.959978487208,16.9574771426585,17.954975798109,18.9524744535595,
19.94997310901,20.1593781767106),.UNSPECIFIED.);
#474=B_SPLINE_CURVE_WITH_KNOTS('',3,(#24349,#24350,#24351,#24352,#24353,
#24354,#24355,#24356,#24357,#24358,#24359,#24360,#24361,#24362,#24363,#24364,
#24365,#24366,#24367,#24368,#24369,#24370),.UNSPECIFIED.,.F.,.F.,(4,3,3,
3,3,3,3,4),(-16.4127538780514,-15.959978487208,-14.9624798317575,-13.964981176307,
-12.9674825208565,-11.969983865406,-10.9724852099555,-10.1295685708718),
 .UNSPECIFIED.);
#475=B_SPLINE_CURVE_WITH_KNOTS('',3,(#24376,#24377,#24378,#24379,#24380,
#24381,#24382,#24383,#24384,#24385,#24386,#24387,#24388),.UNSPECIFIED.,
 .F.,.F.,(4,3,3,3,4),(-3.84638326369218,-2.9924959663515,-1.994997310901,
-0.997498655450501,0.),.UNSPECIFIED.);
#476=B_SPLINE_CURVE_WITH_KNOTS('',3,(#24391,#24392,#24393,#24394,#24395,
#24396,#24397,#24398,#24399,#24400,#24401,#24402,#24403,#24404,#24405,#24406,
#24407,#24408,#24409),.UNSPECIFIED.,.F.,.F.,(4,3,3,3,3,3,4),(2.01461286527449,
2.99249596635151,3.98999462180201,4.98749327725251,5.98499193270301,6.98249058815351,
7.59300756235149),.UNSPECIFIED.);
#477=B_SPLINE_CURVE_WITH_KNOTS('',3,(#24415,#24416,#24417,#24418,#24419),
 .UNSPECIFIED.,.F.,.F.,(4,1,4),(128.805298797182,129.566421347416,130.563920002866),
 .UNSPECIFIED.);
#478=B_SPLINE_CURVE_WITH_KNOTS('',3,(#24422,#24423,#24424,#24425,#24426,
#24427),.UNSPECIFIED.,.F.,.F.,(4,1,1,4),(128.805298797182,129.110486389585,
130.107985045035,131.085868146112),.UNSPECIFIED.);
#479=B_SPLINE_CURVE_WITH_KNOTS('',3,(#24432,#24433,#24434,#24435,#24436,
#24437,#24438,#24439,#24440,#24441,#24442),.UNSPECIFIED.,.F.,.F.,(4,1,1,
1,1,1,1,1,4),(122.522113490002,122.583930759262,123.581429414713,124.578928070163,
125.576426725614,126.573925381064,127.571424036515,128.568922691965,128.805298797182),
 .UNSPECIFIED.);
#480=B_SPLINE_CURVE_WITH_KNOTS('',3,(#24443,#24444,#24445,#24446,#24447,
#24448,#24449,#24450,#24451,#24452),.UNSPECIFIED.,.F.,.F.,(4,1,1,1,1,1,
1,4),(122.522113490002,123.125494456882,124.122993112332,125.120491767783,
126.117990423233,127.115489078684,128.112987734134,128.805298797182),
 .UNSPECIFIED.);
#481=B_SPLINE_CURVE_WITH_KNOTS('',3,(#24457,#24458,#24459,#24460,#24461,
#24462,#24463,#24464,#24465,#24466),.UNSPECIFIED.,.F.,.F.,(4,1,1,1,1,1,
1,4),(116.238928182822,116.598938826559,117.59643748201,118.59393613746,
119.591434792911,120.588933448361,121.586432103812,122.522113490002),
 .UNSPECIFIED.);
#482=B_SPLINE_CURVE_WITH_KNOTS('',3,(#24467,#24468,#24469,#24470,#24471,
#24472,#24473,#24474,#24475,#24476),.UNSPECIFIED.,.F.,.F.,(4,1,1,1,1,1,
1,4),(116.238928182822,117.140502524179,118.138001179629,119.13549983508,
120.13299849053,121.130497145981,122.127995801431,122.522113490002),
 .UNSPECIFIED.);
#483=B_SPLINE_CURVE_WITH_KNOTS('',3,(#24481,#24482,#24483,#24484,#24485,
#24486,#24487,#24488,#24489,#24490),.UNSPECIFIED.,.F.,.F.,(4,1,1,1,1,1,
1,4),(109.955742875643,110.613946893856,111.611445549307,112.608944204757,
113.606442860208,114.603941515658,115.601440171109,116.238928182822),
 .UNSPECIFIED.);
#484=B_SPLINE_CURVE_WITH_KNOTS('',3,(#24491,#24492,#24493,#24494,#24495,
#24496,#24497,#24498,#24499,#24500,#24501),.UNSPECIFIED.,.F.,.F.,(4,1,1,
1,1,1,1,1,4),(109.955742875643,110.158011936025,111.155510591476,112.153009246926,
113.150507902377,114.148006557827,115.145505213278,116.143003868728,116.238928182822),
 .UNSPECIFIED.);
#485=B_SPLINE_CURVE_WITH_KNOTS('',3,(#24506,#24507,#24508,#24509,#24510,
#24511,#24512,#24513,#24514,#24515),.UNSPECIFIED.,.F.,.F.,(4,1,1,1,1,1,
1,4),(103.672557568463,104.628954961153,105.626453616604,106.623952272054,
107.621450927505,108.618949582955,109.616448238406,109.955742875643),
 .UNSPECIFIED.);
#486=B_SPLINE_CURVE_WITH_KNOTS('',3,(#24516,#24517,#24518,#24519,#24520,
#24521,#24522,#24523,#24524,#24525),.UNSPECIFIED.,.F.,.F.,(4,1,1,1,1,1,
1,4),(103.672557568463,104.173020003322,105.170518658772,106.168017314223,
107.165515969673,108.163014625124,109.160513280574,109.955742875643),
 .UNSPECIFIED.);
#487=B_SPLINE_CURVE_WITH_KNOTS('',3,(#24530,#24531,#24532,#24533,#24534,
#24535,#24536,#24537,#24538,#24539,#24540),.UNSPECIFIED.,.F.,.F.,(4,1,1,
1,1,1,1,1,4),(97.3893722612835,97.6464643729998,98.6439630284503,99.6414616839008,
100.638960339351,101.636458994802,102.633957650252,103.631456305703,103.672557568463),
 .UNSPECIFIED.);
#488=B_SPLINE_CURVE_WITH_KNOTS('',3,(#24541,#24542,#24543,#24544,#24545,
#24546,#24547,#24548,#24549,#24550),.UNSPECIFIED.,.F.,.F.,(4,1,1,1,1,1,
1,4),(97.3893722612835,98.188028070619,99.1855267260695,100.18302538152,
101.18052403697,102.178022692421,103.175521347871,103.672557568463),
 .UNSPECIFIED.);
#489=B_SPLINE_CURVE_WITH_KNOTS('',3,(#24555,#24556,#24557,#24558,#24559,
#24560,#24561,#24562,#24563,#24564),.UNSPECIFIED.,.F.,.F.,(4,1,1,1,1,1,
1,4),(91.1061869541039,91.6614724402968,92.6589710957473,93.6564697511978,
94.6539684066483,95.6514670620988,96.6489657175493,97.3893722612835),
 .UNSPECIFIED.);
#490=B_SPLINE_CURVE_WITH_KNOTS('',3,(#24565,#24566,#24567,#24568,#24569,
#24570,#24571,#24572,#24573,#24574,#24575),.UNSPECIFIED.,.F.,.F.,(4,1,1,
1,1,1,1,1,4),(91.106186954104,91.2055374824655,92.203036137916,93.2005347933665,
94.198033448817,95.1955321042675,96.193030759718,97.1905294151685,97.3893722612835),
 .UNSPECIFIED.);
#491=B_SPLINE_CURVE_WITH_KNOTS('',3,(#24580,#24581,#24582,#24583,#24584,
#24585,#24586,#24587,#24588,#24589),.UNSPECIFIED.,.F.,.F.,(4,1,1,1,1,1,
1,4),(84.8230016469243,85.6764805075938,86.6739791630443,87.6714778184948,
88.6689764739453,89.6664751293958,90.6639737848463,91.1061869541039),
 .UNSPECIFIED.);
#492=B_SPLINE_CURVE_WITH_KNOTS('',3,(#24590,#24591,#24592,#24593,#24594,
#24595,#24596,#24597,#24598,#24599),.UNSPECIFIED.,.F.,.F.,(4,1,1,1,1,1,
1,4),(84.8230016469244,85.2205455497625,86.218044205213,87.2155428606635,
88.213041516114,89.2105401715645,90.208038827015,91.106186954104),
 .UNSPECIFIED.);
#493=B_SPLINE_CURVE_WITH_KNOTS('',3,(#24604,#24605,#24606,#24607,#24608,
#24609,#24610,#24611,#24612,#24613,#24614),.UNSPECIFIED.,.F.,.F.,(4,1,1,
1,1,1,1,1,4),(78.5398163397448,78.6939899194402,79.6914885748908,80.6889872303413,
81.6864858857918,82.6839845412423,83.6814831966928,84.6789818521433,84.8230016469243),
 .UNSPECIFIED.);
#494=B_SPLINE_CURVE_WITH_KNOTS('',3,(#24615,#24616,#24617,#24618,#24619,
#24620,#24621,#24622,#24623,#24624),.UNSPECIFIED.,.F.,.F.,(4,1,1,1,1,1,
1,4),(78.5398163397448,79.2355536170595,80.23305227251,81.2305509279605,
82.228049583411,83.2255482388615,84.223046894312,84.8230016469244),
 .UNSPECIFIED.);
#495=B_SPLINE_CURVE_WITH_KNOTS('',3,(#24629,#24630,#24631,#24632,#24633,
#24634,#24635,#24636,#24637,#24638),.UNSPECIFIED.,.F.,.F.,(4,1,1,1,1,1,
1,4),(72.2566310325652,72.7089979867372,73.7064966421877,74.7039952976382,
75.7014939530887,76.6989926085392,77.6964912639897,78.5398163397448),
 .UNSPECIFIED.);
#496=B_SPLINE_CURVE_WITH_KNOTS('',3,(#24639,#24640,#24641,#24642,#24643,
#24644,#24645,#24646,#24647,#24648),.UNSPECIFIED.,.F.,.F.,(4,1,1,1,1,1,
1,4),(72.2566310325652,73.2505616843565,74.248060339807,75.2455589952575,
76.243057650708,77.2405563061585,78.238054961609,78.5398163397448),
 .UNSPECIFIED.);
#497=B_SPLINE_CURVE_WITH_KNOTS('',3,(#24653,#24654,#24655,#24656,#24657,
#24658,#24659,#24660,#24661,#24662),.UNSPECIFIED.,.F.,.F.,(4,1,1,1,1,1,
1,4),(65.9734457253856,66.7240060540342,67.7215047094847,68.7190033649352,
69.7165020203857,70.7140006758362,71.7114993312867,72.2566310325652),
 .UNSPECIFIED.);
#498=B_SPLINE_CURVE_WITH_KNOTS('',3,(#24663,#24664,#24665,#24666,#24667,
#24668,#24669,#24670,#24671,#24672,#24673),.UNSPECIFIED.,.F.,.F.,(4,1,1,
1,1,1,1,1,4),(65.9734457253856,66.2680710962029,67.2655697516534,68.2630684071039,
69.2605670625544,70.2580657180049,71.2555643734554,72.2530630289059,72.2566310325652),
 .UNSPECIFIED.);
#499=B_SPLINE_CURVE_WITH_KNOTS('',3,(#24678,#24679,#24680,#24681,#24682,
#24683,#24684,#24685,#24686,#24687,#24688),.UNSPECIFIED.,.F.,.F.,(4,1,1,
1,1,1,1,1,4),(59.690260418206,59.7415154658807,60.7390141213312,61.7365127767817,
62.7340114322322,63.7315100876827,64.7290087431332,65.7265073985837,65.9734457253856),
 .UNSPECIFIED.);
#500=B_SPLINE_CURVE_WITH_KNOTS('',3,(#24689,#24690,#24691,#24692,#24693,
#24694,#24695,#24696,#24697,#24698),.UNSPECIFIED.,.F.,.F.,(4,1,1,1,1,1,
1,4),(59.690260418206,60.2830791634999,61.2805778189504,62.2780764744009,
63.2755751298514,64.2730737853019,65.2705724407524,65.9734457253856),
 .UNSPECIFIED.);
#501=B_SPLINE_CURVE_WITH_KNOTS('',3,(#24703,#24704,#24705,#24706,#24707,
#24708,#24709,#24710,#24711,#24712),.UNSPECIFIED.,.F.,.F.,(4,1,1,1,1,1,
1,4),(53.4070751110263,53.7565235331777,54.7540221886282,55.7515208440787,
56.7490194995292,57.7465181549797,58.7440168104302,59.690260418206),
 .UNSPECIFIED.);
#502=B_SPLINE_CURVE_WITH_KNOTS('',3,(#24713,#24714,#24715,#24716,#24717,
#24718,#24719,#24720,#24721,#24722),.UNSPECIFIED.,.F.,.F.,(4,1,1,1,1,1,
1,4),(53.4070751110264,54.2980872307969,55.2955858862474,56.2930845416979,
57.2905831971484,58.2880818525989,59.2855805080494,59.690260418206),
 .UNSPECIFIED.);
#503=B_SPLINE_CURVE_WITH_KNOTS('',3,(#24727,#24728,#24729,#24730,#24731,
#24732,#24733,#24734,#24735,#24736),.UNSPECIFIED.,.F.,.F.,(4,1,1,1,1,1,
1,4),(47.1238898038468,47.7715316004747,48.7690302559252,49.7665289113757,
50.7640275668262,51.7615262222767,52.7590248777272,53.4070751110263),
 .UNSPECIFIED.);
#504=B_SPLINE_CURVE_WITH_KNOTS('',3,(#24737,#24738,#24739,#24740,#24741,
#24742,#24743,#24744,#24745,#24746,#24747),.UNSPECIFIED.,.F.,.F.,(4,1,1,
1,1,1,1,1,4),(47.1238898038468,47.3155966426434,48.3130952980939,49.3105939535444,
50.3080926089949,51.3055912644454,52.3030899198959,53.3005885753464,53.4070751110264),
 .UNSPECIFIED.);
#505=B_SPLINE_CURVE_WITH_KNOTS('',3,(#24752,#24753,#24754,#24755,#24756,
#24757,#24758,#24759,#24760,#24761),.UNSPECIFIED.,.F.,.F.,(4,1,1,1,1,1,
1,4),(40.8407044966672,41.7865396677717,42.7840383232222,43.7815369786727,
44.7790356341232,45.7765342895737,46.7740329450242,47.1238898038468),
 .UNSPECIFIED.);
#506=B_SPLINE_CURVE_WITH_KNOTS('',3,(#24762,#24763,#24764,#24765,#24766,
#24767,#24768,#24769,#24770,#24771),.UNSPECIFIED.,.F.,.F.,(4,1,1,1,1,1,
1,4),(40.8407044966672,41.3306047099404,42.3281033653909,43.3256020208414,
44.3231006762919,45.3205993317424,46.3180979871929,47.1238898038468),
 .UNSPECIFIED.);
#507=B_SPLINE_CURVE_WITH_KNOTS('',3,(#24776,#24777,#24778,#24779,#24780,
#24781,#24782,#24783,#24784,#24785,#24786),.UNSPECIFIED.,.F.,.F.,(4,1,1,
1,1,1,1,1,4),(34.5575191894876,34.8040490796182,35.8015477350687,36.7990463905192,
37.7965450459697,38.7940437014202,39.7915423568707,40.7890410123212,40.8407044966672),
 .UNSPECIFIED.);
#508=B_SPLINE_CURVE_WITH_KNOTS('',3,(#24787,#24788,#24789,#24790,#24791,
#24792,#24793,#24794,#24795,#24796),.UNSPECIFIED.,.F.,.F.,(4,1,1,1,1,1,
1,4),(34.5575191894877,35.3456127772374,36.3431114326879,37.3406100881384,
38.3381087435889,39.3356073990394,40.3331060544899,40.8407044966672),
 .UNSPECIFIED.);
#509=B_SPLINE_CURVE_WITH_KNOTS('',3,(#24801,#24802,#24803,#24804,#24805,
#24806,#24807,#24808,#24809,#24810),.UNSPECIFIED.,.F.,.F.,(4,1,1,1,1,1,
1,4),(28.2743338823081,28.8190571469152,29.8165558023657,30.8140544578162,
31.8115531132667,32.8090517687172,33.8065504241677,34.5575191894876),
 .UNSPECIFIED.);
#510=B_SPLINE_CURVE_WITH_KNOTS('',3,(#24811,#24812,#24813,#24814,#24815,
#24816,#24817,#24818,#24819,#24820,#24821),.UNSPECIFIED.,.F.,.F.,(4,1,1,
1,1,1,1,1,4),(28.2743338823081,28.3631221890839,29.3606208445344,30.3581194999849,
31.3556181554354,32.3531168108859,33.3506154663364,34.3481141217869,34.5575191894877),
 .UNSPECIFIED.);
#511=B_SPLINE_CURVE_WITH_KNOTS('',3,(#24826,#24827,#24828,#24829,#24830,
#24831,#24832,#24833,#24834,#24835),.UNSPECIFIED.,.F.,.F.,(4,1,1,1,1,1,
1,4),(21.9911485751284,22.8340652142122,23.8315638696627,24.8290625251132,
25.8265611805637,26.8240598360142,27.8215584914647,28.2743338823081),
 .UNSPECIFIED.);
#512=B_SPLINE_CURVE_WITH_KNOTS('',3,(#24836,#24837,#24838,#24839,#24840,
#24841,#24842,#24843,#24844,#24845),.UNSPECIFIED.,.F.,.F.,(4,1,1,1,1,1,
1,4),(21.9911485751284,22.3781302563809,23.3756289118314,24.3731275672819,
25.3706262227324,26.3681248781829,27.3656235336334,28.2743338823081),
 .UNSPECIFIED.);
#513=B_SPLINE_CURVE_WITH_KNOTS('',3,(#24851,#24852,#24853,#24854,#24855),
 .UNSPECIFIED.,.F.,.F.,(4,1,4),(14.3981410127769,15.3956396682274,15.7079632679489),
 .UNSPECIFIED.);
#514=B_SPLINE_CURVE_WITH_KNOTS('',3,(#24858,#24859,#24860,#24861,#24862),
 .UNSPECIFIED.,.F.,.F.,(4,1,4),(13.8761928695311,14.8540759706082,15.7079632679488),
 .UNSPECIFIED.);
#515=B_SPLINE_CURVE_WITH_KNOTS('',3,(#24868,#24869,#24870,#24871,#24872,
#24873,#24874,#24875,#24876,#24877,#24878,#24879,#24880,#24881,#24882,#24883),
 .UNSPECIFIED.,.F.,.F.,(4,3,3,3,3,4),(114.407157784405,114.712345376808,
115.709844032258,116.707342687709,117.704841343159,118.70233999861),
 .UNSPECIFIED.);
#516=B_SPLINE_CURVE_WITH_KNOTS('',3,(#24891,#24892,#24893,#24894,#24895,
#24896,#24897,#24898,#24899,#24900,#24901,#24902,#24903,#24904,#24905,#24906,
#24907,#24908,#24909,#24910,#24911,#24912),.UNSPECIFIED.,.F.,.F.,(4,3,3,
3,3,3,3,4),(-116.687727133335,-115.709844032258,-114.712345376808,-113.714846721357,
-112.717348065907,-111.719849410456,-110.722350755006,-110.660533485745),
 .UNSPECIFIED.);
#517=B_SPLINE_CURVE_WITH_KNOTS('',3,(#24917,#24918,#24919,#24920,#24921,
#24922,#24923,#24924,#24925,#24926,#24927,#24928,#24929,#24930,#24931,#24932,
#24933,#24934,#24935,#24936,#24937,#24938),.UNSPECIFIED.,.F.,.F.,(4,3,3,
3,3,3,3,4),(108.123972477225,108.727353444105,109.724852099555,110.722350755006,
111.719849410456,112.717348065907,113.714846721357,114.407157784405),
 .UNSPECIFIED.);
#518=B_SPLINE_CURVE_WITH_KNOTS('',3,(#24939,#24940,#24941,#24942,#24943,
#24944,#24945,#24946,#24947,#24948,#24949,#24950,#24951,#24952,#24953,#24954,
#24955,#24956,#24957,#24958,#24959,#24960),.UNSPECIFIED.,.F.,.F.,(4,3,3,
3,3,3,3,4),(-110.660533485745,-109.724852099555,-108.727353444105,-107.729854788654,
-106.732356133204,-105.734857477753,-104.737358822303,-104.377348178566),
 .UNSPECIFIED.);
#519=B_SPLINE_CURVE_WITH_KNOTS('',3,(#24965,#24966,#24967,#24968,#24969,
#24970,#24971,#24972,#24973,#24974,#24975,#24976,#24977,#24978,#24979,#24980,
#24981,#24982,#24983,#24984,#24985,#24986),.UNSPECIFIED.,.F.,.F.,(4,3,3,
3,3,3,3,4),(101.840787170045,102.742361511402,103.739860166852,104.737358822303,
105.734857477753,106.732356133204,107.729854788654,108.123972477225),
 .UNSPECIFIED.);
#520=B_SPLINE_CURVE_WITH_KNOTS('',3,(#24987,#24988,#24989,#24990,#24991,
#24992,#24993,#24994,#24995,#24996,#24997,#24998,#24999,#25000,#25001,#25002,
#25003,#25004,#25005,#25006,#25007,#25008),.UNSPECIFIED.,.F.,.F.,(4,3,3,
3,3,3,3,4),(-104.377348178566,-103.739860166852,-102.742361511402,-101.744862855951,
-100.747364200501,-99.7498655450501,-98.7523668895996,-98.094162871386),
 .UNSPECIFIED.);
#521=B_SPLINE_CURVE_WITH_KNOTS('',3,(#25013,#25014,#25015,#25016,#25017,
#25018,#25019,#25020,#25021,#25022,#25023,#25024,#25025,#25026,#25027,#25028,
#25029,#25030,#25031,#25032,#25033,#25034,#25035,#25036,#25037),
 .UNSPECIFIED.,.F.,.F.,(4,3,3,3,3,3,3,3,4),(95.5576018628657,95.7598709232481,
96.7573695786986,97.7548682341491,98.7523668895996,99.7498655450501,100.747364200501,
101.744862855951,101.840787170045),.UNSPECIFIED.);
#522=B_SPLINE_CURVE_WITH_KNOTS('',3,(#25038,#25039,#25040,#25041,#25042,
#25043,#25044,#25045,#25046,#25047,#25048,#25049,#25050,#25051,#25052,#25053,
#25054,#25055,#25056,#25057,#25058,#25059),.UNSPECIFIED.,.F.,.F.,(4,3,3,
3,3,3,3,4),(-98.094162871386,-97.7548682341491,-96.7573695786986,-95.7598709232481,
-94.7623722677976,-93.7648736123471,-92.7673749568966,-91.8109775642064),
 .UNSPECIFIED.);
#523=B_SPLINE_CURVE_WITH_KNOTS('',3,(#25064,#25065,#25066,#25067,#25068,
#25069,#25070,#25071,#25072,#25073,#25074,#25075,#25076,#25077,#25078,#25079,
#25080,#25081,#25082,#25083,#25084,#25085),.UNSPECIFIED.,.F.,.F.,(4,3,3,
3,3,3,3,4),(89.2744165556862,89.7748789905451,90.7723776459956,91.7698763014461,
92.7673749568966,93.7648736123471,94.7623722677976,95.5576018628657),
 .UNSPECIFIED.);
#524=B_SPLINE_CURVE_WITH_KNOTS('',3,(#25086,#25087,#25088,#25089,#25090,
#25091,#25092,#25093,#25094,#25095,#25096,#25097,#25098,#25099,#25100,#25101,
#25102,#25103,#25104,#25105,#25106,#25107,#25108,#25109,#25110),
 .UNSPECIFIED.,.F.,.F.,(4,3,3,3,3,3,3,3,4),(-91.8109775642064,-91.7698763014461,
-90.7723776459956,-89.7748789905451,-88.7773803350946,-87.7798816796441,
-86.7823830241936,-85.7848843687431,-85.5277922570269),.UNSPECIFIED.);
#525=B_SPLINE_CURVE_WITH_KNOTS('',3,(#25115,#25116,#25117,#25118,#25119,
#25120,#25121,#25122,#25123,#25124,#25125,#25126,#25127,#25128,#25129,#25130,
#25131,#25132,#25133,#25134,#25135,#25136),.UNSPECIFIED.,.F.,.F.,(4,3,3,
3,3,3,3,4),(82.9912312485066,83.7898870578421,84.7873857132926,85.7848843687431,
86.7823830241936,87.7798816796441,88.7773803350946,89.2744165556862),
 .UNSPECIFIED.);
#526=B_SPLINE_CURVE_WITH_KNOTS('',3,(#25137,#25138,#25139,#25140,#25141,
#25142,#25143,#25144,#25145,#25146,#25147,#25148,#25149,#25150,#25151,#25152,
#25153,#25154,#25155,#25156,#25157,#25158),.UNSPECIFIED.,.F.,.F.,(4,3,3,
3,3,3,3,4),(-85.5277922570269,-84.7873857132926,-83.7898870578422,-82.7923884023916,
-81.7948897469411,-80.7973910914906,-79.7998924360401,-79.2446069498473),
 .UNSPECIFIED.);
#527=B_SPLINE_CURVE_WITH_KNOTS('',3,(#25163,#25164,#25165,#25166,#25167,
#25168,#25169,#25170,#25171,#25172,#25173,#25174,#25175,#25176,#25177,#25178,
#25179,#25180,#25181,#25182,#25183,#25184,#25185,#25186,#25187),
 .UNSPECIFIED.,.F.,.F.,(4,3,3,3,3,3,3,3,4),(76.708045941327,76.8073964696886,
77.8048951251391,78.8023937805896,79.7998924360401,80.7973910914906,81.7948897469411,
82.7923884023916,82.9912312485066),.UNSPECIFIED.);
#528=B_SPLINE_CURVE_WITH_KNOTS('',3,(#25188,#25189,#25190,#25191,#25192,
#25193,#25194,#25195,#25196,#25197,#25198,#25199,#25200,#25201,#25202,#25203,
#25204,#25205,#25206,#25207,#25208,#25209),.UNSPECIFIED.,.F.,.F.,(4,3,3,
3,3,3,3,4),(-79.2446069498473,-78.8023937805896,-77.8048951251391,-76.8073964696886,
-75.8098978142381,-74.8123991587876,-73.8149005033371,-72.9614216426677),
 .UNSPECIFIED.);
#529=B_SPLINE_CURVE_WITH_KNOTS('',3,(#25214,#25215,#25216,#25217,#25218,
#25219,#25220,#25221,#25222,#25223,#25224,#25225,#25226,#25227,#25228,#25229,
#25230,#25231,#25232,#25233,#25234,#25235),.UNSPECIFIED.,.F.,.F.,(4,3,3,
3,3,3,3,4),(70.4248606341474,70.8224045369856,71.8199031924361,72.8174018478866,
73.8149005033371,74.8123991587876,75.8098978142381,76.708045941327),
 .UNSPECIFIED.);
#530=B_SPLINE_CURVE_WITH_KNOTS('',3,(#25236,#25237,#25238,#25239,#25240,
#25241,#25242,#25243,#25244,#25245,#25246,#25247,#25248,#25249,#25250,#25251,
#25252,#25253,#25254,#25255,#25256,#25257,#25258,#25259,#25260),
 .UNSPECIFIED.,.F.,.F.,(4,3,3,3,3,3,3,3,4),(-72.9614216426677,-72.8174018478866,
-71.8199031924361,-70.8224045369856,-69.8249058815351,-68.8274072260846,
-67.8299085706341,-66.8324099151836,-66.6782363354882),.UNSPECIFIED.);
#531=B_SPLINE_CURVE_WITH_KNOTS('',3,(#25265,#25266,#25267,#25268,#25269,
#25270,#25271,#25272,#25273,#25274,#25275,#25276,#25277,#25278,#25279,#25280,
#25281,#25282,#25283,#25284,#25285,#25286),.UNSPECIFIED.,.F.,.F.,(4,3,3,
3,3,3,3,4),(64.1416753269678,64.8374126042826,65.8349112597331,66.8324099151836,
67.8299085706341,68.8274072260846,69.8249058815351,70.4248606341474),
 .UNSPECIFIED.);
#532=B_SPLINE_CURVE_WITH_KNOTS('',3,(#25287,#25288,#25289,#25290,#25291,
#25292,#25293,#25294,#25295,#25296,#25297,#25298,#25299,#25300,#25301,#25302,
#25303,#25304,#25305,#25306,#25307,#25308),.UNSPECIFIED.,.F.,.F.,(4,3,3,
3,3,3,3,4),(-66.6782363354882,-65.8349112597331,-64.8374126042826,-63.8399139488321,
-62.8424152933816,-61.8449166379311,-60.8474179824806,-60.3950510283085),
 .UNSPECIFIED.);
#533=B_SPLINE_CURVE_WITH_KNOTS('',3,(#25313,#25314,#25315,#25316,#25317,
#25318,#25319,#25320,#25321,#25322,#25323,#25324,#25325,#25326,#25327,#25328,
#25329,#25330,#25331,#25332,#25333,#25334),.UNSPECIFIED.,.F.,.F.,(4,3,3,
3,3,3,3,4),(57.8584900197882,58.8524206715796,59.8499193270301,60.8474179824806,
61.8449166379311,62.8424152933816,63.8399139488321,64.1416753269678),
 .UNSPECIFIED.);
#534=B_SPLINE_CURVE_WITH_KNOTS('',3,(#25335,#25336,#25337,#25338,#25339,
#25340,#25341,#25342,#25343,#25344,#25345,#25346,#25347,#25348,#25349,#25350,
#25351,#25352,#25353,#25354,#25355,#25356),.UNSPECIFIED.,.F.,.F.,(4,3,3,
3,3,3,3,4),(-60.3950510283085,-59.8499193270301,-58.8524206715796,-57.8549220161291,
-56.8574233606786,-55.8599247052281,-54.8624260497776,-54.1118657211289),
 .UNSPECIFIED.);
#535=B_SPLINE_CURVE_WITH_KNOTS('',3,(#25361,#25362,#25363,#25364,#25365,
#25366,#25367,#25368,#25369,#25370,#25371,#25372,#25373,#25374,#25375,#25376,
#25377,#25378,#25379,#25380,#25381,#25382,#25383,#25384,#25385),
 .UNSPECIFIED.,.F.,.F.,(4,3,3,3,3,3,3,3,4),(51.5753047126086,51.8699300834261,
52.8674287388766,53.8649273943271,54.8624260497776,55.8599247052281,56.8574233606786,
57.8549220161291,57.8584900197882),.UNSPECIFIED.);
#536=B_SPLINE_CURVE_WITH_KNOTS('',3,(#25386,#25387,#25388,#25389,#25390,
#25391,#25392,#25393,#25394,#25395,#25396,#25397,#25398,#25399,#25400,#25401,
#25402,#25403,#25404,#25405,#25406,#25407,#25408,#25409,#25410),
 .UNSPECIFIED.,.F.,.F.,(4,3,3,3,3,3,3,3,4),(-54.1118657211289,-53.8649273943271,
-52.8674287388766,-51.8699300834261,-50.8724314279756,-49.8749327725251,
-48.8774341170746,-47.8799354616241,-47.8286804139493),.UNSPECIFIED.);
#537=B_SPLINE_CURVE_WITH_KNOTS('',3,(#25415,#25416,#25417,#25418,#25419,
#25420,#25421,#25422,#25423,#25424,#25425,#25426,#25427,#25428,#25429,#25430,
#25431,#25432,#25433,#25434,#25435,#25436),.UNSPECIFIED.,.F.,.F.,(4,3,3,
3,3,3,3,4),(45.292119405429,45.8849381507231,46.8824368061736,47.8799354616241,
48.8774341170746,49.8749327725251,50.8724314279756,51.5753047126086),
 .UNSPECIFIED.);
#538=B_SPLINE_CURVE_WITH_KNOTS('',3,(#25437,#25438,#25439,#25440,#25441,
#25442,#25443,#25444,#25445,#25446,#25447,#25448,#25449,#25450,#25451,#25452,
#25453,#25454,#25455,#25456,#25457,#25458),.UNSPECIFIED.,.F.,.F.,(4,3,3,
3,3,3,3,4),(-47.8286804139493,-46.8824368061736,-45.8849381507231,-44.8874394952726,
-43.8899408398221,-42.8924421843716,-41.8949435289211,-41.5454951067697),
 .UNSPECIFIED.);
#539=B_SPLINE_CURVE_WITH_KNOTS('',3,(#25463,#25464,#25465,#25466,#25467,
#25468,#25469,#25470,#25471,#25472,#25473,#25474,#25475,#25476,#25477,#25478,
#25479,#25480,#25481,#25482,#25483,#25484),.UNSPECIFIED.,.F.,.F.,(4,3,3,
3,3,3,3,4),(39.0089340982494,39.8999462180201,40.8974448734706,41.8949435289211,
42.8924421843716,43.8899408398221,44.8874394952726,45.292119405429),
 .UNSPECIFIED.);
#540=B_SPLINE_CURVE_WITH_KNOTS('',3,(#25485,#25486,#25487,#25488,#25489,
#25490,#25491,#25492,#25493,#25494,#25495,#25496,#25497,#25498,#25499,#25500,
#25501,#25502,#25503,#25504,#25505,#25506),.UNSPECIFIED.,.F.,.F.,(4,3,3,
3,3,3,3,4),(-41.5454951067697,-40.8974448734706,-39.8999462180201,-38.9024475625696,
-37.9049489071191,-36.9074502516685,-35.909951596218,-35.2623097995902),
 .UNSPECIFIED.);
#541=B_SPLINE_CURVE_WITH_KNOTS('',3,(#25511,#25512,#25513,#25514,#25515,
#25516,#25517,#25518,#25519,#25520,#25521,#25522,#25523,#25524,#25525,#25526,
#25527,#25528,#25529,#25530,#25531,#25532,#25533,#25534,#25535),
 .UNSPECIFIED.,.F.,.F.,(4,3,3,3,3,3,3,3,4),(32.7257487910699,32.9174556298665,
33.9149542853171,34.9124529407676,35.9099515962181,36.9074502516685,37.904948907119,
38.9024475625696,39.0089340982494),.UNSPECIFIED.);
#542=B_SPLINE_CURVE_WITH_KNOTS('',3,(#25536,#25537,#25538,#25539,#25540,
#25541,#25542,#25543,#25544,#25545,#25546,#25547,#25548,#25549,#25550,#25551,
#25552,#25553,#25554,#25555,#25556,#25557),.UNSPECIFIED.,.F.,.F.,(4,3,3,
3,3,3,3,4),(-35.2623097995902,-34.9124529407676,-33.9149542853171,-32.9174556298665,
-31.919956974416,-30.9224583189655,-29.9249596635151,-28.9791244924106),
 .UNSPECIFIED.);
#543=B_SPLINE_CURVE_WITH_KNOTS('',3,(#25562,#25563,#25564,#25565,#25566,
#25567,#25568,#25569,#25570,#25571,#25572,#25573,#25574,#25575,#25576,#25577,
#25578,#25579,#25580,#25581,#25582,#25583),.UNSPECIFIED.,.F.,.F.,(4,3,3,
3,3,3,3,4),(26.4425634838902,26.9324636971635,27.929962352614,28.9274610080645,
29.924959663515,30.9224583189655,31.919956974416,32.7257487910699),
 .UNSPECIFIED.);
#544=B_SPLINE_CURVE_WITH_KNOTS('',3,(#25584,#25585,#25586,#25587,#25588,
#25589,#25590,#25591,#25592,#25593,#25594,#25595,#25596,#25597,#25598,#25599,
#25600,#25601,#25602,#25603,#25604,#25605,#25606,#25607,#25608),
 .UNSPECIFIED.,.F.,.F.,(4,3,3,3,3,3,3,3,4),(-28.9791244924106,-28.9274610080645,
-27.929962352614,-26.9324636971635,-25.934965041713,-24.9374663862625,-23.939967730812,
-22.9424690753615,-22.6959391852309),.UNSPECIFIED.);
#545=B_SPLINE_CURVE_WITH_KNOTS('',3,(#25613,#25614,#25615,#25616,#25617,
#25618,#25619,#25620,#25621,#25622,#25623,#25624,#25625,#25626,#25627,#25628,
#25629,#25630,#25631,#25632,#25633,#25634),.UNSPECIFIED.,.F.,.F.,(4,3,3,
3,3,3,3,4),(20.1593781767106,20.9474717644605,21.944970419911,22.9424690753615,
23.939967730812,24.9374663862625,25.934965041713,26.4425634838902),
 .UNSPECIFIED.);
#546=B_SPLINE_CURVE_WITH_KNOTS('',3,(#25635,#25636,#25637,#25638,#25639,
#25640,#25641,#25642,#25643,#25644,#25645,#25646,#25647,#25648,#25649,#25650,
#25651,#25652,#25653,#25654,#25655,#25656),.UNSPECIFIED.,.F.,.F.,(4,3,3,
3,3,3,3,4),(-22.6959391852309,-21.944970419911,-20.9474717644605,-19.94997310901,
-18.9524744535595,-17.954975798109,-16.9574771426585,-16.4127538780514),
 .UNSPECIFIED.);
#547=B_SPLINE_CURVE_WITH_KNOTS('',3,(#25661,#25662,#25663,#25664,#25665,
#25666,#25667,#25668,#25669,#25670,#25671,#25672,#25673,#25674,#25675,#25676,
#25677,#25678,#25679,#25680,#25681,#25682,#25683,#25684,#25685),
 .UNSPECIFIED.,.F.,.F.,(4,3,3,3,3,3,3,3,4),(13.8761928695311,13.964981176307,
14.9624798317575,15.959978487208,16.9574771426585,17.954975798109,18.9524744535595,
19.94997310901,20.1593781767106),.UNSPECIFIED.);
#548=B_SPLINE_CURVE_WITH_KNOTS('',3,(#25686,#25687,#25688,#25689,#25690,
#25691,#25692,#25693,#25694,#25695,#25696,#25697,#25698,#25699,#25700,#25701,
#25702,#25703,#25704,#25705,#25706,#25707),.UNSPECIFIED.,.F.,.F.,(4,3,3,
3,3,3,3,4),(-16.4127538780514,-15.959978487208,-14.9624798317575,-13.964981176307,
-12.9674825208565,-11.969983865406,-10.9724852099555,-10.1295685708718),
 .UNSPECIFIED.);
#549=B_SPLINE_CURVE_WITH_KNOTS('',3,(#25713,#25714,#25715,#25716,#25717,
#25718,#25719,#25720,#25721,#25722,#25723,#25724,#25725),.UNSPECIFIED.,
 .F.,.F.,(4,3,3,3,4),(-3.84638326369218,-2.9924959663515,-1.994997310901,
-0.997498655450501,0.),.UNSPECIFIED.);
#550=B_SPLINE_CURVE_WITH_KNOTS('',3,(#25728,#25729,#25730,#25731,#25732,
#25733,#25734,#25735,#25736,#25737,#25738,#25739,#25740,#25741,#25742,#25743,
#25744,#25745,#25746),.UNSPECIFIED.,.F.,.F.,(4,3,3,3,3,3,4),(2.01461286527449,
2.99249596635151,3.98999462180201,4.98749327725251,5.98499193270301,6.98249058815351,
7.59300756235149),.UNSPECIFIED.);
#551=B_SPLINE_CURVE_WITH_KNOTS('',3,(#25752,#25753,#25754,#25755,#25756),
 .UNSPECIFIED.,.F.,.F.,(4,1,4),(128.805298797182,129.566421347416,130.563920002866),
 .UNSPECIFIED.);
#552=B_SPLINE_CURVE_WITH_KNOTS('',3,(#25759,#25760,#25761,#25762,#25763,
#25764),.UNSPECIFIED.,.F.,.F.,(4,1,1,4),(128.805298797182,129.110486389585,
130.107985045035,131.085868146112),.UNSPECIFIED.);
#553=B_SPLINE_CURVE_WITH_KNOTS('',3,(#25769,#25770,#25771,#25772,#25773,
#25774,#25775,#25776,#25777,#25778,#25779),.UNSPECIFIED.,.F.,.F.,(4,1,1,
1,1,1,1,1,4),(122.522113490002,122.583930759262,123.581429414713,124.578928070163,
125.576426725614,126.573925381064,127.571424036515,128.568922691965,128.805298797182),
 .UNSPECIFIED.);
#554=B_SPLINE_CURVE_WITH_KNOTS('',3,(#25780,#25781,#25782,#25783,#25784,
#25785,#25786,#25787,#25788,#25789),.UNSPECIFIED.,.F.,.F.,(4,1,1,1,1,1,
1,4),(122.522113490002,123.125494456882,124.122993112332,125.120491767783,
126.117990423233,127.115489078684,128.112987734134,128.805298797182),
 .UNSPECIFIED.);
#555=B_SPLINE_CURVE_WITH_KNOTS('',3,(#25794,#25795,#25796,#25797,#25798,
#25799,#25800,#25801,#25802,#25803),.UNSPECIFIED.,.F.,.F.,(4,1,1,1,1,1,
1,4),(116.238928182822,116.598938826559,117.59643748201,118.59393613746,
119.591434792911,120.588933448361,121.586432103812,122.522113490002),
 .UNSPECIFIED.);
#556=B_SPLINE_CURVE_WITH_KNOTS('',3,(#25804,#25805,#25806,#25807,#25808,
#25809,#25810,#25811,#25812,#25813),.UNSPECIFIED.,.F.,.F.,(4,1,1,1,1,1,
1,4),(116.238928182822,117.140502524179,118.138001179629,119.13549983508,
120.13299849053,121.130497145981,122.127995801431,122.522113490002),
 .UNSPECIFIED.);
#557=B_SPLINE_CURVE_WITH_KNOTS('',3,(#25818,#25819,#25820,#25821,#25822,
#25823,#25824,#25825,#25826,#25827),.UNSPECIFIED.,.F.,.F.,(4,1,1,1,1,1,
1,4),(109.955742875643,110.613946893856,111.611445549307,112.608944204757,
113.606442860208,114.603941515658,115.601440171109,116.238928182822),
 .UNSPECIFIED.);
#558=B_SPLINE_CURVE_WITH_KNOTS('',3,(#25828,#25829,#25830,#25831,#25832,
#25833,#25834,#25835,#25836,#25837,#25838),.UNSPECIFIED.,.F.,.F.,(4,1,1,
1,1,1,1,1,4),(109.955742875643,110.158011936025,111.155510591476,112.153009246926,
113.150507902377,114.148006557827,115.145505213278,116.143003868728,116.238928182822),
 .UNSPECIFIED.);
#559=B_SPLINE_CURVE_WITH_KNOTS('',3,(#25843,#25844,#25845,#25846,#25847,
#25848,#25849,#25850,#25851,#25852),.UNSPECIFIED.,.F.,.F.,(4,1,1,1,1,1,
1,4),(103.672557568463,104.628954961153,105.626453616604,106.623952272054,
107.621450927505,108.618949582955,109.616448238406,109.955742875643),
 .UNSPECIFIED.);
#560=B_SPLINE_CURVE_WITH_KNOTS('',3,(#25853,#25854,#25855,#25856,#25857,
#25858,#25859,#25860,#25861,#25862),.UNSPECIFIED.,.F.,.F.,(4,1,1,1,1,1,
1,4),(103.672557568463,104.173020003322,105.170518658772,106.168017314223,
107.165515969673,108.163014625124,109.160513280574,109.955742875643),
 .UNSPECIFIED.);
#561=B_SPLINE_CURVE_WITH_KNOTS('',3,(#25867,#25868,#25869,#25870,#25871,
#25872,#25873,#25874,#25875,#25876,#25877),.UNSPECIFIED.,.F.,.F.,(4,1,1,
1,1,1,1,1,4),(97.3893722612835,97.6464643729998,98.6439630284503,99.6414616839008,
100.638960339351,101.636458994802,102.633957650252,103.631456305703,103.672557568463),
 .UNSPECIFIED.);
#562=B_SPLINE_CURVE_WITH_KNOTS('',3,(#25878,#25879,#25880,#25881,#25882,
#25883,#25884,#25885,#25886,#25887),.UNSPECIFIED.,.F.,.F.,(4,1,1,1,1,1,
1,4),(97.3893722612835,98.188028070619,99.1855267260695,100.18302538152,
101.18052403697,102.178022692421,103.175521347871,103.672557568463),
 .UNSPECIFIED.);
#563=B_SPLINE_CURVE_WITH_KNOTS('',3,(#25892,#25893,#25894,#25895,#25896,
#25897,#25898,#25899,#25900,#25901),.UNSPECIFIED.,.F.,.F.,(4,1,1,1,1,1,
1,4),(91.1061869541039,91.6614724402968,92.6589710957473,93.6564697511978,
94.6539684066483,95.6514670620988,96.6489657175493,97.3893722612835),
 .UNSPECIFIED.);
#564=B_SPLINE_CURVE_WITH_KNOTS('',3,(#25902,#25903,#25904,#25905,#25906,
#25907,#25908,#25909,#25910,#25911,#25912),.UNSPECIFIED.,.F.,.F.,(4,1,1,
1,1,1,1,1,4),(91.106186954104,91.2055374824655,92.203036137916,93.2005347933665,
94.198033448817,95.1955321042675,96.193030759718,97.1905294151685,97.3893722612835),
 .UNSPECIFIED.);
#565=B_SPLINE_CURVE_WITH_KNOTS('',3,(#25917,#25918,#25919,#25920,#25921,
#25922,#25923,#25924,#25925,#25926),.UNSPECIFIED.,.F.,.F.,(4,1,1,1,1,1,
1,4),(84.8230016469243,85.6764805075938,86.6739791630443,87.6714778184948,
88.6689764739453,89.6664751293958,90.6639737848463,91.1061869541039),
 .UNSPECIFIED.);
#566=B_SPLINE_CURVE_WITH_KNOTS('',3,(#25927,#25928,#25929,#25930,#25931,
#25932,#25933,#25934,#25935,#25936),.UNSPECIFIED.,.F.,.F.,(4,1,1,1,1,1,
1,4),(84.8230016469244,85.2205455497625,86.218044205213,87.2155428606635,
88.213041516114,89.2105401715645,90.208038827015,91.106186954104),
 .UNSPECIFIED.);
#567=B_SPLINE_CURVE_WITH_KNOTS('',3,(#25941,#25942,#25943,#25944,#25945,
#25946,#25947,#25948,#25949,#25950,#25951),.UNSPECIFIED.,.F.,.F.,(4,1,1,
1,1,1,1,1,4),(78.5398163397448,78.6939899194402,79.6914885748908,80.6889872303413,
81.6864858857918,82.6839845412423,83.6814831966928,84.6789818521433,84.8230016469243),
 .UNSPECIFIED.);
#568=B_SPLINE_CURVE_WITH_KNOTS('',3,(#25952,#25953,#25954,#25955,#25956,
#25957,#25958,#25959,#25960,#25961),.UNSPECIFIED.,.F.,.F.,(4,1,1,1,1,1,
1,4),(78.5398163397448,79.2355536170595,80.23305227251,81.2305509279605,
82.228049583411,83.2255482388615,84.223046894312,84.8230016469244),
 .UNSPECIFIED.);
#569=B_SPLINE_CURVE_WITH_KNOTS('',3,(#25966,#25967,#25968,#25969,#25970,
#25971,#25972,#25973,#25974,#25975),.UNSPECIFIED.,.F.,.F.,(4,1,1,1,1,1,
1,4),(72.2566310325652,72.7089979867372,73.7064966421877,74.7039952976382,
75.7014939530887,76.6989926085392,77.6964912639897,78.5398163397448),
 .UNSPECIFIED.);
#570=B_SPLINE_CURVE_WITH_KNOTS('',3,(#25976,#25977,#25978,#25979,#25980,
#25981,#25982,#25983,#25984,#25985),.UNSPECIFIED.,.F.,.F.,(4,1,1,1,1,1,
1,4),(72.2566310325652,73.2505616843565,74.248060339807,75.2455589952575,
76.243057650708,77.2405563061585,78.238054961609,78.5398163397448),
 .UNSPECIFIED.);
#571=B_SPLINE_CURVE_WITH_KNOTS('',3,(#25990,#25991,#25992,#25993,#25994,
#25995,#25996,#25997,#25998,#25999),.UNSPECIFIED.,.F.,.F.,(4,1,1,1,1,1,
1,4),(65.9734457253856,66.7240060540342,67.7215047094847,68.7190033649352,
69.7165020203857,70.7140006758362,71.7114993312867,72.2566310325652),
 .UNSPECIFIED.);
#572=B_SPLINE_CURVE_WITH_KNOTS('',3,(#26000,#26001,#26002,#26003,#26004,
#26005,#26006,#26007,#26008,#26009,#26010),.UNSPECIFIED.,.F.,.F.,(4,1,1,
1,1,1,1,1,4),(65.9734457253856,66.2680710962029,67.2655697516534,68.2630684071039,
69.2605670625544,70.2580657180049,71.2555643734554,72.2530630289059,72.2566310325652),
 .UNSPECIFIED.);
#573=B_SPLINE_CURVE_WITH_KNOTS('',3,(#26015,#26016,#26017,#26018,#26019,
#26020,#26021,#26022,#26023,#26024,#26025),.UNSPECIFIED.,.F.,.F.,(4,1,1,
1,1,1,1,1,4),(59.690260418206,59.7415154658807,60.7390141213312,61.7365127767817,
62.7340114322322,63.7315100876827,64.7290087431332,65.7265073985837,65.9734457253856),
 .UNSPECIFIED.);
#574=B_SPLINE_CURVE_WITH_KNOTS('',3,(#26026,#26027,#26028,#26029,#26030,
#26031,#26032,#26033,#26034,#26035),.UNSPECIFIED.,.F.,.F.,(4,1,1,1,1,1,
1,4),(59.690260418206,60.2830791634999,61.2805778189504,62.2780764744009,
63.2755751298514,64.2730737853019,65.2705724407524,65.9734457253856),
 .UNSPECIFIED.);
#575=B_SPLINE_CURVE_WITH_KNOTS('',3,(#26040,#26041,#26042,#26043,#26044,
#26045,#26046,#26047,#26048,#26049),.UNSPECIFIED.,.F.,.F.,(4,1,1,1,1,1,
1,4),(53.4070751110263,53.7565235331777,54.7540221886282,55.7515208440787,
56.7490194995292,57.7465181549797,58.7440168104302,59.690260418206),
 .UNSPECIFIED.);
#576=B_SPLINE_CURVE_WITH_KNOTS('',3,(#26050,#26051,#26052,#26053,#26054,
#26055,#26056,#26057,#26058,#26059),.UNSPECIFIED.,.F.,.F.,(4,1,1,1,1,1,
1,4),(53.4070751110264,54.2980872307969,55.2955858862474,56.2930845416979,
57.2905831971484,58.2880818525989,59.2855805080494,59.690260418206),
 .UNSPECIFIED.);
#577=B_SPLINE_CURVE_WITH_KNOTS('',3,(#26064,#26065,#26066,#26067,#26068,
#26069,#26070,#26071,#26072,#26073),.UNSPECIFIED.,.F.,.F.,(4,1,1,1,1,1,
1,4),(47.1238898038468,47.7715316004747,48.7690302559252,49.7665289113757,
50.7640275668262,51.7615262222767,52.7590248777272,53.4070751110263),
 .UNSPECIFIED.);
#578=B_SPLINE_CURVE_WITH_KNOTS('',3,(#26074,#26075,#26076,#26077,#26078,
#26079,#26080,#26081,#26082,#26083,#26084),.UNSPECIFIED.,.F.,.F.,(4,1,1,
1,1,1,1,1,4),(47.1238898038468,47.3155966426434,48.3130952980939,49.3105939535444,
50.3080926089949,51.3055912644454,52.3030899198959,53.3005885753464,53.4070751110264),
 .UNSPECIFIED.);
#579=B_SPLINE_CURVE_WITH_KNOTS('',3,(#26089,#26090,#26091,#26092,#26093,
#26094,#26095,#26096,#26097,#26098),.UNSPECIFIED.,.F.,.F.,(4,1,1,1,1,1,
1,4),(40.8407044966672,41.7865396677717,42.7840383232222,43.7815369786727,
44.7790356341232,45.7765342895737,46.7740329450242,47.1238898038468),
 .UNSPECIFIED.);
#580=B_SPLINE_CURVE_WITH_KNOTS('',3,(#26099,#26100,#26101,#26102,#26103,
#26104,#26105,#26106,#26107,#26108),.UNSPECIFIED.,.F.,.F.,(4,1,1,1,1,1,
1,4),(40.8407044966672,41.3306047099404,42.3281033653909,43.3256020208414,
44.3231006762919,45.3205993317424,46.3180979871929,47.1238898038468),
 .UNSPECIFIED.);
#581=B_SPLINE_CURVE_WITH_KNOTS('',3,(#26113,#26114,#26115,#26116,#26117,
#26118,#26119,#26120,#26121,#26122,#26123),.UNSPECIFIED.,.F.,.F.,(4,1,1,
1,1,1,1,1,4),(34.5575191894876,34.8040490796182,35.8015477350687,36.7990463905192,
37.7965450459697,38.7940437014202,39.7915423568707,40.7890410123212,40.8407044966672),
 .UNSPECIFIED.);
#582=B_SPLINE_CURVE_WITH_KNOTS('',3,(#26124,#26125,#26126,#26127,#26128,
#26129,#26130,#26131,#26132,#26133),.UNSPECIFIED.,.F.,.F.,(4,1,1,1,1,1,
1,4),(34.5575191894877,35.3456127772374,36.3431114326879,37.3406100881384,
38.3381087435889,39.3356073990394,40.3331060544899,40.8407044966672),
 .UNSPECIFIED.);
#583=B_SPLINE_CURVE_WITH_KNOTS('',3,(#26138,#26139,#26140,#26141,#26142,
#26143,#26144,#26145,#26146,#26147),.UNSPECIFIED.,.F.,.F.,(4,1,1,1,1,1,
1,4),(28.2743338823081,28.8190571469152,29.8165558023657,30.8140544578162,
31.8115531132667,32.8090517687172,33.8065504241677,34.5575191894876),
 .UNSPECIFIED.);
#584=B_SPLINE_CURVE_WITH_KNOTS('',3,(#26148,#26149,#26150,#26151,#26152,
#26153,#26154,#26155,#26156,#26157,#26158),.UNSPECIFIED.,.F.,.F.,(4,1,1,
1,1,1,1,1,4),(28.2743338823081,28.3631221890839,29.3606208445344,30.3581194999849,
31.3556181554354,32.3531168108859,33.3506154663364,34.3481141217869,34.5575191894877),
 .UNSPECIFIED.);
#585=B_SPLINE_CURVE_WITH_KNOTS('',3,(#26163,#26164,#26165,#26166,#26167,
#26168,#26169,#26170,#26171,#26172),.UNSPECIFIED.,.F.,.F.,(4,1,1,1,1,1,
1,4),(21.9911485751284,22.8340652142122,23.8315638696627,24.8290625251132,
25.8265611805637,26.8240598360142,27.8215584914647,28.2743338823081),
 .UNSPECIFIED.);
#586=B_SPLINE_CURVE_WITH_KNOTS('',3,(#26173,#26174,#26175,#26176,#26177,
#26178,#26179,#26180,#26181,#26182),.UNSPECIFIED.,.F.,.F.,(4,1,1,1,1,1,
1,4),(21.9911485751284,22.3781302563809,23.3756289118314,24.3731275672819,
25.3706262227324,26.3681248781829,27.3656235336334,28.2743338823081),
 .UNSPECIFIED.);
#587=B_SPLINE_CURVE_WITH_KNOTS('',3,(#26188,#26189,#26190,#26191,#26192),
 .UNSPECIFIED.,.F.,.F.,(4,1,4),(14.3981410127769,15.3956396682274,15.7079632679489),
 .UNSPECIFIED.);
#588=B_SPLINE_CURVE_WITH_KNOTS('',3,(#26195,#26196,#26197,#26198,#26199),
 .UNSPECIFIED.,.F.,.F.,(4,1,4),(13.8761928695311,14.8540759706082,15.7079632679488),
 .UNSPECIFIED.);
#589=B_SPLINE_CURVE_WITH_KNOTS('',3,(#26205,#26206,#26207,#26208,#26209,
#26210,#26211,#26212,#26213,#26214,#26215,#26216,#26217,#26218,#26219,#26220),
 .UNSPECIFIED.,.F.,.F.,(4,3,3,3,3,4),(114.407157784404,114.712345376808,
115.709844032258,116.707342687709,117.704841343159,118.702339998609),
 .UNSPECIFIED.);
#590=B_SPLINE_CURVE_WITH_KNOTS('',3,(#26228,#26229,#26230,#26231,#26232,
#26233,#26234,#26235,#26236,#26237,#26238,#26239,#26240,#26241,#26242,#26243,
#26244,#26245,#26246,#26247,#26248,#26249),.UNSPECIFIED.,.F.,.F.,(4,3,3,
3,3,3,3,4),(-116.687727133335,-115.709844032258,-114.712345376808,-113.714846721357,
-112.717348065907,-111.719849410456,-110.722350755006,-110.660533485745),
 .UNSPECIFIED.);
#591=B_SPLINE_CURVE_WITH_KNOTS('',3,(#26254,#26255,#26256,#26257,#26258,
#26259,#26260,#26261,#26262,#26263,#26264,#26265,#26266,#26267,#26268,#26269,
#26270,#26271,#26272,#26273,#26274,#26275),.UNSPECIFIED.,.F.,.F.,(4,3,3,
3,3,3,3,4),(108.123972477224,108.727353444105,109.724852099555,110.722350755006,
111.719849410456,112.717348065907,113.714846721357,114.407157784404),
 .UNSPECIFIED.);
#592=B_SPLINE_CURVE_WITH_KNOTS('',3,(#26276,#26277,#26278,#26279,#26280,
#26281,#26282,#26283,#26284,#26285,#26286,#26287,#26288,#26289,#26290,#26291,
#26292,#26293,#26294,#26295,#26296,#26297),.UNSPECIFIED.,.F.,.F.,(4,3,3,
3,3,3,3,4),(-110.660533485745,-109.724852099555,-108.727353444105,-107.729854788654,
-106.732356133204,-105.734857477753,-104.737358822303,-104.377348178565),
 .UNSPECIFIED.);
#593=B_SPLINE_CURVE_WITH_KNOTS('',3,(#26302,#26303,#26304,#26305,#26306,
#26307,#26308,#26309,#26310,#26311,#26312,#26313,#26314,#26315,#26316,#26317,
#26318,#26319,#26320,#26321,#26322,#26323),.UNSPECIFIED.,.F.,.F.,(4,3,3,
3,3,3,3,4),(101.840787170045,102.742361511402,103.739860166852,104.737358822303,
105.734857477753,106.732356133204,107.729854788654,108.123972477224),
 .UNSPECIFIED.);
#594=B_SPLINE_CURVE_WITH_KNOTS('',3,(#26324,#26325,#26326,#26327,#26328,
#26329,#26330,#26331,#26332,#26333,#26334,#26335,#26336,#26337,#26338,#26339,
#26340,#26341,#26342,#26343,#26344,#26345),.UNSPECIFIED.,.F.,.F.,(4,3,3,
3,3,3,3,4),(-104.377348178565,-103.739860166852,-102.742361511402,-101.744862855951,
-100.747364200501,-99.74986554505,-98.7523668895995,-98.0941628713858),
 .UNSPECIFIED.);
#595=B_SPLINE_CURVE_WITH_KNOTS('',3,(#26350,#26351,#26352,#26353,#26354,
#26355,#26356,#26357,#26358,#26359,#26360,#26361,#26362,#26363,#26364,#26365,
#26366,#26367,#26368,#26369,#26370,#26371,#26372,#26373,#26374),
 .UNSPECIFIED.,.F.,.F.,(4,3,3,3,3,3,3,3,4),(95.5576018628653,95.7598709232481,
96.7573695786986,97.7548682341491,98.7523668895996,99.7498655450501,100.747364200501,
101.744862855951,101.840787170045),.UNSPECIFIED.);
#596=B_SPLINE_CURVE_WITH_KNOTS('',3,(#26375,#26376,#26377,#26378,#26379,
#26380,#26381,#26382,#26383,#26384,#26385,#26386,#26387,#26388,#26389,#26390,
#26391,#26392,#26393,#26394,#26395,#26396),.UNSPECIFIED.,.F.,.F.,(4,3,3,
3,3,3,3,4),(-98.0941628713858,-97.754868234149,-96.7573695786985,-95.759870923248,
-94.7623722677975,-93.764873612347,-92.7673749568965,-91.8109775642062),
 .UNSPECIFIED.);
#597=B_SPLINE_CURVE_WITH_KNOTS('',3,(#26401,#26402,#26403,#26404,#26405,
#26406,#26407,#26408,#26409,#26410,#26411,#26412,#26413,#26414,#26415,#26416,
#26417,#26418,#26419,#26420,#26421,#26422),.UNSPECIFIED.,.F.,.F.,(4,3,3,
3,3,3,3,4),(89.2744165556857,89.774878990545,90.7723776459955,91.769876301446,
92.7673749568965,93.764873612347,94.7623722677975,95.5576018628653),
 .UNSPECIFIED.);
#598=B_SPLINE_CURVE_WITH_KNOTS('',3,(#26423,#26424,#26425,#26426,#26427,
#26428,#26429,#26430,#26431,#26432,#26433,#26434,#26435,#26436,#26437,#26438,
#26439,#26440,#26441,#26442,#26443,#26444,#26445,#26446,#26447),
 .UNSPECIFIED.,.F.,.F.,(4,3,3,3,3,3,3,3,4),(-91.8109775642062,-91.769876301446,
-90.7723776459955,-89.774878990545,-88.7773803350945,-87.779881679644,-86.7823830241935,
-85.784884368743,-85.5277922570266),.UNSPECIFIED.);
#599=B_SPLINE_CURVE_WITH_KNOTS('',3,(#26452,#26453,#26454,#26455,#26456,
#26457,#26458,#26459,#26460,#26461,#26462,#26463,#26464,#26465,#26466,#26467,
#26468,#26469,#26470,#26471,#26472,#26473),.UNSPECIFIED.,.F.,.F.,(4,3,3,
3,3,3,3,4),(82.9912312485061,83.7898870578421,84.7873857132926,85.7848843687431,
86.7823830241935,87.779881679644,88.7773803350946,89.2744165556857),
 .UNSPECIFIED.);
#600=B_SPLINE_CURVE_WITH_KNOTS('',3,(#26474,#26475,#26476,#26477,#26478,
#26479,#26480,#26481,#26482,#26483,#26484,#26485,#26486,#26487,#26488,#26489,
#26490,#26491,#26492,#26493,#26494,#26495),.UNSPECIFIED.,.F.,.F.,(4,3,3,
3,3,3,3,4),(-85.5277922570266,-84.7873857132925,-83.789887057842,-82.7923884023915,
-81.794889746941,-80.7973910914905,-79.79989243604,-79.244606949847),
 .UNSPECIFIED.);
#601=B_SPLINE_CURVE_WITH_KNOTS('',3,(#26500,#26501,#26502,#26503,#26504,
#26505,#26506,#26507,#26508,#26509,#26510,#26511,#26512,#26513,#26514,#26515,
#26516,#26517,#26518,#26519,#26520,#26521,#26522,#26523,#26524),
 .UNSPECIFIED.,.F.,.F.,(4,3,3,3,3,3,3,3,4),(76.7080459413264,76.8073964696885,
77.804895125139,78.8023937805895,79.79989243604,80.7973910914905,81.7948897469411,
82.7923884023915,82.9912312485061),.UNSPECIFIED.);
#602=B_SPLINE_CURVE_WITH_KNOTS('',3,(#26525,#26526,#26527,#26528,#26529,
#26530,#26531,#26532,#26533,#26534,#26535,#26536,#26537,#26538,#26539,#26540,
#26541,#26542,#26543,#26544,#26545,#26546),.UNSPECIFIED.,.F.,.F.,(4,3,3,
3,3,3,3,4),(-79.244606949847,-78.8023937805895,-77.804895125139,-76.8073964696885,
-75.809897814238,-74.8123991587875,-73.814900503337,-72.9614216426674),
 .UNSPECIFIED.);
#603=B_SPLINE_CURVE_WITH_KNOTS('',3,(#26551,#26552,#26553,#26554,#26555,
#26556,#26557,#26558,#26559,#26560,#26561,#26562,#26563,#26564,#26565,#26566,
#26567,#26568,#26569,#26570,#26571,#26572),.UNSPECIFIED.,.F.,.F.,(4,3,3,
3,3,3,3,4),(70.4248606341468,70.8224045369855,71.8199031924361,72.8174018478865,
73.814900503337,74.8123991587875,75.809897814238,76.7080459413264),
 .UNSPECIFIED.);
#604=B_SPLINE_CURVE_WITH_KNOTS('',3,(#26573,#26574,#26575,#26576,#26577,
#26578,#26579,#26580,#26581,#26582,#26583,#26584,#26585,#26586,#26587,#26588,
#26589,#26590,#26591,#26592,#26593,#26594,#26595,#26596,#26597),
 .UNSPECIFIED.,.F.,.F.,(4,3,3,3,3,3,3,3,4),(-72.9614216426674,-72.8174018478865,
-71.819903192436,-70.8224045369855,-69.824905881535,-68.8274072260845,-67.829908570634,
-66.8324099151835,-66.6782363354877),.UNSPECIFIED.);
#605=B_SPLINE_CURVE_WITH_KNOTS('',3,(#26602,#26603,#26604,#26605,#26606,
#26607,#26608,#26609,#26610,#26611,#26612,#26613,#26614,#26615,#26616,#26617,
#26618,#26619,#26620,#26621,#26622,#26623),.UNSPECIFIED.,.F.,.F.,(4,3,3,
3,3,3,3,4),(64.1416753269672,64.8374126042825,65.834911259733,66.8324099151835,
67.829908570634,68.8274072260845,69.824905881535,70.4248606341468),
 .UNSPECIFIED.);
#606=B_SPLINE_CURVE_WITH_KNOTS('',3,(#26624,#26625,#26626,#26627,#26628,
#26629,#26630,#26631,#26632,#26633,#26634,#26635,#26636,#26637,#26638,#26639,
#26640,#26641,#26642,#26643,#26644,#26645),.UNSPECIFIED.,.F.,.F.,(4,3,3,
3,3,3,3,4),(-66.6782363354877,-65.834911259733,-64.8374126042825,-63.839913948832,
-62.8424152933815,-61.844916637931,-60.8474179824805,-60.3950510283081),
 .UNSPECIFIED.);
#607=B_SPLINE_CURVE_WITH_KNOTS('',3,(#26650,#26651,#26652,#26653,#26654,
#26655,#26656,#26657,#26658,#26659,#26660,#26661,#26662,#26663,#26664,#26665,
#26666,#26667,#26668,#26669,#26670,#26671),.UNSPECIFIED.,.F.,.F.,(4,3,3,
3,3,3,3,4),(57.8584900197876,58.8524206715795,59.84991932703,60.8474179824805,
61.844916637931,62.8424152933815,63.839913948832,64.1416753269672),
 .UNSPECIFIED.);
#608=B_SPLINE_CURVE_WITH_KNOTS('',3,(#26672,#26673,#26674,#26675,#26676,
#26677,#26678,#26679,#26680,#26681,#26682,#26683,#26684,#26685,#26686,#26687,
#26688,#26689,#26690,#26691,#26692,#26693),.UNSPECIFIED.,.F.,.F.,(4,3,3,
3,3,3,3,4),(-60.3950510283081,-59.84991932703,-58.8524206715795,-57.854922016129,
-56.8574233606785,-55.859924705228,-54.8624260497775,-54.1118657211285),
 .UNSPECIFIED.);
#609=B_SPLINE_CURVE_WITH_KNOTS('',3,(#26698,#26699,#26700,#26701,#26702,
#26703,#26704,#26705,#26706,#26707,#26708,#26709,#26710,#26711,#26712,#26713,
#26714,#26715,#26716,#26717,#26718,#26719,#26720,#26721,#26722),
 .UNSPECIFIED.,.F.,.F.,(4,3,3,3,3,3,3,3,4),(51.5753047126083,51.869930083426,
52.8674287388765,53.864927394327,54.8624260497775,55.859924705228,56.8574233606785,
57.854922016129,57.8584900197876),.UNSPECIFIED.);
#610=B_SPLINE_CURVE_WITH_KNOTS('',3,(#26723,#26724,#26725,#26726,#26727,
#26728,#26729,#26730,#26731,#26732,#26733,#26734,#26735,#26736,#26737,#26738,
#26739,#26740,#26741,#26742,#26743,#26744,#26745,#26746,#26747),
 .UNSPECIFIED.,.F.,.F.,(4,3,3,3,3,3,3,3,4),(-54.1118657211285,-53.864927394327,
-52.8674287388765,-51.869930083426,-50.8724314279755,-49.874932772525,-48.8774341170745,
-47.879935461624,-47.8286804139489),.UNSPECIFIED.);
#611=B_SPLINE_CURVE_WITH_KNOTS('',3,(#26752,#26753,#26754,#26755,#26756,
#26757,#26758,#26759,#26760,#26761,#26762,#26763,#26764,#26765,#26766,#26767,
#26768,#26769,#26770,#26771,#26772,#26773),.UNSPECIFIED.,.F.,.F.,(4,3,3,
3,3,3,3,4),(45.2921194054287,45.884938150723,46.8824368061735,47.879935461624,
48.8774341170745,49.874932772525,50.8724314279755,51.5753047126083),
 .UNSPECIFIED.);
#612=B_SPLINE_CURVE_WITH_KNOTS('',3,(#26774,#26775,#26776,#26777,#26778,
#26779,#26780,#26781,#26782,#26783,#26784,#26785,#26786,#26787,#26788,#26789,
#26790,#26791,#26792,#26793,#26794,#26795),.UNSPECIFIED.,.F.,.F.,(4,3,3,
3,3,3,3,4),(-47.8286804139489,-46.8824368061735,-45.884938150723,-44.8874394952725,
-43.889940839822,-42.8924421843715,-41.894943528921,-41.5454951067693),
 .UNSPECIFIED.);
#613=B_SPLINE_CURVE_WITH_KNOTS('',3,(#26800,#26801,#26802,#26803,#26804,
#26805,#26806,#26807,#26808,#26809,#26810,#26811,#26812,#26813,#26814,#26815,
#26816,#26817,#26818,#26819,#26820,#26821),.UNSPECIFIED.,.F.,.F.,(4,3,3,
3,3,3,3,4),(39.0089340982491,39.89994621802,40.8974448734705,41.894943528921,
42.8924421843715,43.889940839822,44.8874394952725,45.2921194054287),
 .UNSPECIFIED.);
#614=B_SPLINE_CURVE_WITH_KNOTS('',3,(#26822,#26823,#26824,#26825,#26826,
#26827,#26828,#26829,#26830,#26831,#26832,#26833,#26834,#26835,#26836,#26837,
#26838,#26839,#26840,#26841,#26842,#26843),.UNSPECIFIED.,.F.,.F.,(4,3,3,
3,3,3,3,4),(-41.5454951067693,-40.8974448734705,-39.89994621802,-38.9024475625695,
-37.904948907119,-36.9074502516685,-35.909951596218,-35.2623097995897),
 .UNSPECIFIED.);
#615=B_SPLINE_CURVE_WITH_KNOTS('',3,(#26848,#26849,#26850,#26851,#26852,
#26853,#26854,#26855,#26856,#26857,#26858,#26859,#26860,#26861,#26862,#26863,
#26864,#26865,#26866,#26867,#26868,#26869,#26870,#26871,#26872),
 .UNSPECIFIED.,.F.,.F.,(4,3,3,3,3,3,3,3,4),(32.7257487910695,32.9174556298665,
33.914954285317,34.9124529407675,35.909951596218,36.9074502516685,37.904948907119,
38.9024475625695,39.0089340982491),.UNSPECIFIED.);
#616=B_SPLINE_CURVE_WITH_KNOTS('',3,(#26873,#26874,#26875,#26876,#26877,
#26878,#26879,#26880,#26881,#26882,#26883,#26884,#26885,#26886,#26887,#26888,
#26889,#26890,#26891,#26892,#26893,#26894),.UNSPECIFIED.,.F.,.F.,(4,3,3,
3,3,3,3,4),(-35.2623097995897,-34.9124529407675,-33.914954285317,-32.9174556298665,
-31.919956974416,-30.9224583189655,-29.924959663515,-28.9791244924101),
 .UNSPECIFIED.);
#617=B_SPLINE_CURVE_WITH_KNOTS('',3,(#26899,#26900,#26901,#26902,#26903,
#26904,#26905,#26906,#26907,#26908,#26909,#26910,#26911,#26912,#26913,#26914,
#26915,#26916,#26917,#26918,#26919,#26920),.UNSPECIFIED.,.F.,.F.,(4,3,3,
3,3,3,3,4),(26.4425634838898,26.9324636971635,27.929962352614,28.9274610080645,
29.924959663515,30.9224583189655,31.919956974416,32.7257487910695),
 .UNSPECIFIED.);
#618=B_SPLINE_CURVE_WITH_KNOTS('',3,(#26921,#26922,#26923,#26924,#26925,
#26926,#26927,#26928,#26929,#26930,#26931,#26932,#26933,#26934,#26935,#26936,
#26937,#26938,#26939,#26940,#26941,#26942,#26943,#26944,#26945),
 .UNSPECIFIED.,.F.,.F.,(4,3,3,3,3,3,3,3,4),(-28.9791244924101,-28.9274610080645,
-27.929962352614,-26.9324636971635,-25.934965041713,-24.9374663862625,-23.939967730812,
-22.9424690753615,-22.6959391852305),.UNSPECIFIED.);
#619=B_SPLINE_CURVE_WITH_KNOTS('',3,(#26950,#26951,#26952,#26953,#26954,
#26955,#26956,#26957,#26958,#26959,#26960,#26961,#26962,#26963,#26964,#26965,
#26966,#26967,#26968,#26969,#26970,#26971),.UNSPECIFIED.,.F.,.F.,(4,3,3,
3,3,3,3,4),(20.1593781767102,20.9474717644605,21.944970419911,22.9424690753615,
23.939967730812,24.9374663862625,25.934965041713,26.4425634838898),
 .UNSPECIFIED.);
#620=B_SPLINE_CURVE_WITH_KNOTS('',3,(#26972,#26973,#26974,#26975,#26976,
#26977,#26978,#26979,#26980,#26981,#26982,#26983,#26984,#26985,#26986,#26987,
#26988,#26989,#26990,#26991,#26992,#26993),.UNSPECIFIED.,.F.,.F.,(4,3,3,
3,3,3,3,4),(-22.6959391852305,-21.944970419911,-20.9474717644605,-19.94997310901,
-18.9524744535595,-17.954975798109,-16.9574771426585,-16.4127538780512),
 .UNSPECIFIED.);
#621=B_SPLINE_CURVE_WITH_KNOTS('',3,(#26998,#26999,#27000,#27001,#27002,
#27003,#27004,#27005,#27006,#27007,#27008,#27009,#27010,#27011,#27012,#27013,
#27014,#27015,#27016,#27017,#27018,#27019,#27020,#27021,#27022),
 .UNSPECIFIED.,.F.,.F.,(4,3,3,3,3,3,3,3,4),(13.8761928695306,13.964981176307,
14.9624798317575,15.959978487208,16.9574771426585,17.954975798109,18.9524744535595,
19.94997310901,20.1593781767102),.UNSPECIFIED.);
#622=B_SPLINE_CURVE_WITH_KNOTS('',3,(#27023,#27024,#27025,#27026,#27027,
#27028,#27029,#27030,#27031,#27032,#27033,#27034,#27035,#27036,#27037,#27038,
#27039,#27040,#27041,#27042,#27043,#27044),.UNSPECIFIED.,.F.,.F.,(4,3,3,
3,3,3,3,4),(-16.4127538780512,-15.959978487208,-14.9624798317575,-13.964981176307,
-12.9674825208565,-11.969983865406,-10.9724852099555,-10.1295685708716),
 .UNSPECIFIED.);
#623=B_SPLINE_CURVE_WITH_KNOTS('',3,(#27050,#27051,#27052,#27053,#27054,
#27055,#27056,#27057,#27058,#27059,#27060,#27061,#27062),.UNSPECIFIED.,
 .F.,.F.,(4,3,3,3,4),(-3.84638326369194,-2.9924959663515,-1.994997310901,
-0.997498655450502,0.),.UNSPECIFIED.);
#624=B_SPLINE_CURVE_WITH_KNOTS('',3,(#27065,#27066,#27067,#27068,#27069,
#27070,#27071,#27072,#27073,#27074,#27075,#27076,#27077,#27078,#27079,#27080,
#27081,#27082,#27083),.UNSPECIFIED.,.F.,.F.,(4,3,3,3,3,3,4),(2.01461286527449,
2.9924959663515,3.989994621802,4.9874932772525,5.984991932703,6.9824905881535,
7.59300756235101),.UNSPECIFIED.);
#625=B_SPLINE_CURVE_WITH_KNOTS('',3,(#27089,#27090,#27091,#27092,#27093),
 .UNSPECIFIED.,.F.,.F.,(4,1,4),(128.805298797181,129.566421347416,130.563920002867),
 .UNSPECIFIED.);
#626=B_SPLINE_CURVE_WITH_KNOTS('',3,(#27096,#27097,#27098,#27099,#27100,
#27101),.UNSPECIFIED.,.F.,.F.,(4,1,1,4),(128.805298797181,129.110486389585,
130.107985045035,131.085868146112),.UNSPECIFIED.);
#627=B_SPLINE_CURVE_WITH_KNOTS('',3,(#27106,#27107,#27108,#27109,#27110,
#27111,#27112,#27113,#27114,#27115,#27116),.UNSPECIFIED.,.F.,.F.,(4,1,1,
1,1,1,1,1,4),(122.522113490002,122.583930759263,123.581429414713,124.578928070164,
125.576426725614,126.573925381065,127.571424036515,128.568922691966,128.805298797181),
 .UNSPECIFIED.);
#628=B_SPLINE_CURVE_WITH_KNOTS('',3,(#27117,#27118,#27119,#27120,#27121,
#27122,#27123,#27124,#27125,#27126),.UNSPECIFIED.,.F.,.F.,(4,1,1,1,1,1,
1,4),(122.522113490002,123.125494456882,124.122993112332,125.120491767783,
126.117990423233,127.115489078684,128.112987734134,128.805298797181),
 .UNSPECIFIED.);
#629=B_SPLINE_CURVE_WITH_KNOTS('',3,(#27131,#27132,#27133,#27134,#27135,
#27136,#27137,#27138,#27139,#27140),.UNSPECIFIED.,.F.,.F.,(4,1,1,1,1,1,
1,4),(116.238928182822,116.59893882656,117.59643748201,118.593936137461,
119.591434792911,120.588933448362,121.586432103812,122.522113490002),
 .UNSPECIFIED.);
#630=B_SPLINE_CURVE_WITH_KNOTS('',3,(#27141,#27142,#27143,#27144,#27145,
#27146,#27147,#27148,#27149,#27150),.UNSPECIFIED.,.F.,.F.,(4,1,1,1,1,1,
1,4),(116.238928182823,117.140502524179,118.138001179629,119.13549983508,
120.13299849053,121.130497145981,122.127995801431,122.522113490002),
 .UNSPECIFIED.);
#631=B_SPLINE_CURVE_WITH_KNOTS('',3,(#27155,#27156,#27157,#27158,#27159,
#27160,#27161,#27162,#27163,#27164),.UNSPECIFIED.,.F.,.F.,(4,1,1,1,1,1,
1,4),(109.955742875643,110.613946893857,111.611445549307,112.608944204758,
113.606442860208,114.603941515659,115.601440171109,116.238928182822),
 .UNSPECIFIED.);
#632=B_SPLINE_CURVE_WITH_KNOTS('',3,(#27165,#27166,#27167,#27168,#27169,
#27170,#27171,#27172,#27173,#27174,#27175),.UNSPECIFIED.,.F.,.F.,(4,1,1,
1,1,1,1,1,4),(109.955742875643,110.158011936025,111.155510591476,112.153009246926,
113.150507902377,114.148006557827,115.145505213278,116.143003868728,116.238928182823),
 .UNSPECIFIED.);
#633=B_SPLINE_CURVE_WITH_KNOTS('',3,(#27180,#27181,#27182,#27183,#27184,
#27185,#27186,#27187,#27188,#27189),.UNSPECIFIED.,.F.,.F.,(4,1,1,1,1,1,
1,4),(103.672557568463,104.628954961154,105.626453616604,106.623952272055,
107.621450927505,108.618949582956,109.616448238406,109.955742875643),
 .UNSPECIFIED.);
#634=B_SPLINE_CURVE_WITH_KNOTS('',3,(#27190,#27191,#27192,#27193,#27194,
#27195,#27196,#27197,#27198,#27199),.UNSPECIFIED.,.F.,.F.,(4,1,1,1,1,1,
1,4),(103.672557568463,104.173020003322,105.170518658773,106.168017314223,
107.165515969674,108.163014625124,109.160513280575,109.955742875643),
 .UNSPECIFIED.);
#635=B_SPLINE_CURVE_WITH_KNOTS('',3,(#27204,#27205,#27206,#27207,#27208,
#27209,#27210,#27211,#27212,#27213,#27214),.UNSPECIFIED.,.F.,.F.,(4,1,1,
1,1,1,1,1,4),(97.3893722612837,97.646464373,98.6439630284505,99.641461683901,
100.638960339352,101.636458994802,102.633957650253,103.631456305703,103.672557568463),
 .UNSPECIFIED.);
#636=B_SPLINE_CURVE_WITH_KNOTS('',3,(#27215,#27216,#27217,#27218,#27219,
#27220,#27221,#27222,#27223,#27224),.UNSPECIFIED.,.F.,.F.,(4,1,1,1,1,1,
1,4),(97.3893722612837,98.1880280706194,99.1855267260699,100.18302538152,
101.180524036971,102.178022692421,103.175521347872,103.672557568463),
 .UNSPECIFIED.);
#637=B_SPLINE_CURVE_WITH_KNOTS('',3,(#27229,#27230,#27231,#27232,#27233,
#27234,#27235,#27236,#27237,#27238),.UNSPECIFIED.,.F.,.F.,(4,1,1,1,1,1,
1,4),(91.106186954104,91.661472440297,92.6589710957475,93.656469751198,
94.6539684066485,95.651467062099,96.6489657175495,97.3893722612837),
 .UNSPECIFIED.);
#638=B_SPLINE_CURVE_WITH_KNOTS('',3,(#27239,#27240,#27241,#27242,#27243,
#27244,#27245,#27246,#27247,#27248,#27249),.UNSPECIFIED.,.F.,.F.,(4,1,1,
1,1,1,1,1,4),(91.106186954104,91.2055374824659,92.2030361379164,93.2005347933669,
94.1980334488174,95.1955321042679,96.1930307597184,97.1905294151689,97.3893722612837),
 .UNSPECIFIED.);
#639=B_SPLINE_CURVE_WITH_KNOTS('',3,(#27254,#27255,#27256,#27257,#27258,
#27259,#27260,#27261,#27262,#27263),.UNSPECIFIED.,.F.,.F.,(4,1,1,1,1,1,
1,4),(84.8230016469245,85.676480507594,86.6739791630445,87.671477818495,
88.6689764739455,89.666475129396,90.6639737848465,91.106186954104),
 .UNSPECIFIED.);
#640=B_SPLINE_CURVE_WITH_KNOTS('',3,(#27264,#27265,#27266,#27267,#27268,
#27269,#27270,#27271,#27272,#27273),.UNSPECIFIED.,.F.,.F.,(4,1,1,1,1,1,
1,4),(84.8230016469245,85.2205455497629,86.2180442052134,87.2155428606639,
88.2130415161144,89.2105401715649,90.2080388270154,91.106186954104),
 .UNSPECIFIED.);
#641=B_SPLINE_CURVE_WITH_KNOTS('',3,(#27278,#27279,#27280,#27281,#27282,
#27283,#27284,#27285,#27286,#27287,#27288),.UNSPECIFIED.,.F.,.F.,(4,1,1,
1,1,1,1,1,4),(78.5398163397448,78.6939899194405,79.691488574891,80.6889872303415,
81.686485885792,82.6839845412425,83.681483196693,84.6789818521435,84.8230016469245),
 .UNSPECIFIED.);
#642=B_SPLINE_CURVE_WITH_KNOTS('',3,(#27289,#27290,#27291,#27292,#27293,
#27294,#27295,#27296,#27297,#27298),.UNSPECIFIED.,.F.,.F.,(4,1,1,1,1,1,
1,4),(78.5398163397448,79.2355536170598,80.2330522725103,81.2305509279608,
82.2280495834113,83.2255482388618,84.2230468943123,84.8230016469245),
 .UNSPECIFIED.);
#643=B_SPLINE_CURVE_WITH_KNOTS('',3,(#27303,#27304,#27305,#27306,#27307,
#27308,#27309,#27310,#27311,#27312),.UNSPECIFIED.,.F.,.F.,(4,1,1,1,1,1,
1,4),(72.2566310325652,72.7089979867375,73.706496642188,74.7039952976385,
75.701493953089,76.6989926085395,77.69649126399,78.5398163397448),
 .UNSPECIFIED.);
#644=B_SPLINE_CURVE_WITH_KNOTS('',3,(#27313,#27314,#27315,#27316,#27317,
#27318,#27319,#27320,#27321,#27322),.UNSPECIFIED.,.F.,.F.,(4,1,1,1,1,1,
1,4),(72.2566310325652,73.2505616843569,74.2480603398074,75.2455589952579,
76.2430576507084,77.2405563061589,78.2380549616094,78.5398163397448),
 .UNSPECIFIED.);
#645=B_SPLINE_CURVE_WITH_KNOTS('',3,(#27327,#27328,#27329,#27330,#27331,
#27332,#27333,#27334,#27335,#27336),.UNSPECIFIED.,.F.,.F.,(4,1,1,1,1,1,
1,4),(65.9734457253856,66.7240060540345,67.721504709485,68.7190033649355,
69.716502020386,70.7140006758365,71.711499331287,72.2566310325652),
 .UNSPECIFIED.);
#646=B_SPLINE_CURVE_WITH_KNOTS('',3,(#27337,#27338,#27339,#27340,#27341,
#27342,#27343,#27344,#27345,#27346,#27347),.UNSPECIFIED.,.F.,.F.,(4,1,1,
1,1,1,1,1,4),(65.9734457253856,66.2680710962033,67.2655697516538,68.2630684071043,
69.2605670625549,70.2580657180054,71.2555643734559,72.2530630289064,72.2566310325652),
 .UNSPECIFIED.);
#647=B_SPLINE_CURVE_WITH_KNOTS('',3,(#27352,#27353,#27354,#27355,#27356,
#27357,#27358,#27359,#27360,#27361,#27362),.UNSPECIFIED.,.F.,.F.,(4,1,1,
1,1,1,1,1,4),(59.690260418206,59.741515465881,60.7390141213315,61.736512776782,
62.7340114322325,63.731510087683,64.7290087431335,65.726507398584,65.9734457253856),
 .UNSPECIFIED.);
#648=B_SPLINE_CURVE_WITH_KNOTS('',3,(#27363,#27364,#27365,#27366,#27367,
#27368,#27369,#27370,#27371,#27372),.UNSPECIFIED.,.F.,.F.,(4,1,1,1,1,1,
1,4),(59.690260418206,60.2830791635003,61.2805778189508,62.2780764744013,
63.2755751298518,64.2730737853023,65.2705724407528,65.9734457253856),
 .UNSPECIFIED.);
#649=B_SPLINE_CURVE_WITH_KNOTS('',3,(#27377,#27378,#27379,#27380,#27381,
#27382,#27383,#27384,#27385,#27386),.UNSPECIFIED.,.F.,.F.,(4,1,1,1,1,1,
1,4),(53.4070751110264,53.756523533178,54.7540221886285,55.751520844079,
56.7490194995295,57.74651815498,58.7440168104305,59.690260418206),
 .UNSPECIFIED.);
#650=B_SPLINE_CURVE_WITH_KNOTS('',3,(#27387,#27388,#27389,#27390,#27391,
#27392,#27393,#27394,#27395,#27396),.UNSPECIFIED.,.F.,.F.,(4,1,1,1,1,1,
1,4),(53.4070751110264,54.2980872307973,55.2955858862478,56.2930845416983,
57.2905831971488,58.2880818525993,59.2855805080498,59.690260418206),
 .UNSPECIFIED.);
#651=B_SPLINE_CURVE_WITH_KNOTS('',3,(#27401,#27402,#27403,#27404,#27405,
#27406,#27407,#27408,#27409,#27410),.UNSPECIFIED.,.F.,.F.,(4,1,1,1,1,1,
1,4),(47.1238898038468,47.771531600475,48.7690302559255,49.766528911376,
50.7640275668265,51.761526222277,52.7590248777275,53.4070751110264),
 .UNSPECIFIED.);
#652=B_SPLINE_CURVE_WITH_KNOTS('',3,(#27411,#27412,#27413,#27414,#27415,
#27416,#27417,#27418,#27419,#27420,#27421),.UNSPECIFIED.,.F.,.F.,(4,1,1,
1,1,1,1,1,4),(47.1238898038468,47.3155966426438,48.3130952980943,49.3105939535448,
50.3080926089953,51.3055912644458,52.3030899198963,53.3005885753468,53.4070751110264),
 .UNSPECIFIED.);
#653=B_SPLINE_CURVE_WITH_KNOTS('',3,(#27426,#27427,#27428,#27429,#27430,
#27431,#27432,#27433,#27434,#27435),.UNSPECIFIED.,.F.,.F.,(4,1,1,1,1,1,
1,4),(40.8407044966672,41.786539667772,42.7840383232225,43.781536978673,
44.7790356341235,45.776534289574,46.7740329450245,47.1238898038468),
 .UNSPECIFIED.);
#654=B_SPLINE_CURVE_WITH_KNOTS('',3,(#27436,#27437,#27438,#27439,#27440,
#27441,#27442,#27443,#27444,#27445),.UNSPECIFIED.,.F.,.F.,(4,1,1,1,1,1,
1,4),(40.8407044966672,41.3306047099408,42.3281033653913,43.3256020208418,
44.3231006762923,45.3205993317428,46.3180979871933,47.1238898038468),
 .UNSPECIFIED.);
#655=B_SPLINE_CURVE_WITH_KNOTS('',3,(#27450,#27451,#27452,#27453,#27454,
#27455,#27456,#27457,#27458,#27459,#27460),.UNSPECIFIED.,.F.,.F.,(4,1,1,
1,1,1,1,1,4),(34.5575191894876,34.8040490796185,35.801547735069,36.7990463905195,
37.79654504597,38.7940437014205,39.791542356871,40.7890410123215,40.8407044966672),
 .UNSPECIFIED.);
#656=B_SPLINE_CURVE_WITH_KNOTS('',3,(#27461,#27462,#27463,#27464,#27465,
#27466,#27467,#27468,#27469,#27470),.UNSPECIFIED.,.F.,.F.,(4,1,1,1,1,1,
1,4),(34.5575191894876,35.3456127772378,36.3431114326883,37.3406100881388,
38.3381087435893,39.3356073990398,40.3331060544903,40.8407044966672),
 .UNSPECIFIED.);
#657=B_SPLINE_CURVE_WITH_KNOTS('',3,(#27475,#27476,#27477,#27478,#27479,
#27480,#27481,#27482,#27483,#27484),.UNSPECIFIED.,.F.,.F.,(4,1,1,1,1,1,
1,4),(28.2743338823079,28.8190571469155,29.816555802366,30.8140544578165,
31.811553113267,32.8090517687175,33.806550424168,34.5575191894876),
 .UNSPECIFIED.);
#658=B_SPLINE_CURVE_WITH_KNOTS('',3,(#27485,#27486,#27487,#27488,#27489,
#27490,#27491,#27492,#27493,#27494,#27495),.UNSPECIFIED.,.F.,.F.,(4,1,1,
1,1,1,1,1,4),(28.2743338823079,28.3631221890843,29.3606208445348,30.3581194999853,
31.3556181554358,32.3531168108863,33.3506154663368,34.3481141217873,34.5575191894876),
 .UNSPECIFIED.);
#659=B_SPLINE_CURVE_WITH_KNOTS('',3,(#27500,#27501,#27502,#27503,#27504,
#27505,#27506,#27507,#27508,#27509),.UNSPECIFIED.,.F.,.F.,(4,1,1,1,1,1,
1,4),(21.9911485751283,22.8340652142125,23.831563869663,24.8290625251135,
25.826561180564,26.8240598360145,27.821558491465,28.2743338823079),
 .UNSPECIFIED.);
#660=B_SPLINE_CURVE_WITH_KNOTS('',3,(#27510,#27511,#27512,#27513,#27514,
#27515,#27516,#27517,#27518,#27519),.UNSPECIFIED.,.F.,.F.,(4,1,1,1,1,1,
1,4),(21.9911485751283,22.3781302563813,23.3756289118318,24.3731275672823,
25.3706262227328,26.3681248781833,27.3656235336338,28.2743338823079),
 .UNSPECIFIED.);
#661=B_SPLINE_CURVE_WITH_KNOTS('',3,(#27525,#27526,#27527,#27528,#27529),
 .UNSPECIFIED.,.F.,.F.,(4,1,4),(14.3981410127773,15.3956396682278,15.707963267949),
 .UNSPECIFIED.);
#662=B_SPLINE_CURVE_WITH_KNOTS('',3,(#27532,#27533,#27534,#27535,#27536),
 .UNSPECIFIED.,.F.,.F.,(4,1,4),(13.8761928695316,14.8540759706085,15.707963267949),
 .UNSPECIFIED.);
#663=B_SPLINE_CURVE_WITH_KNOTS('',3,(#27542,#27543,#27544,#27545,#27546,
#27547,#27548,#27549,#27550,#27551,#27552,#27553,#27554,#27555,#27556,#27557),
 .UNSPECIFIED.,.F.,.F.,(4,3,3,3,3,4),(114.407157784404,114.712345376808,
115.709844032258,116.707342687709,117.704841343159,118.702339998609),
 .UNSPECIFIED.);
#664=B_SPLINE_CURVE_WITH_KNOTS('',3,(#27565,#27566,#27567,#27568,#27569,
#27570,#27571,#27572,#27573,#27574,#27575,#27576,#27577,#27578,#27579,#27580,
#27581,#27582,#27583,#27584,#27585,#27586),.UNSPECIFIED.,.F.,.F.,(4,3,3,
3,3,3,3,4),(-116.687727133335,-115.709844032258,-114.712345376808,-113.714846721357,
-112.717348065907,-111.719849410456,-110.722350755006,-110.660533485745),
 .UNSPECIFIED.);
#665=B_SPLINE_CURVE_WITH_KNOTS('',3,(#27591,#27592,#27593,#27594,#27595,
#27596,#27597,#27598,#27599,#27600,#27601,#27602,#27603,#27604,#27605,#27606,
#27607,#27608,#27609,#27610,#27611,#27612),.UNSPECIFIED.,.F.,.F.,(4,3,3,
3,3,3,3,4),(108.123972477224,108.727353444105,109.724852099555,110.722350755006,
111.719849410456,112.717348065907,113.714846721357,114.407157784404),
 .UNSPECIFIED.);
#666=B_SPLINE_CURVE_WITH_KNOTS('',3,(#27613,#27614,#27615,#27616,#27617,
#27618,#27619,#27620,#27621,#27622,#27623,#27624,#27625,#27626,#27627,#27628,
#27629,#27630,#27631,#27632,#27633,#27634),.UNSPECIFIED.,.F.,.F.,(4,3,3,
3,3,3,3,4),(-110.660533485745,-109.724852099555,-108.727353444105,-107.729854788654,
-106.732356133204,-105.734857477753,-104.737358822303,-104.377348178565),
 .UNSPECIFIED.);
#667=B_SPLINE_CURVE_WITH_KNOTS('',3,(#27639,#27640,#27641,#27642,#27643,
#27644,#27645,#27646,#27647,#27648,#27649,#27650,#27651,#27652,#27653,#27654,
#27655,#27656,#27657,#27658,#27659,#27660),.UNSPECIFIED.,.F.,.F.,(4,3,3,
3,3,3,3,4),(101.840787170045,102.742361511402,103.739860166852,104.737358822303,
105.734857477753,106.732356133204,107.729854788654,108.123972477224),
 .UNSPECIFIED.);
#668=B_SPLINE_CURVE_WITH_KNOTS('',3,(#27661,#27662,#27663,#27664,#27665,
#27666,#27667,#27668,#27669,#27670,#27671,#27672,#27673,#27674,#27675,#27676,
#27677,#27678,#27679,#27680,#27681,#27682),.UNSPECIFIED.,.F.,.F.,(4,3,3,
3,3,3,3,4),(-104.377348178565,-103.739860166852,-102.742361511402,-101.744862855951,
-100.747364200501,-99.74986554505,-98.7523668895995,-98.0941628713858),
 .UNSPECIFIED.);
#669=B_SPLINE_CURVE_WITH_KNOTS('',3,(#27687,#27688,#27689,#27690,#27691,
#27692,#27693,#27694,#27695,#27696,#27697,#27698,#27699,#27700,#27701,#27702,
#27703,#27704,#27705,#27706,#27707,#27708,#27709,#27710,#27711),
 .UNSPECIFIED.,.F.,.F.,(4,3,3,3,3,3,3,3,4),(95.5576018628653,95.759870923248,
96.7573695786985,97.754868234149,98.7523668895996,99.7498655450501,100.747364200501,
101.744862855951,101.840787170045),.UNSPECIFIED.);
#670=B_SPLINE_CURVE_WITH_KNOTS('',3,(#27712,#27713,#27714,#27715,#27716,
#27717,#27718,#27719,#27720,#27721,#27722,#27723,#27724,#27725,#27726,#27727,
#27728,#27729,#27730,#27731,#27732,#27733),.UNSPECIFIED.,.F.,.F.,(4,3,3,
3,3,3,3,4),(-98.0941628713858,-97.754868234149,-96.7573695786985,-95.759870923248,
-94.7623722677975,-93.764873612347,-92.7673749568965,-91.8109775642062),
 .UNSPECIFIED.);
#671=B_SPLINE_CURVE_WITH_KNOTS('',3,(#27738,#27739,#27740,#27741,#27742,
#27743,#27744,#27745,#27746,#27747,#27748,#27749,#27750,#27751,#27752,#27753,
#27754,#27755,#27756,#27757,#27758,#27759),.UNSPECIFIED.,.F.,.F.,(4,3,3,
3,3,3,3,4),(89.2744165556857,89.774878990545,90.7723776459955,91.769876301446,
92.7673749568965,93.764873612347,94.7623722677975,95.5576018628653),
 .UNSPECIFIED.);
#672=B_SPLINE_CURVE_WITH_KNOTS('',3,(#27760,#27761,#27762,#27763,#27764,
#27765,#27766,#27767,#27768,#27769,#27770,#27771,#27772,#27773,#27774,#27775,
#27776,#27777,#27778,#27779,#27780,#27781,#27782,#27783,#27784),
 .UNSPECIFIED.,.F.,.F.,(4,3,3,3,3,3,3,3,4),(-91.8109775642062,-91.769876301446,
-90.7723776459955,-89.774878990545,-88.7773803350945,-87.779881679644,-86.7823830241935,
-85.784884368743,-85.5277922570266),.UNSPECIFIED.);
#673=B_SPLINE_CURVE_WITH_KNOTS('',3,(#27789,#27790,#27791,#27792,#27793,
#27794,#27795,#27796,#27797,#27798,#27799,#27800,#27801,#27802,#27803,#27804,
#27805,#27806,#27807,#27808,#27809,#27810),.UNSPECIFIED.,.F.,.F.,(4,3,3,
3,3,3,3,4),(82.9912312485061,83.7898870578421,84.7873857132926,85.7848843687431,
86.7823830241935,87.779881679644,88.7773803350946,89.2744165556857),
 .UNSPECIFIED.);
#674=B_SPLINE_CURVE_WITH_KNOTS('',3,(#27811,#27812,#27813,#27814,#27815,
#27816,#27817,#27818,#27819,#27820,#27821,#27822,#27823,#27824,#27825,#27826,
#27827,#27828,#27829,#27830,#27831,#27832),.UNSPECIFIED.,.F.,.F.,(4,3,3,
3,3,3,3,4),(-85.5277922570266,-84.7873857132925,-83.789887057842,-82.7923884023915,
-81.794889746941,-80.7973910914905,-79.79989243604,-79.244606949847),
 .UNSPECIFIED.);
#675=B_SPLINE_CURVE_WITH_KNOTS('',3,(#27837,#27838,#27839,#27840,#27841,
#27842,#27843,#27844,#27845,#27846,#27847,#27848,#27849,#27850,#27851,#27852,
#27853,#27854,#27855,#27856,#27857,#27858,#27859,#27860,#27861),
 .UNSPECIFIED.,.F.,.F.,(4,3,3,3,3,3,3,3,4),(76.7080459413264,76.8073964696885,
77.804895125139,78.8023937805895,79.79989243604,80.7973910914905,81.7948897469411,
82.7923884023915,82.9912312485061),.UNSPECIFIED.);
#676=B_SPLINE_CURVE_WITH_KNOTS('',3,(#27862,#27863,#27864,#27865,#27866,
#27867,#27868,#27869,#27870,#27871,#27872,#27873,#27874,#27875,#27876,#27877,
#27878,#27879,#27880,#27881,#27882,#27883),.UNSPECIFIED.,.F.,.F.,(4,3,3,
3,3,3,3,4),(-79.244606949847,-78.8023937805895,-77.804895125139,-76.8073964696885,
-75.809897814238,-74.8123991587875,-73.814900503337,-72.9614216426674),
 .UNSPECIFIED.);
#677=B_SPLINE_CURVE_WITH_KNOTS('',3,(#27888,#27889,#27890,#27891,#27892,
#27893,#27894,#27895,#27896,#27897,#27898,#27899,#27900,#27901,#27902,#27903,
#27904,#27905,#27906,#27907,#27908,#27909),.UNSPECIFIED.,.F.,.F.,(4,3,3,
3,3,3,3,4),(70.4248606341468,70.8224045369855,71.8199031924361,72.8174018478865,
73.814900503337,74.8123991587875,75.809897814238,76.7080459413264),
 .UNSPECIFIED.);
#678=B_SPLINE_CURVE_WITH_KNOTS('',3,(#27910,#27911,#27912,#27913,#27914,
#27915,#27916,#27917,#27918,#27919,#27920,#27921,#27922,#27923,#27924,#27925,
#27926,#27927,#27928,#27929,#27930,#27931,#27932,#27933,#27934),
 .UNSPECIFIED.,.F.,.F.,(4,3,3,3,3,3,3,3,4),(-72.9614216426674,-72.8174018478865,
-71.819903192436,-70.8224045369855,-69.824905881535,-68.8274072260845,-67.829908570634,
-66.8324099151835,-66.6782363354877),.UNSPECIFIED.);
#679=B_SPLINE_CURVE_WITH_KNOTS('',3,(#27939,#27940,#27941,#27942,#27943,
#27944,#27945,#27946,#27947,#27948,#27949,#27950,#27951,#27952,#27953,#27954,
#27955,#27956,#27957,#27958,#27959,#27960),.UNSPECIFIED.,.F.,.F.,(4,3,3,
3,3,3,3,4),(64.1416753269672,64.8374126042825,65.834911259733,66.8324099151835,
67.829908570634,68.8274072260845,69.824905881535,70.4248606341468),
 .UNSPECIFIED.);
#680=B_SPLINE_CURVE_WITH_KNOTS('',3,(#27961,#27962,#27963,#27964,#27965,
#27966,#27967,#27968,#27969,#27970,#27971,#27972,#27973,#27974,#27975,#27976,
#27977,#27978,#27979,#27980,#27981,#27982),.UNSPECIFIED.,.F.,.F.,(4,3,3,
3,3,3,3,4),(-66.6782363354877,-65.834911259733,-64.8374126042825,-63.839913948832,
-62.8424152933815,-61.844916637931,-60.8474179824805,-60.3950510283081),
 .UNSPECIFIED.);
#681=B_SPLINE_CURVE_WITH_KNOTS('',3,(#27987,#27988,#27989,#27990,#27991,
#27992,#27993,#27994,#27995,#27996,#27997,#27998,#27999,#28000,#28001,#28002,
#28003,#28004,#28005,#28006,#28007,#28008),.UNSPECIFIED.,.F.,.F.,(4,3,3,
3,3,3,3,4),(57.8584900197876,58.8524206715795,59.84991932703,60.8474179824805,
61.844916637931,62.8424152933815,63.839913948832,64.1416753269672),
 .UNSPECIFIED.);
#682=B_SPLINE_CURVE_WITH_KNOTS('',3,(#28009,#28010,#28011,#28012,#28013,
#28014,#28015,#28016,#28017,#28018,#28019,#28020,#28021,#28022,#28023,#28024,
#28025,#28026,#28027,#28028,#28029,#28030),.UNSPECIFIED.,.F.,.F.,(4,3,3,
3,3,3,3,4),(-60.3950510283081,-59.84991932703,-58.8524206715795,-57.854922016129,
-56.8574233606785,-55.859924705228,-54.8624260497775,-54.1118657211285),
 .UNSPECIFIED.);
#683=B_SPLINE_CURVE_WITH_KNOTS('',3,(#28035,#28036,#28037,#28038,#28039,
#28040,#28041,#28042,#28043,#28044,#28045,#28046,#28047,#28048,#28049,#28050,
#28051,#28052,#28053,#28054,#28055,#28056,#28057,#28058,#28059),
 .UNSPECIFIED.,.F.,.F.,(4,3,3,3,3,3,3,3,4),(51.5753047126083,51.869930083426,
52.8674287388765,53.864927394327,54.8624260497775,55.859924705228,56.8574233606785,
57.854922016129,57.8584900197876),.UNSPECIFIED.);
#684=B_SPLINE_CURVE_WITH_KNOTS('',3,(#28060,#28061,#28062,#28063,#28064,
#28065,#28066,#28067,#28068,#28069,#28070,#28071,#28072,#28073,#28074,#28075,
#28076,#28077,#28078,#28079,#28080,#28081,#28082,#28083,#28084),
 .UNSPECIFIED.,.F.,.F.,(4,3,3,3,3,3,3,3,4),(-54.1118657211285,-53.864927394327,
-52.8674287388765,-51.869930083426,-50.8724314279755,-49.874932772525,-48.8774341170745,
-47.879935461624,-47.8286804139489),.UNSPECIFIED.);
#685=B_SPLINE_CURVE_WITH_KNOTS('',3,(#28089,#28090,#28091,#28092,#28093,
#28094,#28095,#28096,#28097,#28098,#28099,#28100,#28101,#28102,#28103,#28104,
#28105,#28106,#28107,#28108,#28109,#28110),.UNSPECIFIED.,.F.,.F.,(4,3,3,
3,3,3,3,4),(45.2921194054287,45.884938150723,46.8824368061735,47.879935461624,
48.8774341170745,49.874932772525,50.8724314279755,51.5753047126083),
 .UNSPECIFIED.);
#686=B_SPLINE_CURVE_WITH_KNOTS('',3,(#28111,#28112,#28113,#28114,#28115,
#28116,#28117,#28118,#28119,#28120,#28121,#28122,#28123,#28124,#28125,#28126,
#28127,#28128,#28129,#28130,#28131,#28132),.UNSPECIFIED.,.F.,.F.,(4,3,3,
3,3,3,3,4),(-47.8286804139489,-46.8824368061735,-45.884938150723,-44.8874394952725,
-43.889940839822,-42.8924421843715,-41.894943528921,-41.5454951067693),
 .UNSPECIFIED.);
#687=B_SPLINE_CURVE_WITH_KNOTS('',3,(#28137,#28138,#28139,#28140,#28141,
#28142,#28143,#28144,#28145,#28146,#28147,#28148,#28149,#28150,#28151,#28152,
#28153,#28154,#28155,#28156,#28157,#28158),.UNSPECIFIED.,.F.,.F.,(4,3,3,
3,3,3,3,4),(39.0089340982491,39.89994621802,40.8974448734705,41.894943528921,
42.8924421843715,43.889940839822,44.8874394952725,45.2921194054287),
 .UNSPECIFIED.);
#688=B_SPLINE_CURVE_WITH_KNOTS('',3,(#28159,#28160,#28161,#28162,#28163,
#28164,#28165,#28166,#28167,#28168,#28169,#28170,#28171,#28172,#28173,#28174,
#28175,#28176,#28177,#28178,#28179,#28180),.UNSPECIFIED.,.F.,.F.,(4,3,3,
3,3,3,3,4),(-41.5454951067693,-40.8974448734705,-39.89994621802,-38.9024475625695,
-37.904948907119,-36.9074502516685,-35.909951596218,-35.2623097995897),
 .UNSPECIFIED.);
#689=B_SPLINE_CURVE_WITH_KNOTS('',3,(#28185,#28186,#28187,#28188,#28189,
#28190,#28191,#28192,#28193,#28194,#28195,#28196,#28197,#28198,#28199,#28200,
#28201,#28202,#28203,#28204,#28205,#28206,#28207,#28208,#28209),
 .UNSPECIFIED.,.F.,.F.,(4,3,3,3,3,3,3,3,4),(32.7257487910695,32.9174556298665,
33.914954285317,34.9124529407675,35.909951596218,36.9074502516685,37.904948907119,
38.9024475625695,39.0089340982491),.UNSPECIFIED.);
#690=B_SPLINE_CURVE_WITH_KNOTS('',3,(#28210,#28211,#28212,#28213,#28214,
#28215,#28216,#28217,#28218,#28219,#28220,#28221,#28222,#28223,#28224,#28225,
#28226,#28227,#28228,#28229,#28230,#28231),.UNSPECIFIED.,.F.,.F.,(4,3,3,
3,3,3,3,4),(-35.2623097995897,-34.9124529407675,-33.914954285317,-32.9174556298665,
-31.919956974416,-30.9224583189655,-29.924959663515,-28.9791244924101),
 .UNSPECIFIED.);
#691=B_SPLINE_CURVE_WITH_KNOTS('',3,(#28236,#28237,#28238,#28239,#28240,
#28241,#28242,#28243,#28244,#28245,#28246,#28247,#28248,#28249,#28250,#28251,
#28252,#28253,#28254,#28255,#28256,#28257),.UNSPECIFIED.,.F.,.F.,(4,3,3,
3,3,3,3,4),(26.4425634838898,26.9324636971635,27.929962352614,28.9274610080645,
29.924959663515,30.9224583189655,31.919956974416,32.7257487910695),
 .UNSPECIFIED.);
#692=B_SPLINE_CURVE_WITH_KNOTS('',3,(#28258,#28259,#28260,#28261,#28262,
#28263,#28264,#28265,#28266,#28267,#28268,#28269,#28270,#28271,#28272,#28273,
#28274,#28275,#28276,#28277,#28278,#28279,#28280,#28281,#28282),
 .UNSPECIFIED.,.F.,.F.,(4,3,3,3,3,3,3,3,4),(-28.9791244924101,-28.9274610080645,
-27.929962352614,-26.9324636971635,-25.934965041713,-24.9374663862625,-23.939967730812,
-22.9424690753615,-22.6959391852305),.UNSPECIFIED.);
#693=B_SPLINE_CURVE_WITH_KNOTS('',3,(#28287,#28288,#28289,#28290,#28291,
#28292,#28293,#28294,#28295,#28296,#28297,#28298,#28299,#28300,#28301,#28302,
#28303,#28304,#28305,#28306,#28307,#28308),.UNSPECIFIED.,.F.,.F.,(4,3,3,
3,3,3,3,4),(20.1593781767102,20.9474717644605,21.944970419911,22.9424690753615,
23.939967730812,24.9374663862625,25.934965041713,26.4425634838898),
 .UNSPECIFIED.);
#694=B_SPLINE_CURVE_WITH_KNOTS('',3,(#28309,#28310,#28311,#28312,#28313,
#28314,#28315,#28316,#28317,#28318,#28319,#28320,#28321,#28322,#28323,#28324,
#28325,#28326,#28327,#28328,#28329,#28330),.UNSPECIFIED.,.F.,.F.,(4,3,3,
3,3,3,3,4),(-22.6959391852305,-21.944970419911,-20.9474717644605,-19.94997310901,
-18.9524744535595,-17.954975798109,-16.9574771426585,-16.4127538780512),
 .UNSPECIFIED.);
#695=B_SPLINE_CURVE_WITH_KNOTS('',3,(#28335,#28336,#28337,#28338,#28339,
#28340,#28341,#28342,#28343,#28344,#28345,#28346,#28347,#28348,#28349,#28350,
#28351,#28352,#28353,#28354,#28355,#28356,#28357,#28358,#28359),
 .UNSPECIFIED.,.F.,.F.,(4,3,3,3,3,3,3,3,4),(13.8761928695306,13.964981176307,
14.9624798317575,15.959978487208,16.9574771426585,17.954975798109,18.9524744535595,
19.94997310901,20.1593781767102),.UNSPECIFIED.);
#696=B_SPLINE_CURVE_WITH_KNOTS('',3,(#28360,#28361,#28362,#28363,#28364,
#28365,#28366,#28367,#28368,#28369,#28370,#28371,#28372,#28373,#28374,#28375,
#28376,#28377,#28378,#28379,#28380,#28381),.UNSPECIFIED.,.F.,.F.,(4,3,3,
3,3,3,3,4),(-16.4127538780512,-15.959978487208,-14.9624798317575,-13.964981176307,
-12.9674825208565,-11.969983865406,-10.9724852099555,-10.1295685708716),
 .UNSPECIFIED.);
#697=B_SPLINE_CURVE_WITH_KNOTS('',3,(#28387,#28388,#28389,#28390,#28391,
#28392,#28393,#28394,#28395,#28396,#28397,#28398,#28399),.UNSPECIFIED.,
 .F.,.F.,(4,3,3,3,4),(-3.84638326369194,-2.9924959663515,-1.994997310901,
-0.997498655450501,0.),.UNSPECIFIED.);
#698=B_SPLINE_CURVE_WITH_KNOTS('',3,(#28402,#28403,#28404,#28405,#28406,
#28407,#28408,#28409,#28410,#28411,#28412,#28413,#28414,#28415,#28416,#28417,
#28418,#28419,#28420),.UNSPECIFIED.,.F.,.F.,(4,3,3,3,3,3,4),(2.01461286527449,
2.9924959663515,3.989994621802,4.9874932772525,5.984991932703,6.9824905881535,
7.59300756235101),.UNSPECIFIED.);
#699=B_SPLINE_CURVE_WITH_KNOTS('',3,(#28426,#28427,#28428,#28429,#28430),
 .UNSPECIFIED.,.F.,.F.,(4,1,4),(128.805298797181,129.566421347416,130.563920002867),
 .UNSPECIFIED.);
#700=B_SPLINE_CURVE_WITH_KNOTS('',3,(#28433,#28434,#28435,#28436,#28437,
#28438),.UNSPECIFIED.,.F.,.F.,(4,1,1,4),(128.805298797181,129.110486389585,
130.107985045035,131.085868146112),.UNSPECIFIED.);
#701=B_SPLINE_CURVE_WITH_KNOTS('',3,(#28443,#28444,#28445,#28446,#28447,
#28448,#28449,#28450,#28451,#28452,#28453),.UNSPECIFIED.,.F.,.F.,(4,1,1,
1,1,1,1,1,4),(122.522113490002,122.583930759263,123.581429414713,124.578928070164,
125.576426725614,126.573925381065,127.571424036515,128.568922691966,128.805298797181),
 .UNSPECIFIED.);
#702=B_SPLINE_CURVE_WITH_KNOTS('',3,(#28454,#28455,#28456,#28457,#28458,
#28459,#28460,#28461,#28462,#28463),.UNSPECIFIED.,.F.,.F.,(4,1,1,1,1,1,
1,4),(122.522113490002,123.125494456882,124.122993112332,125.120491767783,
126.117990423233,127.115489078684,128.112987734134,128.805298797181),
 .UNSPECIFIED.);
#703=B_SPLINE_CURVE_WITH_KNOTS('',3,(#28468,#28469,#28470,#28471,#28472,
#28473,#28474,#28475,#28476,#28477),.UNSPECIFIED.,.F.,.F.,(4,1,1,1,1,1,
1,4),(116.238928182822,116.59893882656,117.59643748201,118.593936137461,
119.591434792911,120.588933448362,121.586432103812,122.522113490002),
 .UNSPECIFIED.);
#704=B_SPLINE_CURVE_WITH_KNOTS('',3,(#28478,#28479,#28480,#28481,#28482,
#28483,#28484,#28485,#28486,#28487),.UNSPECIFIED.,.F.,.F.,(4,1,1,1,1,1,
1,4),(116.238928182823,117.140502524179,118.138001179629,119.13549983508,
120.13299849053,121.130497145981,122.127995801431,122.522113490002),
 .UNSPECIFIED.);
#705=B_SPLINE_CURVE_WITH_KNOTS('',3,(#28492,#28493,#28494,#28495,#28496,
#28497,#28498,#28499,#28500,#28501),.UNSPECIFIED.,.F.,.F.,(4,1,1,1,1,1,
1,4),(109.955742875643,110.613946893857,111.611445549307,112.608944204758,
113.606442860208,114.603941515659,115.601440171109,116.238928182822),
 .UNSPECIFIED.);
#706=B_SPLINE_CURVE_WITH_KNOTS('',3,(#28502,#28503,#28504,#28505,#28506,
#28507,#28508,#28509,#28510,#28511,#28512),.UNSPECIFIED.,.F.,.F.,(4,1,1,
1,1,1,1,1,4),(109.955742875643,110.158011936025,111.155510591476,112.153009246926,
113.150507902377,114.148006557827,115.145505213278,116.143003868728,116.238928182823),
 .UNSPECIFIED.);
#707=B_SPLINE_CURVE_WITH_KNOTS('',3,(#28517,#28518,#28519,#28520,#28521,
#28522,#28523,#28524,#28525,#28526),.UNSPECIFIED.,.F.,.F.,(4,1,1,1,1,1,
1,4),(103.672557568463,104.628954961154,105.626453616604,106.623952272055,
107.621450927505,108.618949582956,109.616448238406,109.955742875643),
 .UNSPECIFIED.);
#708=B_SPLINE_CURVE_WITH_KNOTS('',3,(#28527,#28528,#28529,#28530,#28531,
#28532,#28533,#28534,#28535,#28536),.UNSPECIFIED.,.F.,.F.,(4,1,1,1,1,1,
1,4),(103.672557568463,104.173020003322,105.170518658773,106.168017314223,
107.165515969674,108.163014625124,109.160513280575,109.955742875643),
 .UNSPECIFIED.);
#709=B_SPLINE_CURVE_WITH_KNOTS('',3,(#28541,#28542,#28543,#28544,#28545,
#28546,#28547,#28548,#28549,#28550,#28551),.UNSPECIFIED.,.F.,.F.,(4,1,1,
1,1,1,1,1,4),(97.3893722612837,97.646464373,98.6439630284505,99.641461683901,
100.638960339352,101.636458994802,102.633957650253,103.631456305703,103.672557568463),
 .UNSPECIFIED.);
#710=B_SPLINE_CURVE_WITH_KNOTS('',3,(#28552,#28553,#28554,#28555,#28556,
#28557,#28558,#28559,#28560,#28561),.UNSPECIFIED.,.F.,.F.,(4,1,1,1,1,1,
1,4),(97.3893722612837,98.1880280706194,99.1855267260699,100.18302538152,
101.180524036971,102.178022692421,103.175521347872,103.672557568463),
 .UNSPECIFIED.);
#711=B_SPLINE_CURVE_WITH_KNOTS('',3,(#28566,#28567,#28568,#28569,#28570,
#28571,#28572,#28573,#28574,#28575),.UNSPECIFIED.,.F.,.F.,(4,1,1,1,1,1,
1,4),(91.106186954104,91.661472440297,92.6589710957475,93.656469751198,
94.6539684066485,95.651467062099,96.6489657175495,97.3893722612837),
 .UNSPECIFIED.);
#712=B_SPLINE_CURVE_WITH_KNOTS('',3,(#28576,#28577,#28578,#28579,#28580,
#28581,#28582,#28583,#28584,#28585,#28586),.UNSPECIFIED.,.F.,.F.,(4,1,1,
1,1,1,1,1,4),(91.106186954104,91.2055374824659,92.2030361379164,93.2005347933669,
94.1980334488174,95.1955321042679,96.1930307597184,97.1905294151689,97.3893722612837),
 .UNSPECIFIED.);
#713=B_SPLINE_CURVE_WITH_KNOTS('',3,(#28591,#28592,#28593,#28594,#28595,
#28596,#28597,#28598,#28599,#28600),.UNSPECIFIED.,.F.,.F.,(4,1,1,1,1,1,
1,4),(84.8230016469245,85.676480507594,86.6739791630445,87.671477818495,
88.6689764739455,89.666475129396,90.6639737848465,91.106186954104),
 .UNSPECIFIED.);
#714=B_SPLINE_CURVE_WITH_KNOTS('',3,(#28601,#28602,#28603,#28604,#28605,
#28606,#28607,#28608,#28609,#28610),.UNSPECIFIED.,.F.,.F.,(4,1,1,1,1,1,
1,4),(84.8230016469245,85.2205455497629,86.2180442052134,87.2155428606639,
88.2130415161144,89.2105401715649,90.2080388270154,91.106186954104),
 .UNSPECIFIED.);
#715=B_SPLINE_CURVE_WITH_KNOTS('',3,(#28615,#28616,#28617,#28618,#28619,
#28620,#28621,#28622,#28623,#28624,#28625),.UNSPECIFIED.,.F.,.F.,(4,1,1,
1,1,1,1,1,4),(78.5398163397448,78.6939899194405,79.691488574891,80.6889872303415,
81.686485885792,82.6839845412425,83.681483196693,84.6789818521435,84.8230016469245),
 .UNSPECIFIED.);
#716=B_SPLINE_CURVE_WITH_KNOTS('',3,(#28626,#28627,#28628,#28629,#28630,
#28631,#28632,#28633,#28634,#28635),.UNSPECIFIED.,.F.,.F.,(4,1,1,1,1,1,
1,4),(78.5398163397448,79.2355536170598,80.2330522725103,81.2305509279608,
82.2280495834113,83.2255482388618,84.2230468943123,84.8230016469245),
 .UNSPECIFIED.);
#717=B_SPLINE_CURVE_WITH_KNOTS('',3,(#28640,#28641,#28642,#28643,#28644,
#28645,#28646,#28647,#28648,#28649),.UNSPECIFIED.,.F.,.F.,(4,1,1,1,1,1,
1,4),(72.2566310325652,72.7089979867375,73.706496642188,74.7039952976385,
75.701493953089,76.6989926085395,77.69649126399,78.5398163397448),
 .UNSPECIFIED.);
#718=B_SPLINE_CURVE_WITH_KNOTS('',3,(#28650,#28651,#28652,#28653,#28654,
#28655,#28656,#28657,#28658,#28659),.UNSPECIFIED.,.F.,.F.,(4,1,1,1,1,1,
1,4),(72.2566310325652,73.2505616843569,74.2480603398074,75.2455589952579,
76.2430576507084,77.2405563061589,78.2380549616094,78.5398163397448),
 .UNSPECIFIED.);
#719=B_SPLINE_CURVE_WITH_KNOTS('',3,(#28664,#28665,#28666,#28667,#28668,
#28669,#28670,#28671,#28672,#28673),.UNSPECIFIED.,.F.,.F.,(4,1,1,1,1,1,
1,4),(65.9734457253856,66.7240060540345,67.721504709485,68.7190033649355,
69.716502020386,70.7140006758365,71.711499331287,72.2566310325652),
 .UNSPECIFIED.);
#720=B_SPLINE_CURVE_WITH_KNOTS('',3,(#28674,#28675,#28676,#28677,#28678,
#28679,#28680,#28681,#28682,#28683,#28684),.UNSPECIFIED.,.F.,.F.,(4,1,1,
1,1,1,1,1,4),(65.9734457253856,66.2680710962033,67.2655697516538,68.2630684071043,
69.2605670625549,70.2580657180054,71.2555643734559,72.2530630289064,72.2566310325652),
 .UNSPECIFIED.);
#721=B_SPLINE_CURVE_WITH_KNOTS('',3,(#28689,#28690,#28691,#28692,#28693,
#28694,#28695,#28696,#28697,#28698,#28699),.UNSPECIFIED.,.F.,.F.,(4,1,1,
1,1,1,1,1,4),(59.690260418206,59.741515465881,60.7390141213315,61.736512776782,
62.7340114322325,63.731510087683,64.7290087431335,65.726507398584,65.9734457253856),
 .UNSPECIFIED.);
#722=B_SPLINE_CURVE_WITH_KNOTS('',3,(#28700,#28701,#28702,#28703,#28704,
#28705,#28706,#28707,#28708,#28709),.UNSPECIFIED.,.F.,.F.,(4,1,1,1,1,1,
1,4),(59.690260418206,60.2830791635003,61.2805778189508,62.2780764744013,
63.2755751298518,64.2730737853023,65.2705724407528,65.9734457253856),
 .UNSPECIFIED.);
#723=B_SPLINE_CURVE_WITH_KNOTS('',3,(#28714,#28715,#28716,#28717,#28718,
#28719,#28720,#28721,#28722,#28723),.UNSPECIFIED.,.F.,.F.,(4,1,1,1,1,1,
1,4),(53.4070751110264,53.756523533178,54.7540221886285,55.751520844079,
56.7490194995295,57.74651815498,58.7440168104305,59.690260418206),
 .UNSPECIFIED.);
#724=B_SPLINE_CURVE_WITH_KNOTS('',3,(#28724,#28725,#28726,#28727,#28728,
#28729,#28730,#28731,#28732,#28733),.UNSPECIFIED.,.F.,.F.,(4,1,1,1,1,1,
1,4),(53.4070751110264,54.2980872307973,55.2955858862478,56.2930845416983,
57.2905831971488,58.2880818525993,59.2855805080498,59.690260418206),
 .UNSPECIFIED.);
#725=B_SPLINE_CURVE_WITH_KNOTS('',3,(#28738,#28739,#28740,#28741,#28742,
#28743,#28744,#28745,#28746,#28747),.UNSPECIFIED.,.F.,.F.,(4,1,1,1,1,1,
1,4),(47.1238898038468,47.771531600475,48.7690302559255,49.766528911376,
50.7640275668265,51.761526222277,52.7590248777275,53.4070751110264),
 .UNSPECIFIED.);
#726=B_SPLINE_CURVE_WITH_KNOTS('',3,(#28748,#28749,#28750,#28751,#28752,
#28753,#28754,#28755,#28756,#28757,#28758),.UNSPECIFIED.,.F.,.F.,(4,1,1,
1,1,1,1,1,4),(47.1238898038468,47.3155966426438,48.3130952980943,49.3105939535448,
50.3080926089953,51.3055912644458,52.3030899198963,53.3005885753468,53.4070751110264),
 .UNSPECIFIED.);
#727=B_SPLINE_CURVE_WITH_KNOTS('',3,(#28763,#28764,#28765,#28766,#28767,
#28768,#28769,#28770,#28771,#28772),.UNSPECIFIED.,.F.,.F.,(4,1,1,1,1,1,
1,4),(40.8407044966672,41.786539667772,42.7840383232225,43.781536978673,
44.7790356341235,45.776534289574,46.7740329450245,47.1238898038468),
 .UNSPECIFIED.);
#728=B_SPLINE_CURVE_WITH_KNOTS('',3,(#28773,#28774,#28775,#28776,#28777,
#28778,#28779,#28780,#28781,#28782),.UNSPECIFIED.,.F.,.F.,(4,1,1,1,1,1,
1,4),(40.8407044966672,41.3306047099408,42.3281033653913,43.3256020208418,
44.3231006762923,45.3205993317428,46.3180979871933,47.1238898038468),
 .UNSPECIFIED.);
#729=B_SPLINE_CURVE_WITH_KNOTS('',3,(#28787,#28788,#28789,#28790,#28791,
#28792,#28793,#28794,#28795,#28796,#28797),.UNSPECIFIED.,.F.,.F.,(4,1,1,
1,1,1,1,1,4),(34.5575191894876,34.8040490796185,35.801547735069,36.7990463905195,
37.79654504597,38.7940437014205,39.791542356871,40.7890410123215,40.8407044966672),
 .UNSPECIFIED.);
#730=B_SPLINE_CURVE_WITH_KNOTS('',3,(#28798,#28799,#28800,#28801,#28802,
#28803,#28804,#28805,#28806,#28807),.UNSPECIFIED.,.F.,.F.,(4,1,1,1,1,1,
1,4),(34.5575191894876,35.3456127772378,36.3431114326883,37.3406100881388,
38.3381087435893,39.3356073990398,40.3331060544903,40.8407044966672),
 .UNSPECIFIED.);
#731=B_SPLINE_CURVE_WITH_KNOTS('',3,(#28812,#28813,#28814,#28815,#28816,
#28817,#28818,#28819,#28820,#28821),.UNSPECIFIED.,.F.,.F.,(4,1,1,1,1,1,
1,4),(28.2743338823079,28.8190571469155,29.816555802366,30.8140544578165,
31.811553113267,32.8090517687175,33.806550424168,34.5575191894876),
 .UNSPECIFIED.);
#732=B_SPLINE_CURVE_WITH_KNOTS('',3,(#28822,#28823,#28824,#28825,#28826,
#28827,#28828,#28829,#28830,#28831,#28832),.UNSPECIFIED.,.F.,.F.,(4,1,1,
1,1,1,1,1,4),(28.2743338823079,28.3631221890843,29.3606208445348,30.3581194999853,
31.3556181554358,32.3531168108863,33.3506154663368,34.3481141217873,34.5575191894876),
 .UNSPECIFIED.);
#733=B_SPLINE_CURVE_WITH_KNOTS('',3,(#28837,#28838,#28839,#28840,#28841,
#28842,#28843,#28844,#28845,#28846),.UNSPECIFIED.,.F.,.F.,(4,1,1,1,1,1,
1,4),(21.9911485751283,22.8340652142125,23.831563869663,24.8290625251135,
25.826561180564,26.8240598360145,27.821558491465,28.2743338823079),
 .UNSPECIFIED.);
#734=B_SPLINE_CURVE_WITH_KNOTS('',3,(#28847,#28848,#28849,#28850,#28851,
#28852,#28853,#28854,#28855,#28856),.UNSPECIFIED.,.F.,.F.,(4,1,1,1,1,1,
1,4),(21.9911485751283,22.3781302563813,23.3756289118318,24.3731275672823,
25.3706262227328,26.3681248781833,27.3656235336338,28.2743338823079),
 .UNSPECIFIED.);
#735=B_SPLINE_CURVE_WITH_KNOTS('',3,(#28862,#28863,#28864,#28865,#28866),
 .UNSPECIFIED.,.F.,.F.,(4,1,4),(14.3981410127773,15.3956396682278,15.707963267949),
 .UNSPECIFIED.);
#736=B_SPLINE_CURVE_WITH_KNOTS('',3,(#28869,#28870,#28871,#28872,#28873),
 .UNSPECIFIED.,.F.,.F.,(4,1,4),(13.8761928695316,14.8540759706085,15.707963267949),
 .UNSPECIFIED.);
#737=B_SPLINE_CURVE_WITH_KNOTS('',3,(#28879,#28880,#28881,#28882,#28883,
#28884,#28885,#28886,#28887,#28888,#28889,#28890,#28891,#28892,#28893,#28894),
 .UNSPECIFIED.,.F.,.F.,(4,3,3,3,3,4),(114.407157784404,114.712345376808,
115.709844032258,116.707342687709,117.704841343159,118.702339998609),
 .UNSPECIFIED.);
#738=B_SPLINE_CURVE_WITH_KNOTS('',3,(#28902,#28903,#28904,#28905,#28906,
#28907,#28908,#28909,#28910,#28911,#28912,#28913,#28914,#28915,#28916,#28917,
#28918,#28919,#28920,#28921,#28922,#28923),.UNSPECIFIED.,.F.,.F.,(4,3,3,
3,3,3,3,4),(-116.687727133335,-115.709844032258,-114.712345376807,-113.714846721357,
-112.717348065906,-111.719849410456,-110.722350755005,-110.660533485745),
 .UNSPECIFIED.);
#739=B_SPLINE_CURVE_WITH_KNOTS('',3,(#28928,#28929,#28930,#28931,#28932,
#28933,#28934,#28935,#28936,#28937,#28938,#28939,#28940,#28941,#28942,#28943,
#28944,#28945,#28946,#28947,#28948,#28949),.UNSPECIFIED.,.F.,.F.,(4,3,3,
3,3,3,3,4),(108.123972477225,108.727353444105,109.724852099555,110.722350755006,
111.719849410456,112.717348065907,113.714846721357,114.407157784404),
 .UNSPECIFIED.);
#740=B_SPLINE_CURVE_WITH_KNOTS('',3,(#28950,#28951,#28952,#28953,#28954,
#28955,#28956,#28957,#28958,#28959,#28960,#28961,#28962,#28963,#28964,#28965,
#28966,#28967,#28968,#28969,#28970,#28971),.UNSPECIFIED.,.F.,.F.,(4,3,3,
3,3,3,3,4),(-110.660533485745,-109.724852099555,-108.727353444105,-107.729854788654,
-106.732356133204,-105.734857477753,-104.737358822303,-104.377348178566),
 .UNSPECIFIED.);
#741=B_SPLINE_CURVE_WITH_KNOTS('',3,(#28976,#28977,#28978,#28979,#28980,
#28981,#28982,#28983,#28984,#28985,#28986,#28987,#28988,#28989,#28990,#28991,
#28992,#28993,#28994,#28995,#28996,#28997),.UNSPECIFIED.,.F.,.F.,(4,3,3,
3,3,3,3,4),(101.840787170045,102.742361511402,103.739860166852,104.737358822303,
105.734857477753,106.732356133204,107.729854788654,108.123972477225),
 .UNSPECIFIED.);
#742=B_SPLINE_CURVE_WITH_KNOTS('',3,(#28998,#28999,#29000,#29001,#29002,
#29003,#29004,#29005,#29006,#29007,#29008,#29009,#29010,#29011,#29012,#29013,
#29014,#29015,#29016,#29017,#29018,#29019),.UNSPECIFIED.,.F.,.F.,(4,3,3,
3,3,3,3,4),(-104.377348178566,-103.739860166852,-102.742361511402,-101.744862855951,
-100.747364200501,-99.74986554505,-98.7523668895995,-98.0941628713861),
 .UNSPECIFIED.);
#743=B_SPLINE_CURVE_WITH_KNOTS('',3,(#29024,#29025,#29026,#29027,#29028,
#29029,#29030,#29031,#29032,#29033,#29034,#29035,#29036,#29037,#29038,#29039,
#29040,#29041,#29042,#29043,#29044,#29045,#29046,#29047,#29048),
 .UNSPECIFIED.,.F.,.F.,(4,3,3,3,3,3,3,3,4),(95.5576018628656,95.7598709232481,
96.7573695786986,97.7548682341491,98.7523668895996,99.7498655450501,100.747364200501,
101.744862855951,101.840787170045),.UNSPECIFIED.);
#744=B_SPLINE_CURVE_WITH_KNOTS('',3,(#29049,#29050,#29051,#29052,#29053,
#29054,#29055,#29056,#29057,#29058,#29059,#29060,#29061,#29062,#29063,#29064,
#29065,#29066,#29067,#29068,#29069,#29070),.UNSPECIFIED.,.F.,.F.,(4,3,3,
3,3,3,3,4),(-98.0941628713861,-97.754868234149,-96.7573695786985,-95.759870923248,
-94.7623722677975,-93.764873612347,-92.7673749568965,-91.8109775642065),
 .UNSPECIFIED.);
#745=B_SPLINE_CURVE_WITH_KNOTS('',3,(#29075,#29076,#29077,#29078,#29079,
#29080,#29081,#29082,#29083,#29084,#29085,#29086,#29087,#29088,#29089,#29090,
#29091,#29092,#29093,#29094,#29095,#29096),.UNSPECIFIED.,.F.,.F.,(4,3,3,
3,3,3,3,4),(89.274416555686,89.774878990545,90.7723776459956,91.7698763014461,
92.7673749568966,93.764873612347,94.7623722677975,95.5576018628656),
 .UNSPECIFIED.);
#746=B_SPLINE_CURVE_WITH_KNOTS('',3,(#29097,#29098,#29099,#29100,#29101,
#29102,#29103,#29104,#29105,#29106,#29107,#29108,#29109,#29110,#29111,#29112,
#29113,#29114,#29115,#29116,#29117,#29118,#29119,#29120,#29121),
 .UNSPECIFIED.,.F.,.F.,(4,3,3,3,3,3,3,3,4),(-91.8109775642065,-91.769876301446,
-90.7723776459955,-89.774878990545,-88.7773803350945,-87.779881679644,-86.7823830241935,
-85.784884368743,-85.5277922570269),.UNSPECIFIED.);
#747=B_SPLINE_CURVE_WITH_KNOTS('',3,(#29126,#29127,#29128,#29129,#29130,
#29131,#29132,#29133,#29134,#29135,#29136,#29137,#29138,#29139,#29140,#29141,
#29142,#29143,#29144,#29145,#29146,#29147),.UNSPECIFIED.,.F.,.F.,(4,3,3,
3,3,3,3,4),(82.9912312485064,83.7898870578421,84.7873857132926,85.7848843687431,
86.7823830241936,87.7798816796441,88.7773803350946,89.274416555686),
 .UNSPECIFIED.);
#748=B_SPLINE_CURVE_WITH_KNOTS('',3,(#29148,#29149,#29150,#29151,#29152,
#29153,#29154,#29155,#29156,#29157,#29158,#29159,#29160,#29161,#29162,#29163,
#29164,#29165,#29166,#29167,#29168,#29169),.UNSPECIFIED.,.F.,.F.,(4,3,3,
3,3,3,3,4),(-85.5277922570269,-84.7873857132925,-83.789887057842,-82.7923884023915,
-81.794889746941,-80.7973910914905,-79.79989243604,-79.2446069498473),
 .UNSPECIFIED.);
#749=B_SPLINE_CURVE_WITH_KNOTS('',3,(#29174,#29175,#29176,#29177,#29178,
#29179,#29180,#29181,#29182,#29183,#29184,#29185,#29186,#29187,#29188,#29189,
#29190,#29191,#29192,#29193,#29194,#29195,#29196,#29197,#29198),
 .UNSPECIFIED.,.F.,.F.,(4,3,3,3,3,3,3,3,4),(76.7080459413267,76.8073964696886,
77.8048951251391,78.8023937805896,79.7998924360401,80.7973910914905,81.7948897469411,
82.7923884023916,82.9912312485064),.UNSPECIFIED.);
#750=B_SPLINE_CURVE_WITH_KNOTS('',3,(#29199,#29200,#29201,#29202,#29203,
#29204,#29205,#29206,#29207,#29208,#29209,#29210,#29211,#29212,#29213,#29214,
#29215,#29216,#29217,#29218,#29219,#29220),.UNSPECIFIED.,.F.,.F.,(4,3,3,
3,3,3,3,4),(-79.2446069498473,-78.8023937805895,-77.804895125139,-76.8073964696885,
-75.809897814238,-74.8123991587875,-73.814900503337,-72.9614216426677),
 .UNSPECIFIED.);
#751=B_SPLINE_CURVE_WITH_KNOTS('',3,(#29225,#29226,#29227,#29228,#29229,
#29230,#29231,#29232,#29233,#29234,#29235,#29236,#29237,#29238,#29239,#29240,
#29241,#29242,#29243,#29244,#29245,#29246),.UNSPECIFIED.,.F.,.F.,(4,3,3,
3,3,3,3,4),(70.4248606341471,70.8224045369855,71.819903192436,72.8174018478866,
73.814900503337,74.8123991587875,75.8098978142381,76.7080459413267),
 .UNSPECIFIED.);
#752=B_SPLINE_CURVE_WITH_KNOTS('',3,(#29247,#29248,#29249,#29250,#29251,
#29252,#29253,#29254,#29255,#29256,#29257,#29258,#29259,#29260,#29261,#29262,
#29263,#29264,#29265,#29266,#29267,#29268,#29269,#29270,#29271),
 .UNSPECIFIED.,.F.,.F.,(4,3,3,3,3,3,3,3,4),(-72.9614216426677,-72.8174018478865,
-71.819903192436,-70.8224045369855,-69.824905881535,-68.8274072260845,-67.829908570634,
-66.8324099151835,-66.6782363354881),.UNSPECIFIED.);
#753=B_SPLINE_CURVE_WITH_KNOTS('',3,(#29276,#29277,#29278,#29279,#29280,
#29281,#29282,#29283,#29284,#29285,#29286,#29287,#29288,#29289,#29290,#29291,
#29292,#29293,#29294,#29295,#29296,#29297),.UNSPECIFIED.,.F.,.F.,(4,3,3,
3,3,3,3,4),(64.1416753269675,64.8374126042825,65.834911259733,66.8324099151835,
67.829908570634,68.8274072260845,69.824905881535,70.4248606341471),
 .UNSPECIFIED.);
#754=B_SPLINE_CURVE_WITH_KNOTS('',3,(#29298,#29299,#29300,#29301,#29302,
#29303,#29304,#29305,#29306,#29307,#29308,#29309,#29310,#29311,#29312,#29313,
#29314,#29315,#29316,#29317,#29318,#29319),.UNSPECIFIED.,.F.,.F.,(4,3,3,
3,3,3,3,4),(-66.6782363354881,-65.834911259733,-64.8374126042825,-63.839913948832,
-62.8424152933815,-61.844916637931,-60.8474179824805,-60.3950510283085),
 .UNSPECIFIED.);
#755=B_SPLINE_CURVE_WITH_KNOTS('',3,(#29324,#29325,#29326,#29327,#29328,
#29329,#29330,#29331,#29332,#29333,#29334,#29335,#29336,#29337,#29338,#29339,
#29340,#29341,#29342,#29343,#29344,#29345),.UNSPECIFIED.,.F.,.F.,(4,3,3,
3,3,3,3,4),(57.8584900197882,58.8524206715795,59.84991932703,60.8474179824806,
61.844916637931,62.8424152933815,63.839913948832,64.1416753269675),
 .UNSPECIFIED.);
#756=B_SPLINE_CURVE_WITH_KNOTS('',3,(#29346,#29347,#29348,#29349,#29350,
#29351,#29352,#29353,#29354,#29355,#29356,#29357,#29358,#29359,#29360,#29361,
#29362,#29363,#29364,#29365,#29366,#29367),.UNSPECIFIED.,.F.,.F.,(4,3,3,
3,3,3,3,4),(-60.3950510283085,-59.84991932703,-58.8524206715795,-57.854922016129,
-56.8574233606785,-55.859924705228,-54.8624260497775,-54.1118657211288),
 .UNSPECIFIED.);
#757=B_SPLINE_CURVE_WITH_KNOTS('',3,(#29372,#29373,#29374,#29375,#29376,
#29377,#29378,#29379,#29380,#29381,#29382,#29383,#29384,#29385,#29386,#29387,
#29388,#29389,#29390,#29391,#29392,#29393,#29394,#29395,#29396),
 .UNSPECIFIED.,.F.,.F.,(4,3,3,3,3,3,3,3,4),(51.5753047126086,51.869930083426,
52.8674287388765,53.864927394327,54.8624260497775,55.859924705228,56.8574233606785,
57.8549220161291,57.8584900197882),.UNSPECIFIED.);
#758=B_SPLINE_CURVE_WITH_KNOTS('',3,(#29397,#29398,#29399,#29400,#29401,
#29402,#29403,#29404,#29405,#29406,#29407,#29408,#29409,#29410,#29411,#29412,
#29413,#29414,#29415,#29416,#29417,#29418,#29419,#29420,#29421),
 .UNSPECIFIED.,.F.,.F.,(4,3,3,3,3,3,3,3,4),(-54.1118657211288,-53.864927394327,
-52.8674287388765,-51.869930083426,-50.8724314279755,-49.874932772525,-48.8774341170745,
-47.879935461624,-47.8286804139492),.UNSPECIFIED.);
#759=B_SPLINE_CURVE_WITH_KNOTS('',3,(#29426,#29427,#29428,#29429,#29430,
#29431,#29432,#29433,#29434,#29435,#29436,#29437,#29438,#29439,#29440,#29441,
#29442,#29443,#29444,#29445,#29446,#29447),.UNSPECIFIED.,.F.,.F.,(4,3,3,
3,3,3,3,4),(45.292119405429,45.884938150723,46.8824368061735,47.879935461624,
48.8774341170745,49.874932772525,50.8724314279755,51.5753047126086),
 .UNSPECIFIED.);
#760=B_SPLINE_CURVE_WITH_KNOTS('',3,(#29448,#29449,#29450,#29451,#29452,
#29453,#29454,#29455,#29456,#29457,#29458,#29459,#29460,#29461,#29462,#29463,
#29464,#29465,#29466,#29467,#29468,#29469),.UNSPECIFIED.,.F.,.F.,(4,3,3,
3,3,3,3,4),(-47.8286804139492,-46.8824368061735,-45.884938150723,-44.8874394952725,
-43.889940839822,-42.8924421843715,-41.894943528921,-41.5454951067696),
 .UNSPECIFIED.);
#761=B_SPLINE_CURVE_WITH_KNOTS('',3,(#29474,#29475,#29476,#29477,#29478,
#29479,#29480,#29481,#29482,#29483,#29484,#29485,#29486,#29487,#29488,#29489,
#29490,#29491,#29492,#29493,#29494,#29495),.UNSPECIFIED.,.F.,.F.,(4,3,3,
3,3,3,3,4),(39.0089340982494,39.89994621802,40.8974448734705,41.894943528921,
42.8924421843715,43.889940839822,44.8874394952725,45.292119405429),
 .UNSPECIFIED.);
#762=B_SPLINE_CURVE_WITH_KNOTS('',3,(#29496,#29497,#29498,#29499,#29500,
#29501,#29502,#29503,#29504,#29505,#29506,#29507,#29508,#29509,#29510,#29511,
#29512,#29513,#29514,#29515,#29516,#29517),.UNSPECIFIED.,.F.,.F.,(4,3,3,
3,3,3,3,4),(-41.5454951067696,-40.8974448734705,-39.89994621802,-38.9024475625695,
-37.904948907119,-36.9074502516685,-35.909951596218,-35.26230979959),
 .UNSPECIFIED.);
#763=B_SPLINE_CURVE_WITH_KNOTS('',3,(#29522,#29523,#29524,#29525,#29526,
#29527,#29528,#29529,#29530,#29531,#29532,#29533,#29534,#29535,#29536,#29537,
#29538,#29539,#29540,#29541,#29542,#29543,#29544,#29545,#29546),
 .UNSPECIFIED.,.F.,.F.,(4,3,3,3,3,3,3,3,4),(32.7257487910698,32.9174556298665,
33.914954285317,34.9124529407675,35.909951596218,36.9074502516685,37.904948907119,
38.9024475625695,39.0089340982494),.UNSPECIFIED.);
#764=B_SPLINE_CURVE_WITH_KNOTS('',3,(#29547,#29548,#29549,#29550,#29551,
#29552,#29553,#29554,#29555,#29556,#29557,#29558,#29559,#29560,#29561,#29562,
#29563,#29564,#29565,#29566,#29567,#29568),.UNSPECIFIED.,.F.,.F.,(4,3,3,
3,3,3,3,4),(-35.26230979959,-34.9124529407675,-33.914954285317,-32.9174556298665,
-31.919956974416,-30.9224583189655,-29.924959663515,-28.9791244924104),
 .UNSPECIFIED.);
#765=B_SPLINE_CURVE_WITH_KNOTS('',3,(#29573,#29574,#29575,#29576,#29577,
#29578,#29579,#29580,#29581,#29582,#29583,#29584,#29585,#29586,#29587,#29588,
#29589,#29590,#29591,#29592,#29593,#29594),.UNSPECIFIED.,.F.,.F.,(4,3,3,
3,3,3,3,4),(26.4425634838902,26.9324636971635,27.929962352614,28.9274610080645,
29.924959663515,30.9224583189655,31.919956974416,32.7257487910698),
 .UNSPECIFIED.);
#766=B_SPLINE_CURVE_WITH_KNOTS('',3,(#29595,#29596,#29597,#29598,#29599,
#29600,#29601,#29602,#29603,#29604,#29605,#29606,#29607,#29608,#29609,#29610,
#29611,#29612,#29613,#29614,#29615,#29616,#29617,#29618,#29619),
 .UNSPECIFIED.,.F.,.F.,(4,3,3,3,3,3,3,3,4),(-28.9791244924104,-28.9274610080645,
-27.929962352614,-26.9324636971635,-25.934965041713,-24.9374663862625,-23.939967730812,
-22.9424690753615,-22.6959391852311),.UNSPECIFIED.);
#767=B_SPLINE_CURVE_WITH_KNOTS('',3,(#29624,#29625,#29626,#29627,#29628,
#29629,#29630,#29631,#29632,#29633,#29634,#29635,#29636,#29637,#29638,#29639,
#29640,#29641,#29642,#29643,#29644,#29645),.UNSPECIFIED.,.F.,.F.,(4,3,3,
3,3,3,3,4),(20.1593781767106,20.9474717644605,21.944970419911,22.9424690753615,
23.939967730812,24.9374663862625,25.934965041713,26.4425634838902),
 .UNSPECIFIED.);
#768=B_SPLINE_CURVE_WITH_KNOTS('',3,(#29646,#29647,#29648,#29649,#29650,
#29651,#29652,#29653,#29654,#29655,#29656,#29657,#29658,#29659,#29660,#29661,
#29662,#29663,#29664,#29665,#29666,#29667),.UNSPECIFIED.,.F.,.F.,(4,3,3,
3,3,3,3,4),(-22.6959391852311,-21.944970419911,-20.9474717644605,-19.94997310901,
-18.9524744535595,-17.954975798109,-16.9574771426585,-16.4127538780515),
 .UNSPECIFIED.);
#769=B_SPLINE_CURVE_WITH_KNOTS('',3,(#29672,#29673,#29674,#29675,#29676,
#29677,#29678,#29679,#29680,#29681,#29682,#29683,#29684,#29685,#29686,#29687,
#29688,#29689,#29690,#29691,#29692,#29693,#29694,#29695,#29696),
 .UNSPECIFIED.,.F.,.F.,(4,3,3,3,3,3,3,3,4),(13.8761928695309,13.964981176307,
14.9624798317575,15.959978487208,16.9574771426585,17.954975798109,18.9524744535595,
19.94997310901,20.1593781767106),.UNSPECIFIED.);
#770=B_SPLINE_CURVE_WITH_KNOTS('',3,(#29697,#29698,#29699,#29700,#29701,
#29702,#29703,#29704,#29705,#29706,#29707,#29708,#29709,#29710,#29711,#29712,
#29713,#29714,#29715,#29716,#29717,#29718),.UNSPECIFIED.,.F.,.F.,(4,3,3,
3,3,3,3,4),(-16.4127538780515,-15.959978487208,-14.9624798317575,-13.964981176307,
-12.9674825208565,-11.969983865406,-10.9724852099555,-10.1295685708719),
 .UNSPECIFIED.);
#771=B_SPLINE_CURVE_WITH_KNOTS('',3,(#29724,#29725,#29726,#29727,#29728,
#29729,#29730,#29731,#29732,#29733,#29734,#29735,#29736),.UNSPECIFIED.,
 .F.,.F.,(4,3,3,3,4),(-3.84638326369226,-2.9924959663515,-1.994997310901,
-0.9974986554505,0.),.UNSPECIFIED.);
#772=B_SPLINE_CURVE_WITH_KNOTS('',3,(#29739,#29740,#29741,#29742,#29743,
#29744,#29745,#29746,#29747,#29748,#29749,#29750,#29751,#29752,#29753,#29754,
#29755,#29756,#29757),.UNSPECIFIED.,.F.,.F.,(4,3,3,3,3,3,4),(2.01461286527449,
2.9924959663515,3.989994621802,4.9874932772525,5.984991932703,6.9824905881535,
7.59300756235133),.UNSPECIFIED.);
#773=B_SPLINE_CURVE_WITH_KNOTS('',3,(#29763,#29764,#29765,#29766,#29767),
 .UNSPECIFIED.,.F.,.F.,(4,1,4),(128.805298797181,129.566421347416,130.563920002866),
 .UNSPECIFIED.);
#774=B_SPLINE_CURVE_WITH_KNOTS('',3,(#29770,#29771,#29772,#29773,#29774,
#29775),.UNSPECIFIED.,.F.,.F.,(4,1,1,4),(128.805298797181,129.110486389585,
130.107985045035,131.085868146112),.UNSPECIFIED.);
#775=B_SPLINE_CURVE_WITH_KNOTS('',3,(#29780,#29781,#29782,#29783,#29784,
#29785,#29786,#29787,#29788,#29789,#29790),.UNSPECIFIED.,.F.,.F.,(4,1,1,
1,1,1,1,1,4),(122.522113490002,122.583930759262,123.581429414713,124.578928070163,
125.576426725614,126.573925381064,127.571424036515,128.568922691965,128.805298797181),
 .UNSPECIFIED.);
#776=B_SPLINE_CURVE_WITH_KNOTS('',3,(#29791,#29792,#29793,#29794,#29795,
#29796,#29797,#29798,#29799,#29800),.UNSPECIFIED.,.F.,.F.,(4,1,1,1,1,1,
1,4),(122.522113490002,123.125494456882,124.122993112332,125.120491767783,
126.117990423233,127.115489078684,128.112987734134,128.805298797181),
 .UNSPECIFIED.);
#777=B_SPLINE_CURVE_WITH_KNOTS('',3,(#29805,#29806,#29807,#29808,#29809,
#29810,#29811,#29812,#29813,#29814),.UNSPECIFIED.,.F.,.F.,(4,1,1,1,1,1,
1,4),(116.238928182823,116.598938826559,117.59643748201,118.59393613746,
119.591434792911,120.588933448361,121.586432103812,122.522113490002),
 .UNSPECIFIED.);
#778=B_SPLINE_CURVE_WITH_KNOTS('',3,(#29815,#29816,#29817,#29818,#29819,
#29820,#29821,#29822,#29823,#29824),.UNSPECIFIED.,.F.,.F.,(4,1,1,1,1,1,
1,4),(116.238928182822,117.140502524179,118.138001179629,119.13549983508,
120.13299849053,121.130497145981,122.127995801431,122.522113490002),
 .UNSPECIFIED.);
#779=B_SPLINE_CURVE_WITH_KNOTS('',3,(#29829,#29830,#29831,#29832,#29833,
#29834,#29835,#29836,#29837,#29838),.UNSPECIFIED.,.F.,.F.,(4,1,1,1,1,1,
1,4),(109.955742875643,110.613946893856,111.611445549307,112.608944204757,
113.606442860208,114.603941515658,115.601440171109,116.238928182823),
 .UNSPECIFIED.);
#780=B_SPLINE_CURVE_WITH_KNOTS('',3,(#29839,#29840,#29841,#29842,#29843,
#29844,#29845,#29846,#29847,#29848,#29849),.UNSPECIFIED.,.F.,.F.,(4,1,1,
1,1,1,1,1,4),(109.955742875643,110.158011936025,111.155510591476,112.153009246926,
113.150507902377,114.148006557827,115.145505213278,116.143003868728,116.238928182822),
 .UNSPECIFIED.);
#781=B_SPLINE_CURVE_WITH_KNOTS('',3,(#29854,#29855,#29856,#29857,#29858,
#29859,#29860,#29861,#29862,#29863),.UNSPECIFIED.,.F.,.F.,(4,1,1,1,1,1,
1,4),(103.672557568463,104.628954961153,105.626453616604,106.623952272054,
107.621450927505,108.618949582955,109.616448238406,109.955742875643),
 .UNSPECIFIED.);
#782=B_SPLINE_CURVE_WITH_KNOTS('',3,(#29864,#29865,#29866,#29867,#29868,
#29869,#29870,#29871,#29872,#29873),.UNSPECIFIED.,.F.,.F.,(4,1,1,1,1,1,
1,4),(103.672557568463,104.173020003322,105.170518658773,106.168017314223,
107.165515969674,108.163014625124,109.160513280575,109.955742875643),
 .UNSPECIFIED.);
#783=B_SPLINE_CURVE_WITH_KNOTS('',3,(#29878,#29879,#29880,#29881,#29882,
#29883,#29884,#29885,#29886,#29887,#29888),.UNSPECIFIED.,.F.,.F.,(4,1,1,
1,1,1,1,1,4),(97.3893722612837,97.6464643729997,98.6439630284502,99.6414616839007,
100.638960339351,101.636458994802,102.633957650252,103.631456305703,103.672557568463),
 .UNSPECIFIED.);
#784=B_SPLINE_CURVE_WITH_KNOTS('',3,(#29889,#29890,#29891,#29892,#29893,
#29894,#29895,#29896,#29897,#29898),.UNSPECIFIED.,.F.,.F.,(4,1,1,1,1,1,
1,4),(97.3893722612837,98.1880280706191,99.1855267260696,100.18302538152,
101.180524036971,102.178022692421,103.175521347872,103.672557568463),
 .UNSPECIFIED.);
#785=B_SPLINE_CURVE_WITH_KNOTS('',3,(#29903,#29904,#29905,#29906,#29907,
#29908,#29909,#29910,#29911,#29912),.UNSPECIFIED.,.F.,.F.,(4,1,1,1,1,1,
1,4),(91.106186954104,91.6614724402967,92.6589710957472,93.6564697511977,
94.6539684066482,95.6514670620987,96.6489657175492,97.3893722612837),
 .UNSPECIFIED.);
#786=B_SPLINE_CURVE_WITH_KNOTS('',3,(#29913,#29914,#29915,#29916,#29917,
#29918,#29919,#29920,#29921,#29922,#29923),.UNSPECIFIED.,.F.,.F.,(4,1,1,
1,1,1,1,1,4),(91.106186954104,91.2055374824655,92.203036137916,93.2005347933665,
94.198033448817,95.1955321042675,96.193030759718,97.1905294151685,97.3893722612837),
 .UNSPECIFIED.);
#787=B_SPLINE_CURVE_WITH_KNOTS('',3,(#29928,#29929,#29930,#29931,#29932,
#29933,#29934,#29935,#29936,#29937),.UNSPECIFIED.,.F.,.F.,(4,1,1,1,1,1,
1,4),(84.8230016469244,85.6764805075937,86.6739791630442,87.6714778184947,
88.6689764739452,89.6664751293957,90.6639737848462,91.106186954104),
 .UNSPECIFIED.);
#788=B_SPLINE_CURVE_WITH_KNOTS('',3,(#29938,#29939,#29940,#29941,#29942,
#29943,#29944,#29945,#29946,#29947),.UNSPECIFIED.,.F.,.F.,(4,1,1,1,1,1,
1,4),(84.8230016469245,85.2205455497625,86.218044205213,87.2155428606635,
88.213041516114,89.2105401715645,90.208038827015,91.106186954104),
 .UNSPECIFIED.);
#789=B_SPLINE_CURVE_WITH_KNOTS('',3,(#29952,#29953,#29954,#29955,#29956,
#29957,#29958,#29959,#29960,#29961,#29962),.UNSPECIFIED.,.F.,.F.,(4,1,1,
1,1,1,1,1,4),(78.5398163397449,78.6939899194402,79.6914885748907,80.6889872303412,
81.6864858857917,82.6839845412422,83.6814831966927,84.6789818521432,84.8230016469244),
 .UNSPECIFIED.);
#790=B_SPLINE_CURVE_WITH_KNOTS('',3,(#29963,#29964,#29965,#29966,#29967,
#29968,#29969,#29970,#29971,#29972),.UNSPECIFIED.,.F.,.F.,(4,1,1,1,1,1,
1,4),(78.5398163397448,79.2355536170595,80.23305227251,81.2305509279605,
82.228049583411,83.2255482388615,84.223046894312,84.8230016469245),
 .UNSPECIFIED.);
#791=B_SPLINE_CURVE_WITH_KNOTS('',3,(#29977,#29978,#29979,#29980,#29981,
#29982,#29983,#29984,#29985,#29986),.UNSPECIFIED.,.F.,.F.,(4,1,1,1,1,1,
1,4),(72.2566310325652,72.7089979867372,73.7064966421877,74.7039952976382,
75.7014939530887,76.6989926085392,77.6964912639897,78.5398163397449),
 .UNSPECIFIED.);
#792=B_SPLINE_CURVE_WITH_KNOTS('',3,(#29987,#29988,#29989,#29990,#29991,
#29992,#29993,#29994,#29995,#29996),.UNSPECIFIED.,.F.,.F.,(4,1,1,1,1,1,
1,4),(72.2566310325652,73.2505616843565,74.248060339807,75.2455589952575,
76.243057650708,77.2405563061585,78.238054961609,78.5398163397448),
 .UNSPECIFIED.);
#793=B_SPLINE_CURVE_WITH_KNOTS('',3,(#30001,#30002,#30003,#30004,#30005,
#30006,#30007,#30008,#30009,#30010),.UNSPECIFIED.,.F.,.F.,(4,1,1,1,1,1,
1,4),(65.9734457253856,66.7240060540342,67.7215047094847,68.7190033649352,
69.7165020203857,70.7140006758362,71.7114993312867,72.2566310325652),
 .UNSPECIFIED.);
#794=B_SPLINE_CURVE_WITH_KNOTS('',3,(#30011,#30012,#30013,#30014,#30015,
#30016,#30017,#30018,#30019,#30020,#30021),.UNSPECIFIED.,.F.,.F.,(4,1,1,
1,1,1,1,1,4),(65.9734457253856,66.268071096203,67.2655697516535,68.263068407104,
69.2605670625545,70.258065718005,71.2555643734555,72.253063028906,72.2566310325652),
 .UNSPECIFIED.);
#795=B_SPLINE_CURVE_WITH_KNOTS('',3,(#30026,#30027,#30028,#30029,#30030,
#30031,#30032,#30033,#30034,#30035,#30036),.UNSPECIFIED.,.F.,.F.,(4,1,1,
1,1,1,1,1,4),(59.690260418206,59.7415154658807,60.7390141213312,61.7365127767817,
62.7340114322322,63.7315100876827,64.7290087431332,65.7265073985837,65.9734457253856),
 .UNSPECIFIED.);
#796=B_SPLINE_CURVE_WITH_KNOTS('',3,(#30037,#30038,#30039,#30040,#30041,
#30042,#30043,#30044,#30045,#30046),.UNSPECIFIED.,.F.,.F.,(4,1,1,1,1,1,
1,4),(59.690260418206,60.2830791635,61.2805778189505,62.278076474401,63.2755751298515,
64.273073785302,65.2705724407525,65.9734457253856),.UNSPECIFIED.);
#797=B_SPLINE_CURVE_WITH_KNOTS('',3,(#30051,#30052,#30053,#30054,#30055,
#30056,#30057,#30058,#30059,#30060),.UNSPECIFIED.,.F.,.F.,(4,1,1,1,1,1,
1,4),(53.4070751110264,53.7565235331777,54.7540221886282,55.7515208440787,
56.7490194995292,57.7465181549797,58.7440168104302,59.690260418206),
 .UNSPECIFIED.);
#798=B_SPLINE_CURVE_WITH_KNOTS('',3,(#30061,#30062,#30063,#30064,#30065,
#30066,#30067,#30068,#30069,#30070),.UNSPECIFIED.,.F.,.F.,(4,1,1,1,1,1,
1,4),(53.4070751110264,54.298087230797,55.2955858862475,56.293084541698,
57.2905831971485,58.288081852599,59.2855805080495,59.690260418206),
 .UNSPECIFIED.);
#799=B_SPLINE_CURVE_WITH_KNOTS('',3,(#30075,#30076,#30077,#30078,#30079,
#30080,#30081,#30082,#30083,#30084),.UNSPECIFIED.,.F.,.F.,(4,1,1,1,1,1,
1,4),(47.1238898038468,47.7715316004747,48.7690302559252,49.7665289113757,
50.7640275668262,51.7615262222767,52.7590248777272,53.4070751110264),
 .UNSPECIFIED.);
#800=B_SPLINE_CURVE_WITH_KNOTS('',3,(#30085,#30086,#30087,#30088,#30089,
#30090,#30091,#30092,#30093,#30094,#30095),.UNSPECIFIED.,.F.,.F.,(4,1,1,
1,1,1,1,1,4),(47.1238898038468,47.3155966426435,48.313095298094,49.3105939535445,
50.308092608995,51.3055912644455,52.303089919896,53.3005885753465,53.4070751110264),
 .UNSPECIFIED.);
#801=B_SPLINE_CURVE_WITH_KNOTS('',3,(#30100,#30101,#30102,#30103,#30104,
#30105,#30106,#30107,#30108,#30109),.UNSPECIFIED.,.F.,.F.,(4,1,1,1,1,1,
1,4),(40.8407044966672,41.7865396677717,42.7840383232222,43.7815369786727,
44.7790356341232,45.7765342895737,46.7740329450242,47.1238898038468),
 .UNSPECIFIED.);
#802=B_SPLINE_CURVE_WITH_KNOTS('',3,(#30110,#30111,#30112,#30113,#30114,
#30115,#30116,#30117,#30118,#30119),.UNSPECIFIED.,.F.,.F.,(4,1,1,1,1,1,
1,4),(40.8407044966672,41.3306047099405,42.328103365391,43.3256020208415,
44.323100676292,45.3205993317425,46.318097987193,47.1238898038468),
 .UNSPECIFIED.);
#803=B_SPLINE_CURVE_WITH_KNOTS('',3,(#30124,#30125,#30126,#30127,#30128,
#30129,#30130,#30131,#30132,#30133,#30134),.UNSPECIFIED.,.F.,.F.,(4,1,1,
1,1,1,1,1,4),(34.5575191894876,34.8040490796182,35.8015477350687,36.7990463905192,
37.7965450459697,38.7940437014202,39.7915423568707,40.7890410123212,40.8407044966672),
 .UNSPECIFIED.);
#804=B_SPLINE_CURVE_WITH_KNOTS('',3,(#30135,#30136,#30137,#30138,#30139,
#30140,#30141,#30142,#30143,#30144),.UNSPECIFIED.,.F.,.F.,(4,1,1,1,1,1,
1,4),(34.5575191894876,35.3456127772375,36.343111432688,37.3406100881385,
38.338108743589,39.3356073990395,40.33310605449,40.8407044966672),
 .UNSPECIFIED.);
#805=B_SPLINE_CURVE_WITH_KNOTS('',3,(#30149,#30150,#30151,#30152,#30153,
#30154,#30155,#30156,#30157,#30158),.UNSPECIFIED.,.F.,.F.,(4,1,1,1,1,1,
1,4),(28.2743338823079,28.8190571469152,29.8165558023657,30.8140544578162,
31.8115531132667,32.8090517687172,33.8065504241677,34.5575191894876),
 .UNSPECIFIED.);
#806=B_SPLINE_CURVE_WITH_KNOTS('',3,(#30159,#30160,#30161,#30162,#30163,
#30164,#30165,#30166,#30167,#30168,#30169),.UNSPECIFIED.,.F.,.F.,(4,1,1,
1,1,1,1,1,4),(28.2743338823079,28.363122189084,29.3606208445345,30.358119499985,
31.3556181554355,32.353116810886,33.3506154663365,34.348114121787,34.5575191894876),
 .UNSPECIFIED.);
#807=B_SPLINE_CURVE_WITH_KNOTS('',3,(#30174,#30175,#30176,#30177,#30178,
#30179,#30180,#30181,#30182,#30183),.UNSPECIFIED.,.F.,.F.,(4,1,1,1,1,1,
1,4),(21.9911485751283,22.8340652142122,23.8315638696627,24.8290625251132,
25.8265611805637,26.8240598360142,27.8215584914647,28.2743338823079),
 .UNSPECIFIED.);
#808=B_SPLINE_CURVE_WITH_KNOTS('',3,(#30184,#30185,#30186,#30187,#30188,
#30189,#30190,#30191,#30192,#30193),.UNSPECIFIED.,.F.,.F.,(4,1,1,1,1,1,
1,4),(21.9911485751283,22.378130256381,23.3756289118315,24.373127567282,
25.3706262227325,26.368124878183,27.3656235336335,28.2743338823079),
 .UNSPECIFIED.);
#809=B_SPLINE_CURVE_WITH_KNOTS('',3,(#30199,#30200,#30201,#30202,#30203),
 .UNSPECIFIED.,.F.,.F.,(4,1,4),(14.398141012777,15.3956396682275,15.707963267949),
 .UNSPECIFIED.);
#810=B_SPLINE_CURVE_WITH_KNOTS('',3,(#30206,#30207,#30208,#30209,#30210),
 .UNSPECIFIED.,.F.,.F.,(4,1,4),(13.8761928695313,14.8540759706082,15.707963267949),
 .UNSPECIFIED.);
#811=B_SPLINE_CURVE_WITH_KNOTS('',3,(#30216,#30217,#30218,#30219,#30220,
#30221,#30222,#30223,#30224,#30225,#30226,#30227,#30228,#30229,#30230,#30231),
 .UNSPECIFIED.,.F.,.F.,(4,3,3,3,3,4),(114.407157784404,114.712345376807,
115.709844032258,116.707342687708,117.704841343159,118.702339998609),
 .UNSPECIFIED.);
#812=B_SPLINE_CURVE_WITH_KNOTS('',3,(#30239,#30240,#30241,#30242,#30243,
#30244,#30245,#30246,#30247,#30248,#30249,#30250,#30251,#30252,#30253,#30254,
#30255,#30256,#30257,#30258,#30259,#30260),.UNSPECIFIED.,.F.,.F.,(4,3,3,
3,3,3,3,4),(-116.687727133335,-115.709844032258,-114.712345376808,-113.714846721357,
-112.717348065907,-111.719849410456,-110.722350755006,-110.660533485745),
 .UNSPECIFIED.);
#813=B_SPLINE_CURVE_WITH_KNOTS('',3,(#30265,#30266,#30267,#30268,#30269,
#30270,#30271,#30272,#30273,#30274,#30275,#30276,#30277,#30278,#30279,#30280,
#30281,#30282,#30283,#30284,#30285,#30286),.UNSPECIFIED.,.F.,.F.,(4,3,3,
3,3,3,3,4),(108.123972477224,108.727353444104,109.724852099555,110.722350755005,
111.719849410456,112.717348065906,113.714846721357,114.407157784404),
 .UNSPECIFIED.);
#814=B_SPLINE_CURVE_WITH_KNOTS('',3,(#30287,#30288,#30289,#30290,#30291,
#30292,#30293,#30294,#30295,#30296,#30297,#30298,#30299,#30300,#30301,#30302,
#30303,#30304,#30305,#30306,#30307,#30308),.UNSPECIFIED.,.F.,.F.,(4,3,3,
3,3,3,3,4),(-110.660533485745,-109.724852099555,-108.727353444105,-107.729854788654,
-106.732356133204,-105.734857477753,-104.737358822303,-104.377348178565),
 .UNSPECIFIED.);
#815=B_SPLINE_CURVE_WITH_KNOTS('',3,(#30313,#30314,#30315,#30316,#30317,
#30318,#30319,#30320,#30321,#30322,#30323,#30324,#30325,#30326,#30327,#30328,
#30329,#30330,#30331,#30332,#30333,#30334),.UNSPECIFIED.,.F.,.F.,(4,3,3,
3,3,3,3,4),(101.840787170045,102.742361511401,103.739860166852,104.737358822302,
105.734857477753,106.732356133203,107.729854788654,108.123972477224),
 .UNSPECIFIED.);
#816=B_SPLINE_CURVE_WITH_KNOTS('',3,(#30335,#30336,#30337,#30338,#30339,
#30340,#30341,#30342,#30343,#30344,#30345,#30346,#30347,#30348,#30349,#30350,
#30351,#30352,#30353,#30354,#30355,#30356),.UNSPECIFIED.,.F.,.F.,(4,3,3,
3,3,3,3,4),(-104.377348178565,-103.739860166852,-102.742361511402,-101.744862855951,
-100.747364200501,-99.74986554505,-98.7523668895995,-98.0941628713855),
 .UNSPECIFIED.);
#817=B_SPLINE_CURVE_WITH_KNOTS('',3,(#30361,#30362,#30363,#30364,#30365,
#30366,#30367,#30368,#30369,#30370,#30371,#30372,#30373,#30374,#30375,#30376,
#30377,#30378,#30379,#30380,#30381,#30382,#30383,#30384,#30385),
 .UNSPECIFIED.,.F.,.F.,(4,3,3,3,3,3,3,3,4),(95.5576018628649,95.7598709232479,
96.7573695786984,97.7548682341489,98.7523668895994,99.7498655450499,100.7473642005,
101.744862855951,101.840787170045),.UNSPECIFIED.);
#818=B_SPLINE_CURVE_WITH_KNOTS('',3,(#30386,#30387,#30388,#30389,#30390,
#30391,#30392,#30393,#30394,#30395,#30396,#30397,#30398,#30399,#30400,#30401,
#30402,#30403,#30404,#30405,#30406,#30407),.UNSPECIFIED.,.F.,.F.,(4,3,3,
3,3,3,3,4),(-98.0941628713855,-97.754868234149,-96.7573695786985,-95.759870923248,
-94.7623722677975,-93.764873612347,-92.7673749568965,-91.8109775642059),
 .UNSPECIFIED.);
#819=B_SPLINE_CURVE_WITH_KNOTS('',3,(#30412,#30413,#30414,#30415,#30416,
#30417,#30418,#30419,#30420,#30421,#30422,#30423,#30424,#30425,#30426,#30427,
#30428,#30429,#30430,#30431,#30432,#30433),.UNSPECIFIED.,.F.,.F.,(4,3,3,
3,3,3,3,4),(89.2744165556853,89.774878990545,90.7723776459954,91.7698763014459,
92.7673749568964,93.7648736123469,94.7623722677974,95.5576018628649),
 .UNSPECIFIED.);
#820=B_SPLINE_CURVE_WITH_KNOTS('',3,(#30434,#30435,#30436,#30437,#30438,
#30439,#30440,#30441,#30442,#30443,#30444,#30445,#30446,#30447,#30448,#30449,
#30450,#30451,#30452,#30453,#30454,#30455,#30456,#30457,#30458),
 .UNSPECIFIED.,.F.,.F.,(4,3,3,3,3,3,3,3,4),(-91.8109775642059,-91.769876301446,
-90.7723776459955,-89.774878990545,-88.7773803350945,-87.779881679644,-86.7823830241935,
-85.784884368743,-85.5277922570263),.UNSPECIFIED.);
#821=B_SPLINE_CURVE_WITH_KNOTS('',3,(#30463,#30464,#30465,#30466,#30467,
#30468,#30469,#30470,#30471,#30472,#30473,#30474,#30475,#30476,#30477,#30478,
#30479,#30480,#30481,#30482,#30483,#30484),.UNSPECIFIED.,.F.,.F.,(4,3,3,
3,3,3,3,4),(82.9912312485057,83.789887057842,84.7873857132925,85.784884368743,
86.7823830241934,87.7798816796439,88.7773803350944,89.2744165556853),
 .UNSPECIFIED.);
#822=B_SPLINE_CURVE_WITH_KNOTS('',3,(#30485,#30486,#30487,#30488,#30489,
#30490,#30491,#30492,#30493,#30494,#30495,#30496,#30497,#30498,#30499,#30500,
#30501,#30502,#30503,#30504,#30505,#30506),.UNSPECIFIED.,.F.,.F.,(4,3,3,
3,3,3,3,4),(-85.5277922570263,-84.7873857132925,-83.789887057842,-82.7923884023915,
-81.794889746941,-80.7973910914905,-79.79989243604,-79.2446069498467),
 .UNSPECIFIED.);
#823=B_SPLINE_CURVE_WITH_KNOTS('',3,(#30511,#30512,#30513,#30514,#30515,
#30516,#30517,#30518,#30519,#30520,#30521,#30522,#30523,#30524,#30525,#30526,
#30527,#30528,#30529,#30530,#30531,#30532,#30533,#30534,#30535),
 .UNSPECIFIED.,.F.,.F.,(4,3,3,3,3,3,3,3,4),(76.7080459413261,76.8073964696885,
77.8048951251389,78.8023937805895,79.79989243604,80.7973910914905,81.7948897469409,
82.7923884023915,82.9912312485057),.UNSPECIFIED.);
#824=B_SPLINE_CURVE_WITH_KNOTS('',3,(#30536,#30537,#30538,#30539,#30540,
#30541,#30542,#30543,#30544,#30545,#30546,#30547,#30548,#30549,#30550,#30551,
#30552,#30553,#30554,#30555,#30556,#30557),.UNSPECIFIED.,.F.,.F.,(4,3,3,
3,3,3,3,4),(-79.2446069498467,-78.8023937805895,-77.804895125139,-76.8073964696885,
-75.809897814238,-74.8123991587875,-73.814900503337,-72.961421642667),
 .UNSPECIFIED.);
#825=B_SPLINE_CURVE_WITH_KNOTS('',3,(#30562,#30563,#30564,#30565,#30566,
#30567,#30568,#30569,#30570,#30571,#30572,#30573,#30574,#30575,#30576,#30577,
#30578,#30579,#30580,#30581,#30582,#30583),.UNSPECIFIED.,.F.,.F.,(4,3,3,
3,3,3,3,4),(70.4248606341465,70.8224045369854,71.8199031924359,72.8174018478865,
73.8149005033369,74.8123991587874,75.809897814238,76.7080459413261),
 .UNSPECIFIED.);
#826=B_SPLINE_CURVE_WITH_KNOTS('',3,(#30584,#30585,#30586,#30587,#30588,
#30589,#30590,#30591,#30592,#30593,#30594,#30595,#30596,#30597,#30598,#30599,
#30600,#30601,#30602,#30603,#30604,#30605,#30606,#30607,#30608),
 .UNSPECIFIED.,.F.,.F.,(4,3,3,3,3,3,3,3,4),(-72.961421642667,-72.8174018478865,
-71.819903192436,-70.8224045369855,-69.824905881535,-68.8274072260845,-67.829908570634,
-66.8324099151835,-66.6782363354874),.UNSPECIFIED.);
#827=B_SPLINE_CURVE_WITH_KNOTS('',3,(#30613,#30614,#30615,#30616,#30617,
#30618,#30619,#30620,#30621,#30622,#30623,#30624,#30625,#30626,#30627,#30628,
#30629,#30630,#30631,#30632,#30633,#30634),.UNSPECIFIED.,.F.,.F.,(4,3,3,
3,3,3,3,4),(64.1416753269669,64.8374126042824,65.8349112597329,66.8324099151835,
67.8299085706339,68.8274072260845,69.824905881535,70.4248606341465),
 .UNSPECIFIED.);
#828=B_SPLINE_CURVE_WITH_KNOTS('',3,(#30635,#30636,#30637,#30638,#30639,
#30640,#30641,#30642,#30643,#30644,#30645,#30646,#30647,#30648,#30649,#30650,
#30651,#30652,#30653,#30654,#30655,#30656),.UNSPECIFIED.,.F.,.F.,(4,3,3,
3,3,3,3,4),(-66.6782363354874,-65.834911259733,-64.8374126042825,-63.839913948832,
-62.8424152933815,-61.844916637931,-60.8474179824805,-60.3950510283078),
 .UNSPECIFIED.);
#829=B_SPLINE_CURVE_WITH_KNOTS('',3,(#30661,#30662,#30663,#30664,#30665,
#30666,#30667,#30668,#30669,#30670,#30671,#30672,#30673,#30674,#30675,#30676,
#30677,#30678,#30679,#30680,#30681,#30682),.UNSPECIFIED.,.F.,.F.,(4,3,3,
3,3,3,3,4),(57.8584900197873,58.8524206715795,59.84991932703,60.8474179824805,
61.844916637931,62.8424152933815,63.839913948832,64.1416753269669),
 .UNSPECIFIED.);
#830=B_SPLINE_CURVE_WITH_KNOTS('',3,(#30683,#30684,#30685,#30686,#30687,
#30688,#30689,#30690,#30691,#30692,#30693,#30694,#30695,#30696,#30697,#30698,
#30699,#30700,#30701,#30702,#30703,#30704),.UNSPECIFIED.,.F.,.F.,(4,3,3,
3,3,3,3,4),(-60.3950510283078,-59.84991932703,-58.8524206715795,-57.854922016129,
-56.8574233606785,-55.859924705228,-54.8624260497775,-54.1118657211282),
 .UNSPECIFIED.);
#831=B_SPLINE_CURVE_WITH_KNOTS('',3,(#30709,#30710,#30711,#30712,#30713,
#30714,#30715,#30716,#30717,#30718,#30719,#30720,#30721,#30722,#30723,#30724,
#30725,#30726,#30727,#30728,#30729,#30730,#30731,#30732,#30733),
 .UNSPECIFIED.,.F.,.F.,(4,3,3,3,3,3,3,3,4),(51.575304712608,51.869930083426,
52.8674287388765,53.8649273943269,54.8624260497775,55.859924705228,56.8574233606785,
57.854922016129,57.8584900197873),.UNSPECIFIED.);
#832=B_SPLINE_CURVE_WITH_KNOTS('',3,(#30734,#30735,#30736,#30737,#30738,
#30739,#30740,#30741,#30742,#30743,#30744,#30745,#30746,#30747,#30748,#30749,
#30750,#30751,#30752,#30753,#30754,#30755,#30756,#30757,#30758),
 .UNSPECIFIED.,.F.,.F.,(4,3,3,3,3,3,3,3,4),(-54.1118657211282,-53.864927394327,
-52.8674287388765,-51.869930083426,-50.8724314279755,-49.874932772525,-48.8774341170745,
-47.879935461624,-47.8286804139486),.UNSPECIFIED.);
#833=B_SPLINE_CURVE_WITH_KNOTS('',3,(#30763,#30764,#30765,#30766,#30767,
#30768,#30769,#30770,#30771,#30772,#30773,#30774,#30775,#30776,#30777,#30778,
#30779,#30780,#30781,#30782,#30783,#30784),.UNSPECIFIED.,.F.,.F.,(4,3,3,
3,3,3,3,4),(45.2921194054284,45.884938150723,46.8824368061735,47.879935461624,
48.8774341170745,49.874932772525,50.8724314279755,51.575304712608),
 .UNSPECIFIED.);
#834=B_SPLINE_CURVE_WITH_KNOTS('',3,(#30785,#30786,#30787,#30788,#30789,
#30790,#30791,#30792,#30793,#30794,#30795,#30796,#30797,#30798,#30799,#30800,
#30801,#30802,#30803,#30804,#30805,#30806),.UNSPECIFIED.,.F.,.F.,(4,3,3,
3,3,3,3,4),(-47.8286804139486,-46.8824368061735,-45.884938150723,-44.8874394952725,
-43.889940839822,-42.8924421843715,-41.894943528921,-41.545495106769),
 .UNSPECIFIED.);
#835=B_SPLINE_CURVE_WITH_KNOTS('',3,(#30811,#30812,#30813,#30814,#30815,
#30816,#30817,#30818,#30819,#30820,#30821,#30822,#30823,#30824,#30825,#30826,
#30827,#30828,#30829,#30830,#30831,#30832),.UNSPECIFIED.,.F.,.F.,(4,3,3,
3,3,3,3,4),(39.0089340982488,39.89994621802,40.8974448734705,41.894943528921,
42.8924421843715,43.889940839822,44.8874394952725,45.2921194054284),
 .UNSPECIFIED.);
#836=B_SPLINE_CURVE_WITH_KNOTS('',3,(#30833,#30834,#30835,#30836,#30837,
#30838,#30839,#30840,#30841,#30842,#30843,#30844,#30845,#30846,#30847,#30848,
#30849,#30850,#30851,#30852,#30853,#30854),.UNSPECIFIED.,.F.,.F.,(4,3,3,
3,3,3,3,4),(-41.545495106769,-40.8974448734705,-39.89994621802,-38.9024475625695,
-37.904948907119,-36.9074502516685,-35.909951596218,-35.2623097995894),
 .UNSPECIFIED.);
#837=B_SPLINE_CURVE_WITH_KNOTS('',3,(#30859,#30860,#30861,#30862,#30863,
#30864,#30865,#30866,#30867,#30868,#30869,#30870,#30871,#30872,#30873,#30874,
#30875,#30876,#30877,#30878,#30879,#30880,#30881,#30882,#30883),
 .UNSPECIFIED.,.F.,.F.,(4,3,3,3,3,3,3,3,4),(32.7257487910691,32.9174556298665,
33.914954285317,34.9124529407675,35.909951596218,36.9074502516685,37.904948907119,
38.9024475625695,39.0089340982488),.UNSPECIFIED.);
#838=B_SPLINE_CURVE_WITH_KNOTS('',3,(#30884,#30885,#30886,#30887,#30888,
#30889,#30890,#30891,#30892,#30893,#30894,#30895,#30896,#30897,#30898,#30899,
#30900,#30901,#30902,#30903,#30904,#30905),.UNSPECIFIED.,.F.,.F.,(4,3,3,
3,3,3,3,4),(-35.2623097995894,-34.9124529407675,-33.914954285317,-32.9174556298665,
-31.919956974416,-30.9224583189655,-29.924959663515,-28.9791244924098),
 .UNSPECIFIED.);
#839=B_SPLINE_CURVE_WITH_KNOTS('',3,(#30910,#30911,#30912,#30913,#30914,
#30915,#30916,#30917,#30918,#30919,#30920,#30921,#30922,#30923,#30924,#30925,
#30926,#30927,#30928,#30929,#30930,#30931),.UNSPECIFIED.,.F.,.F.,(4,3,3,
3,3,3,3,4),(26.4425634838895,26.9324636971635,27.929962352614,28.9274610080645,
29.924959663515,30.9224583189655,31.919956974416,32.7257487910691),
 .UNSPECIFIED.);
#840=B_SPLINE_CURVE_WITH_KNOTS('',3,(#30932,#30933,#30934,#30935,#30936,
#30937,#30938,#30939,#30940,#30941,#30942,#30943,#30944,#30945,#30946,#30947,
#30948,#30949,#30950,#30951,#30952,#30953,#30954,#30955,#30956),
 .UNSPECIFIED.,.F.,.F.,(4,3,3,3,3,3,3,3,4),(-28.9791244924098,-28.9274610080645,
-27.929962352614,-26.9324636971635,-25.934965041713,-24.9374663862625,-23.939967730812,
-22.9424690753615,-22.6959391852305),.UNSPECIFIED.);
#841=B_SPLINE_CURVE_WITH_KNOTS('',3,(#30961,#30962,#30963,#30964,#30965,
#30966,#30967,#30968,#30969,#30970,#30971,#30972,#30973,#30974,#30975,#30976,
#30977,#30978,#30979,#30980,#30981,#30982),.UNSPECIFIED.,.F.,.F.,(4,3,3,
3,3,3,3,4),(20.1593781767099,20.9474717644605,21.944970419911,22.9424690753615,
23.939967730812,24.9374663862625,25.934965041713,26.4425634838895),
 .UNSPECIFIED.);
#842=B_SPLINE_CURVE_WITH_KNOTS('',3,(#30983,#30984,#30985,#30986,#30987,
#30988,#30989,#30990,#30991,#30992,#30993,#30994,#30995,#30996,#30997,#30998,
#30999,#31000,#31001,#31002,#31003,#31004),.UNSPECIFIED.,.F.,.F.,(4,3,3,
3,3,3,3,4),(-22.6959391852305,-21.944970419911,-20.9474717644605,-19.94997310901,
-18.9524744535595,-17.954975798109,-16.9574771426585,-16.4127538780508),
 .UNSPECIFIED.);
#843=B_SPLINE_CURVE_WITH_KNOTS('',3,(#31009,#31010,#31011,#31012,#31013,
#31014,#31015,#31016,#31017,#31018,#31019,#31020,#31021,#31022,#31023,#31024,
#31025,#31026,#31027,#31028,#31029,#31030,#31031,#31032,#31033),
 .UNSPECIFIED.,.F.,.F.,(4,3,3,3,3,3,3,3,4),(13.8761928695303,13.964981176307,
14.9624798317575,15.959978487208,16.9574771426585,17.954975798109,18.9524744535595,
19.94997310901,20.1593781767099),.UNSPECIFIED.);
#844=B_SPLINE_CURVE_WITH_KNOTS('',3,(#31034,#31035,#31036,#31037,#31038,
#31039,#31040,#31041,#31042,#31043,#31044,#31045,#31046,#31047,#31048,#31049,
#31050,#31051,#31052,#31053,#31054,#31055),.UNSPECIFIED.,.F.,.F.,(4,3,3,
3,3,3,3,4),(-16.4127538780508,-15.959978487208,-14.9624798317575,-13.964981176307,
-12.9674825208565,-11.969983865406,-10.9724852099555,-10.1295685708712),
 .UNSPECIFIED.);
#845=B_SPLINE_CURVE_WITH_KNOTS('',3,(#31061,#31062,#31063,#31064,#31065,
#31066,#31067,#31068,#31069,#31070,#31071,#31072,#31073),.UNSPECIFIED.,
 .F.,.F.,(4,3,3,3,4),(-3.84638326369162,-2.9924959663515,-1.994997310901,
-0.9974986554505,0.),.UNSPECIFIED.);
#846=B_SPLINE_CURVE_WITH_KNOTS('',3,(#31076,#31077,#31078,#31079,#31080,
#31081,#31082,#31083,#31084,#31085,#31086,#31087,#31088,#31089,#31090,#31091,
#31092,#31093,#31094),.UNSPECIFIED.,.F.,.F.,(4,3,3,3,3,3,4),(2.01461286527449,
2.9924959663515,3.989994621802,4.9874932772525,5.984991932703,6.9824905881535,
7.59300756235069),.UNSPECIFIED.);
#847=B_SPLINE_CURVE_WITH_KNOTS('',3,(#31100,#31101,#31102,#31103,#31104),
 .UNSPECIFIED.,.F.,.F.,(4,1,4),(128.805298797181,129.566421347416,130.563920002867),
 .UNSPECIFIED.);
#848=B_SPLINE_CURVE_WITH_KNOTS('',3,(#31107,#31108,#31109,#31110,#31111,
#31112),.UNSPECIFIED.,.F.,.F.,(4,1,1,4),(128.805298797181,129.110486389585,
130.107985045036,131.085868146113),.UNSPECIFIED.);
#849=B_SPLINE_CURVE_WITH_KNOTS('',3,(#31117,#31118,#31119,#31120,#31121,
#31122,#31123,#31124,#31125,#31126,#31127),.UNSPECIFIED.,.F.,.F.,(4,1,1,
1,1,1,1,1,4),(122.522113490002,122.583930759263,123.581429414713,124.578928070164,
125.576426725614,126.573925381065,127.571424036515,128.568922691966,128.805298797181),
 .UNSPECIFIED.);
#850=B_SPLINE_CURVE_WITH_KNOTS('',3,(#31128,#31129,#31130,#31131,#31132,
#31133,#31134,#31135,#31136,#31137),.UNSPECIFIED.,.F.,.F.,(4,1,1,1,1,1,
1,4),(122.522113490002,123.125494456882,124.122993112333,125.120491767783,
126.117990423234,127.115489078684,128.112987734135,128.805298797181),
 .UNSPECIFIED.);
#851=B_SPLINE_CURVE_WITH_KNOTS('',3,(#31142,#31143,#31144,#31145,#31146,
#31147,#31148,#31149,#31150,#31151),.UNSPECIFIED.,.F.,.F.,(4,1,1,1,1,1,
1,4),(116.238928182822,116.59893882656,117.59643748201,118.593936137461,
119.591434792911,120.588933448362,121.586432103812,122.522113490002),
 .UNSPECIFIED.);
#852=B_SPLINE_CURVE_WITH_KNOTS('',3,(#31152,#31153,#31154,#31155,#31156,
#31157,#31158,#31159,#31160,#31161),.UNSPECIFIED.,.F.,.F.,(4,1,1,1,1,1,
1,4),(116.238928182822,117.140502524179,118.13800117963,119.13549983508,
120.132998490531,121.130497145981,122.127995801432,122.522113490002),
 .UNSPECIFIED.);
#853=B_SPLINE_CURVE_WITH_KNOTS('',3,(#31166,#31167,#31168,#31169,#31170,
#31171,#31172,#31173,#31174,#31175),.UNSPECIFIED.,.F.,.F.,(4,1,1,1,1,1,
1,4),(109.955742875643,110.613946893857,111.611445549307,112.608944204758,
113.606442860208,114.603941515659,115.601440171109,116.238928182822),
 .UNSPECIFIED.);
#854=B_SPLINE_CURVE_WITH_KNOTS('',3,(#31176,#31177,#31178,#31179,#31180,
#31181,#31182,#31183,#31184,#31185,#31186),.UNSPECIFIED.,.F.,.F.,(4,1,1,
1,1,1,1,1,4),(109.955742875643,110.158011936026,111.155510591476,112.153009246927,
113.150507902377,114.148006557828,115.145505213278,116.143003868729,116.238928182822),
 .UNSPECIFIED.);
#855=B_SPLINE_CURVE_WITH_KNOTS('',3,(#31191,#31192,#31193,#31194,#31195,
#31196,#31197,#31198,#31199,#31200),.UNSPECIFIED.,.F.,.F.,(4,1,1,1,1,1,
1,4),(103.672557568463,104.628954961154,105.626453616604,106.623952272055,
107.621450927505,108.618949582956,109.616448238406,109.955742875643),
 .UNSPECIFIED.);
#856=B_SPLINE_CURVE_WITH_KNOTS('',3,(#31201,#31202,#31203,#31204,#31205,
#31206,#31207,#31208,#31209,#31210),.UNSPECIFIED.,.F.,.F.,(4,1,1,1,1,1,
1,4),(103.672557568463,104.173020003323,105.170518658773,106.168017314224,
107.165515969674,108.163014625125,109.160513280575,109.955742875643),
 .UNSPECIFIED.);
#857=B_SPLINE_CURVE_WITH_KNOTS('',3,(#31215,#31216,#31217,#31218,#31219,
#31220,#31221,#31222,#31223,#31224,#31225),.UNSPECIFIED.,.F.,.F.,(4,1,1,
1,1,1,1,1,4),(97.3893722612837,97.6464643730003,98.6439630284508,99.6414616839013,
100.638960339352,101.636458994802,102.633957650253,103.631456305703,103.672557568463),
 .UNSPECIFIED.);
#858=B_SPLINE_CURVE_WITH_KNOTS('',3,(#31226,#31227,#31228,#31229,#31230,
#31231,#31232,#31233,#31234,#31235),.UNSPECIFIED.,.F.,.F.,(4,1,1,1,1,1,
1,4),(97.3893722612837,98.1880280706196,99.1855267260701,100.183025381521,
101.180524036971,102.178022692422,103.175521347872,103.672557568463),
 .UNSPECIFIED.);
#859=B_SPLINE_CURVE_WITH_KNOTS('',3,(#31240,#31241,#31242,#31243,#31244,
#31245,#31246,#31247,#31248,#31249),.UNSPECIFIED.,.F.,.F.,(4,1,1,1,1,1,
1,4),(91.106186954104,91.6614724402973,92.6589710957478,93.6564697511983,
94.6539684066488,95.6514670620993,96.6489657175498,97.3893722612837),
 .UNSPECIFIED.);
#860=B_SPLINE_CURVE_WITH_KNOTS('',3,(#31250,#31251,#31252,#31253,#31254,
#31255,#31256,#31257,#31258,#31259,#31260),.UNSPECIFIED.,.F.,.F.,(4,1,1,
1,1,1,1,1,4),(91.106186954104,91.2055374824661,92.2030361379166,93.2005347933671,
94.1980334488176,95.1955321042681,96.1930307597186,97.1905294151691,97.3893722612837),
 .UNSPECIFIED.);
#861=B_SPLINE_CURVE_WITH_KNOTS('',3,(#31265,#31266,#31267,#31268,#31269,
#31270,#31271,#31272,#31273,#31274),.UNSPECIFIED.,.F.,.F.,(4,1,1,1,1,1,
1,4),(84.8230016469245,85.6764805075943,86.6739791630448,87.6714778184953,
88.6689764739458,89.6664751293963,90.6639737848468,91.106186954104),
 .UNSPECIFIED.);
#862=B_SPLINE_CURVE_WITH_KNOTS('',3,(#31275,#31276,#31277,#31278,#31279,
#31280,#31281,#31282,#31283,#31284),.UNSPECIFIED.,.F.,.F.,(4,1,1,1,1,1,
1,4),(84.8230016469245,85.2205455497631,86.2180442052136,87.2155428606641,
88.2130415161146,89.2105401715651,90.2080388270156,91.106186954104),
 .UNSPECIFIED.);
#863=B_SPLINE_CURVE_WITH_KNOTS('',3,(#31289,#31290,#31291,#31292,#31293,
#31294,#31295,#31296,#31297,#31298,#31299),.UNSPECIFIED.,.F.,.F.,(4,1,1,
1,1,1,1,1,4),(78.5398163397448,78.6939899194408,79.6914885748913,80.6889872303418,
81.6864858857923,82.6839845412428,83.6814831966933,84.6789818521438,84.8230016469245),
 .UNSPECIFIED.);
#864=B_SPLINE_CURVE_WITH_KNOTS('',3,(#31300,#31301,#31302,#31303,#31304,
#31305,#31306,#31307,#31308,#31309),.UNSPECIFIED.,.F.,.F.,(4,1,1,1,1,1,
1,4),(78.5398163397448,79.2355536170601,80.2330522725106,81.2305509279611,
82.2280495834116,83.2255482388621,84.2230468943126,84.8230016469245),
 .UNSPECIFIED.);
#865=B_SPLINE_CURVE_WITH_KNOTS('',3,(#31314,#31315,#31316,#31317,#31318,
#31319,#31320,#31321,#31322,#31323),.UNSPECIFIED.,.F.,.F.,(4,1,1,1,1,1,
1,4),(72.2566310325652,72.7089979867378,73.7064966421883,74.7039952976388,
75.7014939530893,76.6989926085398,77.6964912639903,78.5398163397448),
 .UNSPECIFIED.);
#866=B_SPLINE_CURVE_WITH_KNOTS('',3,(#31324,#31325,#31326,#31327,#31328,
#31329,#31330,#31331,#31332,#31333),.UNSPECIFIED.,.F.,.F.,(4,1,1,1,1,1,
1,4),(72.2566310325652,73.2505616843571,74.2480603398076,75.2455589952581,
76.2430576507086,77.2405563061591,78.2380549616096,78.5398163397448),
 .UNSPECIFIED.);
#867=B_SPLINE_CURVE_WITH_KNOTS('',3,(#31338,#31339,#31340,#31341,#31342,
#31343,#31344,#31345,#31346,#31347),.UNSPECIFIED.,.F.,.F.,(4,1,1,1,1,1,
1,4),(65.9734457253856,66.7240060540348,67.7215047094853,68.7190033649358,
69.7165020203863,70.7140006758368,71.7114993312873,72.2566310325652),
 .UNSPECIFIED.);
#868=B_SPLINE_CURVE_WITH_KNOTS('',3,(#31348,#31349,#31350,#31351,#31352,
#31353,#31354,#31355,#31356,#31357,#31358),.UNSPECIFIED.,.F.,.F.,(4,1,1,
1,1,1,1,1,4),(65.9734457253856,66.2680710962036,67.2655697516541,68.2630684071046,
69.2605670625551,70.2580657180056,71.2555643734561,72.2530630289066,72.2566310325652),
 .UNSPECIFIED.);
#869=B_SPLINE_CURVE_WITH_KNOTS('',3,(#31363,#31364,#31365,#31366,#31367,
#31368,#31369,#31370,#31371,#31372,#31373),.UNSPECIFIED.,.F.,.F.,(4,1,1,
1,1,1,1,1,4),(59.690260418206,59.7415154658813,60.7390141213318,61.7365127767823,
62.7340114322328,63.7315100876833,64.7290087431338,65.7265073985843,65.9734457253856),
 .UNSPECIFIED.);
#870=B_SPLINE_CURVE_WITH_KNOTS('',3,(#31374,#31375,#31376,#31377,#31378,
#31379,#31380,#31381,#31382,#31383),.UNSPECIFIED.,.F.,.F.,(4,1,1,1,1,1,
1,4),(59.690260418206,60.2830791635006,61.2805778189511,62.2780764744016,
63.2755751298521,64.2730737853026,65.2705724407531,65.9734457253856),
 .UNSPECIFIED.);
#871=B_SPLINE_CURVE_WITH_KNOTS('',3,(#31388,#31389,#31390,#31391,#31392,
#31393,#31394,#31395,#31396,#31397),.UNSPECIFIED.,.F.,.F.,(4,1,1,1,1,1,
1,4),(53.4070751110264,53.7565235331783,54.7540221886288,55.7515208440793,
56.7490194995298,57.7465181549803,58.7440168104308,59.690260418206),
 .UNSPECIFIED.);
#872=B_SPLINE_CURVE_WITH_KNOTS('',3,(#31398,#31399,#31400,#31401,#31402,
#31403,#31404,#31405,#31406,#31407),.UNSPECIFIED.,.F.,.F.,(4,1,1,1,1,1,
1,4),(53.4070751110264,54.2980872307976,55.2955858862481,56.2930845416986,
57.2905831971491,58.2880818525996,59.2855805080501,59.690260418206),
 .UNSPECIFIED.);
#873=B_SPLINE_CURVE_WITH_KNOTS('',3,(#31412,#31413,#31414,#31415,#31416,
#31417,#31418,#31419,#31420,#31421),.UNSPECIFIED.,.F.,.F.,(4,1,1,1,1,1,
1,4),(47.1238898038468,47.7715316004753,48.7690302559258,49.7665289113763,
50.7640275668268,51.7615262222773,52.7590248777278,53.4070751110264),
 .UNSPECIFIED.);
#874=B_SPLINE_CURVE_WITH_KNOTS('',3,(#31422,#31423,#31424,#31425,#31426,
#31427,#31428,#31429,#31430,#31431,#31432),.UNSPECIFIED.,.F.,.F.,(4,1,1,
1,1,1,1,1,4),(47.1238898038468,47.3155966426441,48.3130952980946,49.3105939535451,
50.3080926089956,51.3055912644461,52.3030899198966,53.3005885753471,53.4070751110264),
 .UNSPECIFIED.);
#875=B_SPLINE_CURVE_WITH_KNOTS('',3,(#31437,#31438,#31439,#31440,#31441,
#31442,#31443,#31444,#31445,#31446),.UNSPECIFIED.,.F.,.F.,(4,1,1,1,1,1,
1,4),(40.8407044966672,41.7865396677723,42.7840383232228,43.7815369786733,
44.7790356341238,45.7765342895743,46.7740329450248,47.1238898038468),
 .UNSPECIFIED.);
#876=B_SPLINE_CURVE_WITH_KNOTS('',3,(#31447,#31448,#31449,#31450,#31451,
#31452,#31453,#31454,#31455,#31456),.UNSPECIFIED.,.F.,.F.,(4,1,1,1,1,1,
1,4),(40.8407044966672,41.3306047099411,42.3281033653916,43.3256020208421,
44.3231006762926,45.3205993317431,46.3180979871936,47.1238898038468),
 .UNSPECIFIED.);
#877=B_SPLINE_CURVE_WITH_KNOTS('',3,(#31461,#31462,#31463,#31464,#31465,
#31466,#31467,#31468,#31469,#31470,#31471),.UNSPECIFIED.,.F.,.F.,(4,1,1,
1,1,1,1,1,4),(34.5575191894876,34.8040490796188,35.8015477350693,36.7990463905198,
37.7965450459703,38.7940437014208,39.7915423568713,40.7890410123218,40.8407044966672),
 .UNSPECIFIED.);
#878=B_SPLINE_CURVE_WITH_KNOTS('',3,(#31472,#31473,#31474,#31475,#31476,
#31477,#31478,#31479,#31480,#31481),.UNSPECIFIED.,.F.,.F.,(4,1,1,1,1,1,
1,4),(34.5575191894876,35.3456127772381,36.3431114326886,37.3406100881391,
38.3381087435896,39.3356073990401,40.3331060544906,40.8407044966672),
 .UNSPECIFIED.);
#879=B_SPLINE_CURVE_WITH_KNOTS('',3,(#31486,#31487,#31488,#31489,#31490,
#31491,#31492,#31493,#31494,#31495),.UNSPECIFIED.,.F.,.F.,(4,1,1,1,1,1,
1,4),(28.2743338823079,28.8190571469158,29.8165558023663,30.8140544578168,
31.8115531132673,32.8090517687178,33.8065504241683,34.5575191894876),
 .UNSPECIFIED.);
#880=B_SPLINE_CURVE_WITH_KNOTS('',3,(#31496,#31497,#31498,#31499,#31500,
#31501,#31502,#31503,#31504,#31505,#31506),.UNSPECIFIED.,.F.,.F.,(4,1,1,
1,1,1,1,1,4),(28.2743338823079,28.3631221890846,29.3606208445351,30.3581194999856,
31.3556181554361,32.3531168108866,33.3506154663371,34.3481141217876,34.5575191894876),
 .UNSPECIFIED.);
#881=B_SPLINE_CURVE_WITH_KNOTS('',3,(#31511,#31512,#31513,#31514,#31515,
#31516,#31517,#31518,#31519,#31520),.UNSPECIFIED.,.F.,.F.,(4,1,1,1,1,1,
1,4),(21.9911485751283,22.8340652142128,23.8315638696633,24.8290625251138,
25.8265611805643,26.8240598360148,27.8215584914653,28.2743338823079),
 .UNSPECIFIED.);
#882=B_SPLINE_CURVE_WITH_KNOTS('',3,(#31521,#31522,#31523,#31524,#31525,
#31526,#31527,#31528,#31529,#31530),.UNSPECIFIED.,.F.,.F.,(4,1,1,1,1,1,
1,4),(21.9911485751283,22.3781302563816,23.3756289118321,24.3731275672826,
25.3706262227331,26.3681248781836,27.3656235336341,28.2743338823079),
 .UNSPECIFIED.);
#883=B_SPLINE_CURVE_WITH_KNOTS('',3,(#31536,#31537,#31538,#31539,#31540),
 .UNSPECIFIED.,.F.,.F.,(4,1,4),(14.3981410127776,15.3956396682281,15.707963267949),
 .UNSPECIFIED.);
#884=B_SPLINE_CURVE_WITH_KNOTS('',3,(#31543,#31544,#31545,#31546,#31547),
 .UNSPECIFIED.,.F.,.F.,(4,1,4),(13.8761928695319,14.8540759706088,15.7079632679487),
 .UNSPECIFIED.);
#885=B_SPLINE_CURVE_WITH_KNOTS('',3,(#31549,#31550,#31551,#31552,#31553,
#31554,#31555,#31556,#31557,#31558,#31559,#31560,#31561,#31562,#31563,#31564,
#31565,#31566,#31567,#31568,#31569,#31570,#31571,#31572,#31573,#31574,#31575,
#31576,#31577,#31578,#31579,#31580,#31581,#31582,#31583,#31584,#31585,#31586,
#31587,#31588,#31589,#31590,#31591,#31592,#31593,#31594,#31595,#31596,#31597,
#31598,#31599,#31600,#31601,#31602,#31603,#31604,#31605,#31606,#31607,#31608,
#31609,#31610,#31611,#31612,#31613,#31614,#31615,#31616,#31617,#31618,#31619,
#31620,#31621,#31622,#31623,#31624,#31625,#31626,#31627,#31628,#31629,#31630,
#31631,#31632,#31633,#31634,#31635,#31636),.UNSPECIFIED.,.F.,.F.,(4,3,3,
3,3,3,3,3,3,3,3,3,3,3,3,3,3,3,3,3,3,3,3,3,3,3,3,3,3,4),(-0.378621596831491,
-0.359799974259491,-0.347867720488378,-0.339795904888389,-0.335415766246889,
-0.315546491055276,-0.301208576176833,-0.297330142863398,-0.293235364838415,
-0.272834900814394,-0.252137033433983,-0.23931356808242,-0.228820743229234,
-0.224509894764592,-0.203205274087435,-0.200843172027728,-0.180354289318363,
-0.158315828378964,-0.154363755179046,-0.150814789240723,-0.129430304994364,
-0.107595617692396,-0.0856289754902388,-0.080208065969872,-0.0759455790412052,
-0.0533977706849842,-0.0308256528945546,-0.00876661790841547,-0.00404660180317386,
0.),.UNSPECIFIED.);
#886=B_SPLINE_CURVE_WITH_KNOTS('',3,(#31637,#31638,#31639,#31640,#31641,
#31642,#31643,#31644,#31645,#31646,#31647,#31648,#31649,#31650,#31651,#31652,
#31653,#31654,#31655,#31656,#31657,#31658,#31659,#31660,#31661,#31662,#31663,
#31664,#31665,#31666,#31667,#31668,#31669,#31670,#31671,#31672,#31673,#31674,
#31675,#31676,#31677,#31678,#31679,#31680,#31681,#31682,#31683,#31684,#31685,
#31686,#31687,#31688,#31689,#31690,#31691,#31692,#31693,#31694,#31695,#31696,
#31697,#31698,#31699,#31700,#31701,#31702,#31703,#31704,#31705,#31706,#31707,
#31708,#31709,#31710,#31711,#31712,#31713,#31714,#31715,#31716,#31717,#31718,
#31719,#31720,#31721),.UNSPECIFIED.,.F.,.F.,(4,3,3,3,3,3,3,3,3,3,3,3,3,
3,3,3,3,3,3,3,3,3,3,3,3,3,3,3,4),(-0.37694081721165,-0.35463588075101,-0.332914954557582,
-0.328066888666082,-0.305818294401826,-0.290199566502046,-0.284267361548342,
-0.278599939690394,-0.256916538505875,-0.235698318877041,-0.214945663233777,
-0.208192982084683,-0.204402876940358,-0.183826063192256,-0.180868471203588,
-0.159885877939655,-0.140312002594425,-0.136050822944271,-0.13260723132917,
-0.112148152518366,-0.0917831465515227,-0.0718536005353655,-0.0676631141183089,
-0.0636717608241292,-0.0441132632842336,-0.02492609063918,-0.0063612278911709,
-0.00329487517781129,0.),.UNSPECIFIED.);
#887=B_SPLINE_CURVE_WITH_KNOTS('',3,(#31723,#31724,#31725,#31726,#31727,
#31728,#31729,#31730,#31731,#31732,#31733),.UNSPECIFIED.,.F.,.F.,(4,1,1,
1,1,1,1,1,4),(15.7079632679487,15.8515746260593,16.8490732815098,17.8465719369603,
18.8440705924108,19.8415692478613,20.8390679033118,21.8365665587623,21.9911485751283),
 .UNSPECIFIED.);
#888=B_SPLINE_CURVE_WITH_KNOTS('',3,(#31734,#31735,#31736,#31737,#31738,
#31739,#31740,#31741,#31742,#31743),.UNSPECIFIED.,.F.,.F.,(4,1,1,1,1,1,
1,4),(15.707963267949,16.3931383236786,17.3906369791291,18.3881356345796,
19.3856342900301,20.3831329454806,21.3806316009311,21.9911485751283),
 .UNSPECIFIED.);
#889=B_SPLINE_CURVE_WITH_KNOTS('',3,(#32232,#32233,#32234,#32235,#32236,
#32237,#32238,#32239,#32240,#32241,#32242,#32243,#32244,#32245,#32246,#32247,
#32248,#32249,#32250,#32251,#32252,#32253,#32254,#32255,#32256,#32257,#32258,
#32259,#32260,#32261,#32262,#32263,#32264,#32265,#32266,#32267,#32268,#32269,
#32270,#32271,#32272,#32273,#32274,#32275,#32276,#32277,#32278,#32279,#32280,
#32281,#32282,#32283,#32284,#32285,#32286,#32287,#32288,#32289,#32290,#32291,
#32292,#32293,#32294,#32295,#32296,#32297,#32298,#32299,#32300,#32301,#32302,
#32303,#32304,#32305,#32306,#32307,#32308,#32309,#32310,#32311,#32312,#32313),
 .UNSPECIFIED.,.F.,.F.,(4,3,3,3,3,3,3,3,3,3,3,3,3,3,3,3,3,3,3,3,3,3,3,3,
3,3,3,4),(0.,0.018594885873403,0.0384194798631932,0.0557659996042597,0.0644652503371223,
0.0684490524568481,0.0885013376974244,0.108910426790898,0.125980729541105,
0.133839897547683,0.137280413419243,0.158355507126299,0.177191637791725,
0.1977206197196,0.205647900544446,0.209124298098342,0.23013147760292,0.25162452459456,
0.268078695962123,0.278325048323282,0.284043739612251,0.306312804123555,
0.322962328214973,0.328177032612165,0.333185055167668,0.355706471451577,
0.372910900489228,0.37694081721157),.UNSPECIFIED.);
#890=B_SPLINE_CURVE_WITH_KNOTS('',3,(#32314,#32315,#32316,#32317,#32318,
#32319,#32320,#32321,#32322,#32323,#32324,#32325,#32326,#32327,#32328,#32329,
#32330,#32331,#32332,#32333,#32334,#32335,#32336,#32337,#32338),
 .UNSPECIFIED.,.F.,.F.,(4,3,3,3,3,3,3,3,4),(-10.1295685708712,-9.974986554505,
-8.9774878990545,-7.979989243604,-6.9824905881535,-5.984991932703,-4.9874932772525,
-3.989994621802,-3.84638326369162),.UNSPECIFIED.);
#891=B_SPLINE_CURVE_WITH_KNOTS('',3,(#32827,#32828,#32829,#32830,#32831,
#32832,#32833,#32834,#32835,#32836,#32837,#32838,#32839,#32840,#32841,#32842,
#32843,#32844,#32845,#32846,#32847,#32848),.UNSPECIFIED.,.F.,.F.,(4,3,3,
3,3,3,3,4),(7.59300756235069,7.979989243604,8.97748789905449,9.97498655450499,
10.9724852099555,11.969983865406,12.9674825208565,13.8761928695303),
 .UNSPECIFIED.);
#892=B_SPLINE_CURVE_WITH_KNOTS('',3,(#32849,#32850,#32851,#32852,#32853,
#32854,#32855,#32856,#32857,#32858,#32859,#32860,#32861,#32862,#32863,#32864,
#32865,#32866,#32867,#32868,#32869,#32870,#32871,#32872,#32873,#32874,#32875,
#32876,#32877,#32878,#32879,#32880,#32881,#32882,#32883,#32884,#32885,#32886,
#32887,#32888,#32889,#32890,#32891,#32892,#32893,#32894,#32895,#32896,#32897,
#32898,#32899,#32900,#32901,#32902,#32903,#32904,#32905,#32906,#32907,#32908,
#32909,#32910,#32911,#32912,#32913,#32914,#32915,#32916,#32917,#32918,#32919,
#32920,#32921,#32922,#32923,#32924,#32925,#32926,#32927,#32928,#32929,#32930,
#32931,#32932,#32933),.UNSPECIFIED.,.F.,.F.,(4,3,3,3,3,3,3,3,3,3,3,3,3,
3,3,3,3,3,3,3,3,3,3,3,3,3,3,3,4),(0.,0.0219639704547416,0.0445412096053718,
0.0636172943766679,0.0720964150895219,0.0767535446244105,0.0810482748727846,
0.102994889675057,0.124771807731429,0.142866327742507,0.150422049143916,
0.153915429401351,0.157566138461075,0.17833757213313,0.19714988777574,0.219420483792499,
0.224320878182838,0.22940319248336,0.250068207912569,0.270729023241509,
0.285676322508746,0.29689251627475,0.300623397883779,0.320396471336199,
0.334299980346825,0.338766705971823,0.357793075396352,0.375314655909808,
0.378621596831459),.UNSPECIFIED.);
#893=B_SPLINE_CURVE_WITH_KNOTS('',3,(#32936,#32937,#32938,#32939,#32940,
#32941,#32942,#32943,#32944,#32945,#32946,#32947,#32948,#32949,#32950,#32951,
#32952,#32953,#32954,#32955,#32956,#32957,#32958,#32959,#32960,#32961,#32962,
#32963,#32964,#32965,#32966,#32967,#32968,#32969,#32970,#32971,#32972,#32973,
#32974,#32975,#32976,#32977,#32978,#32979,#32980,#32981,#32982,#32983,#32984,
#32985,#32986,#32987,#32988,#32989,#32990,#32991,#32992,#32993,#32994,#32995,
#32996,#32997,#32998,#32999,#33000,#33001,#33002,#33003,#33004,#33005,#33006,
#33007,#33008,#33009,#33010,#33011,#33012,#33013,#33014,#33015,#33016,#33017,
#33018,#33019,#33020,#33021,#33022,#33023),.UNSPECIFIED.,.F.,.F.,(4,3,3,
3,3,3,3,3,3,3,3,3,3,3,3,3,3,3,3,3,3,3,3,3,3,3,3,3,3,4),(-0.378621596831415,
-0.359799982681486,-0.347867741892736,-0.339796092108079,-0.335415835589243,
-0.315546567792779,-0.301208643322146,-0.297330292477441,-0.293235380625517,
-0.272834922399814,-0.2521370543926,-0.23931358380138,-0.228820766465177,
-0.224509902039135,-0.203205281153447,-0.20084317202772,-0.18035428381319,
-0.158315823561941,-0.154363723715015,-0.150814783989309,-0.129430295261392,
-0.107595605944727,-0.0856289636990593,-0.0802080454028315,-0.0759455719174419,
-0.0533977626018103,-0.0308256449926057,-0.00876660921494158,-0.00404660180319711,
0.),.UNSPECIFIED.);
#894=B_SPLINE_CURVE_WITH_KNOTS('',3,(#33024,#33025,#33026,#33027,#33028,
#33029,#33030,#33031,#33032,#33033,#33034,#33035,#33036,#33037,#33038,#33039,
#33040,#33041,#33042,#33043,#33044,#33045,#33046,#33047,#33048,#33049,#33050,
#33051,#33052,#33053,#33054,#33055,#33056,#33057,#33058,#33059,#33060,#33061,
#33062,#33063,#33064,#33065,#33066,#33067,#33068,#33069,#33070,#33071,#33072,
#33073,#33074,#33075,#33076,#33077,#33078,#33079,#33080,#33081,#33082,#33083,
#33084,#33085,#33086,#33087,#33088,#33089,#33090,#33091,#33092,#33093,#33094,
#33095,#33096,#33097,#33098,#33099,#33100,#33101,#33102,#33103,#33104,#33105,
#33106,#33107,#33108),.UNSPECIFIED.,.F.,.F.,(4,3,3,3,3,3,3,3,3,3,3,3,3,
3,3,3,3,3,3,3,3,3,3,3,3,3,3,3,4),(-0.376940817211667,-0.35463587601936,
-0.332914950417388,-0.328066883946824,-0.305818289667664,-0.290199562359655,
-0.284267352350603,-0.278599940314396,-0.256916539828167,-0.235698322125015,
-0.214945667731477,-0.208192979048904,-0.20440287735044,-0.1838260654653,
-0.180868471203587,-0.159885877932906,-0.140312002588519,-0.136050825693189,
-0.132607233423575,-0.112148154257823,-0.0917831486981529,-0.0718536049354341,
-0.0676631265382839,-0.0636717646905323,-0.0441132683370721,-0.0249260984199674,
-0.00636124025136225,-0.00329487517780647,0.),.UNSPECIFIED.);
#895=B_SPLINE_CURVE_WITH_KNOTS('',3,(#33110,#33111,#33112,#33113,#33114,
#33115,#33116,#33117,#33118,#33119,#33120),.UNSPECIFIED.,.F.,.F.,(4,1,1,
1,1,1,1,1,4),(15.707963267949,15.8515746260587,16.8490732815092,17.8465719369597,
18.8440705924102,19.8415692478607,20.8390679033112,21.8365665587617,21.9911485751283),
 .UNSPECIFIED.);
#896=B_SPLINE_CURVE_WITH_KNOTS('',3,(#33121,#33122,#33123,#33124,#33125,
#33126,#33127,#33128,#33129,#33130),.UNSPECIFIED.,.F.,.F.,(4,1,1,1,1,1,
1,4),(15.707963267949,16.393138323678,17.3906369791285,18.388135634579,
19.3856342900295,20.38313294548,21.3806316009305,21.9911485751283),
 .UNSPECIFIED.);
#897=B_SPLINE_CURVE_WITH_KNOTS('',3,(#33619,#33620,#33621,#33622,#33623,
#33624,#33625,#33626,#33627,#33628,#33629,#33630,#33631,#33632,#33633,#33634,
#33635,#33636,#33637,#33638,#33639,#33640,#33641,#33642,#33643,#33644,#33645,
#33646,#33647,#33648,#33649,#33650,#33651,#33652,#33653,#33654,#33655,#33656,
#33657,#33658,#33659,#33660,#33661,#33662,#33663,#33664,#33665,#33666,#33667,
#33668,#33669,#33670,#33671,#33672,#33673,#33674,#33675,#33676,#33677,#33678,
#33679,#33680,#33681,#33682,#33683,#33684,#33685,#33686,#33687,#33688,#33689,
#33690,#33691,#33692,#33693,#33694,#33695,#33696,#33697,#33698,#33699,#33700),
 .UNSPECIFIED.,.F.,.F.,(4,3,3,3,3,3,3,3,3,3,3,3,3,3,3,3,3,3,3,3,3,3,3,3,
3,3,3,4),(0.,0.0185948935798831,0.0384194866063638,0.0557660055045345,0.0644652605573106,
0.0684490550799758,0.0885013458730424,0.108910437440259,0.125980737528127,
0.133839910140703,0.137280419791478,0.158355512918852,0.177191637791729,
0.197720615992758,0.205647898698541,0.20912429682451,0.230131471962516,
0.251624516628207,0.268078697930462,0.278325052897778,0.284043738565929,
0.306312802790669,0.322962327215306,0.328177030451769,0.333185054058664,
0.355706470426897,0.372910900489216,0.376940817211557),.UNSPECIFIED.);
#898=B_SPLINE_CURVE_WITH_KNOTS('',3,(#33701,#33702,#33703,#33704,#33705,
#33706,#33707,#33708,#33709,#33710,#33711,#33712,#33713,#33714,#33715,#33716,
#33717,#33718,#33719,#33720,#33721,#33722,#33723,#33724,#33725),
 .UNSPECIFIED.,.F.,.F.,(4,3,3,3,3,3,3,3,4),(-10.1295685708719,-9.97498655450499,
-8.97748789905449,-7.979989243604,-6.9824905881535,-5.984991932703,-4.9874932772525,
-3.989994621802,-3.84638326369226),.UNSPECIFIED.);
#899=B_SPLINE_CURVE_WITH_KNOTS('',3,(#34214,#34215,#34216,#34217,#34218,
#34219,#34220,#34221,#34222,#34223,#34224,#34225,#34226,#34227,#34228,#34229,
#34230,#34231,#34232,#34233,#34234,#34235),.UNSPECIFIED.,.F.,.F.,(4,3,3,
3,3,3,3,4),(7.59300756235133,7.979989243604,8.97748789905451,9.97498655450501,
10.9724852099555,11.969983865406,12.9674825208565,13.8761928695309),
 .UNSPECIFIED.);
#900=B_SPLINE_CURVE_WITH_KNOTS('',3,(#34236,#34237,#34238,#34239,#34240,
#34241,#34242,#34243,#34244,#34245,#34246,#34247,#34248,#34249,#34250,#34251,
#34252,#34253,#34254,#34255,#34256,#34257,#34258,#34259,#34260,#34261,#34262,
#34263,#34264,#34265,#34266,#34267,#34268,#34269,#34270,#34271,#34272,#34273,
#34274,#34275,#34276,#34277,#34278,#34279,#34280,#34281,#34282,#34283,#34284,
#34285,#34286,#34287,#34288,#34289,#34290,#34291,#34292,#34293,#34294,#34295,
#34296,#34297,#34298,#34299,#34300,#34301,#34302,#34303,#34304,#34305,#34306,
#34307,#34308,#34309,#34310,#34311,#34312,#34313,#34314,#34315,#34316,#34317,
#34318,#34319,#34320),.UNSPECIFIED.,.F.,.F.,(4,3,3,3,3,3,3,3,3,3,3,3,3,
3,3,3,3,3,3,3,3,3,3,3,3,3,3,3,4),(0.,0.0219639631218642,0.0445412014823461,
0.0636172872690209,0.0720964129740222,0.0767535401253322,0.0810482736599176,
0.1029948885196,0.124771808689427,0.142866328461006,0.150422048595144,0.153915426485005,
0.157566137611273,0.17833757339743,0.197149887775744,0.219420483792504,
0.224320878636298,0.229403192489738,0.250068207587221,0.270729023024861,
0.285676328241119,0.296892526281026,0.300623400781932,0.320396476514032,
0.334299989050446,0.338766713939552,0.357793087087158,0.375314655909825,
0.378621596831476),.UNSPECIFIED.);
#901=B_SPLINE_CURVE_WITH_KNOTS('',3,(#34323,#34324,#34325,#34326,#34327,
#34328,#34329,#34330,#34331,#34332,#34333,#34334,#34335,#34336,#34337,#34338,
#34339,#34340,#34341,#34342,#34343,#34344,#34345,#34346,#34347,#34348,#34349,
#34350,#34351,#34352,#34353,#34354,#34355,#34356,#34357,#34358,#34359,#34360,
#34361,#34362,#34363,#34364,#34365,#34366,#34367,#34368,#34369,#34370,#34371,
#34372,#34373,#34374,#34375,#34376,#34377,#34378,#34379,#34380,#34381,#34382,
#34383,#34384,#34385,#34386,#34387,#34388,#34389,#34390,#34391,#34392,#34393,
#34394,#34395,#34396,#34397,#34398,#34399,#34400,#34401,#34402,#34403,#34404,
#34405,#34406,#34407,#34408,#34409,#34410),.UNSPECIFIED.,.F.,.F.,(4,3,3,
3,3,3,3,3,3,3,3,3,3,3,3,3,3,3,3,3,3,3,3,3,3,3,3,3,3,4),(-0.378621596831342,
-0.359799978647325,-0.347867731642752,-0.339796002462411,-0.335415802350538,
-0.315546531014861,-0.301208611141465,-0.297330220816646,-0.293235373064883,
-0.272834912064565,-0.252137044356719,-0.239313576274462,-0.228820755338192,
-0.224509898510171,-0.203205277724662,-0.200843172027689,-0.180354286447876,
-0.158315825867291,-0.154363738841701,-0.1508147865132,-0.129430299930584,
-0.107595611579441,-0.0856289693581657,-0.0802080552723695,-0.0759455753061188,
-0.0533977664431355,-0.0308256487487178,-0.00876661335280336,-0.00404660180319768,
0.),.UNSPECIFIED.);
#902=B_SPLINE_CURVE_WITH_KNOTS('',3,(#34411,#34412,#34413,#34414,#34415,
#34416,#34417,#34418,#34419,#34420,#34421,#34422,#34423,#34424,#34425,#34426,
#34427,#34428,#34429,#34430,#34431,#34432,#34433,#34434,#34435,#34436,#34437,
#34438,#34439,#34440,#34441,#34442,#34443,#34444,#34445,#34446,#34447,#34448,
#34449,#34450,#34451,#34452,#34453,#34454,#34455,#34456,#34457,#34458,#34459,
#34460,#34461,#34462,#34463,#34464,#34465,#34466,#34467,#34468,#34469,#34470,
#34471,#34472,#34473,#34474,#34475,#34476,#34477,#34478,#34479,#34480,#34481,
#34482,#34483,#34484,#34485,#34486,#34487,#34488,#34489,#34490,#34491,#34492,
#34493,#34494,#34495),.UNSPECIFIED.,.F.,.F.,(4,3,3,3,3,3,3,3,3,3,3,3,3,
3,3,3,3,3,3,3,3,3,3,3,3,3,3,3,4),(-0.376940817211729,-0.354635873302002,
-0.332914948039702,-0.328066881211475,-0.305818286928304,-0.290199559962716,
-0.284267347028432,-0.278599940670464,-0.256916540583258,-0.235698323984283,
-0.21494567030162,-0.208192977306597,-0.204402877464087,-0.183826066657456,
-0.180868471203602,-0.159885877922097,-0.140312002579062,-0.13605082724227,
-0.132607234529552,-0.112148155157824,-0.0917831498359287,-0.0718536073792482,
-0.0676631334737326,-0.0636717668358761,-0.0441132711599333,-0.024926102814774,
-0.00636124727006412,-0.00329487517781668,0.),.UNSPECIFIED.);
#903=B_SPLINE_CURVE_WITH_KNOTS('',3,(#34497,#34498,#34499,#34500,#34501,
#34502,#34503,#34504,#34505,#34506,#34507),.UNSPECIFIED.,.F.,.F.,(4,1,1,
1,1,1,1,1,4),(15.707963267949,15.851574626059,16.8490732815095,17.84657193696,
18.8440705924105,19.841569247861,20.8390679033115,21.836566558762,21.9911485751283),
 .UNSPECIFIED.);
#904=B_SPLINE_CURVE_WITH_KNOTS('',3,(#34508,#34509,#34510,#34511,#34512,
#34513,#34514,#34515,#34516,#34517),.UNSPECIFIED.,.F.,.F.,(4,1,1,1,1,1,
1,4),(15.707963267949,16.3931383236783,17.3906369791288,18.3881356345793,
19.3856342900298,20.3831329454803,21.3806316009308,21.9911485751283),
 .UNSPECIFIED.);
#905=B_SPLINE_CURVE_WITH_KNOTS('',3,(#35006,#35007,#35008,#35009,#35010,
#35011,#35012,#35013,#35014,#35015,#35016,#35017,#35018,#35019,#35020,#35021,
#35022,#35023,#35024,#35025,#35026,#35027,#35028,#35029,#35030,#35031,#35032,
#35033,#35034,#35035,#35036,#35037,#35038,#35039,#35040,#35041,#35042,#35043,
#35044,#35045,#35046,#35047,#35048,#35049,#35050,#35051,#35052,#35053,#35054,
#35055,#35056,#35057,#35058,#35059,#35060,#35061,#35062,#35063,#35064,#35065,
#35066,#35067,#35068,#35069,#35070,#35071,#35072,#35073,#35074,#35075,#35076,
#35077,#35078,#35079,#35080,#35081,#35082,#35083,#35084,#35085,#35086,#35087),
 .UNSPECIFIED.,.F.,.F.,(4,3,3,3,3,3,3,3,3,3,3,3,3,3,3,3,3,3,3,3,3,3,3,3,
3,3,3,4),(0.,0.0185948979987812,0.0384194904729007,0.0557660088877552,0.0644652664176503,
0.0684490565818861,0.0885013505592445,0.108910443544607,0.12598074210639,
0.133839917359234,0.137280423449418,0.158355516244424,0.177191637791737,
0.197720613855199,0.205647897639485,0.209124296087971,0.230131468721749,
0.251624512053417,0.268078699062201,0.278325055529064,0.284043737962168,
0.306312802022573,0.322962326639242,0.328177029191476,0.333185053418253,
0.355706469834782,0.372910900489249,0.376940817211591),.UNSPECIFIED.);
#906=B_SPLINE_CURVE_WITH_KNOTS('',3,(#35088,#35089,#35090,#35091,#35092,
#35093,#35094,#35095,#35096,#35097,#35098,#35099,#35100,#35101,#35102,#35103,
#35104,#35105,#35106,#35107,#35108,#35109,#35110,#35111,#35112),
 .UNSPECIFIED.,.F.,.F.,(4,3,3,3,3,3,3,3,4),(-10.1295685708716,-9.974986554505,
-8.9774878990545,-7.979989243604,-6.9824905881535,-5.984991932703,-4.9874932772525,
-3.989994621802,-3.84638326369194),.UNSPECIFIED.);
#907=B_SPLINE_CURVE_WITH_KNOTS('',3,(#35601,#35602,#35603,#35604,#35605,
#35606,#35607,#35608,#35609,#35610,#35611,#35612,#35613,#35614,#35615,#35616,
#35617,#35618,#35619,#35620,#35621,#35622),.UNSPECIFIED.,.F.,.F.,(4,3,3,
3,3,3,3,4),(7.59300756235101,7.979989243604,8.97748789905451,9.974986554505,
10.9724852099555,11.969983865406,12.9674825208565,13.8761928695306),
 .UNSPECIFIED.);
#908=B_SPLINE_CURVE_WITH_KNOTS('',3,(#35623,#35624,#35625,#35626,#35627,
#35628,#35629,#35630,#35631,#35632,#35633,#35634,#35635,#35636,#35637,#35638,
#35639,#35640,#35641,#35642,#35643,#35644,#35645,#35646,#35647,#35648,#35649,
#35650,#35651,#35652,#35653,#35654,#35655,#35656,#35657,#35658,#35659,#35660,
#35661,#35662,#35663,#35664,#35665,#35666,#35667,#35668,#35669,#35670,#35671,
#35672,#35673,#35674,#35675,#35676,#35677,#35678,#35679,#35680,#35681,#35682,
#35683,#35684,#35685,#35686,#35687,#35688,#35689,#35690,#35691,#35692,#35693,
#35694,#35695,#35696,#35697,#35698,#35699,#35700,#35701,#35702,#35703,#35704,
#35705,#35706,#35707),.UNSPECIFIED.,.F.,.F.,(4,3,3,3,3,3,3,3,3,3,3,3,3,
3,3,3,3,3,3,3,3,3,3,3,3,3,3,3,4),(0.,0.0219639666312835,0.0445412053698155,
0.063617290670558,0.0720964139865945,0.0767535422787978,0.0810482742366969,
0.102994889069381,0.124771808227842,0.142866328114821,0.150422048856047,
0.153915427873857,0.157566138016919,0.178337572791375,0.197149887775755,
0.219420483792515,0.224320878419338,0.229403192482163,0.250068207738402,
0.270729023124161,0.285676325486174,0.29689252147315,0.300623399390804,
0.320396474032259,0.334299984879898,0.338766710117096,0.357793081483418,
0.375314655909829,0.378621596831479),.UNSPECIFIED.);
#909=B_SPLINE_CURVE_WITH_KNOTS('',3,(#35710,#35711,#35712,#35713,#35714,
#35715,#35716,#35717,#35718,#35719,#35720,#35721,#35722,#35723,#35724,#35725,
#35726,#35727,#35728,#35729,#35730,#35731,#35732,#35733,#35734,#35735,#35736,
#35737,#35738,#35739,#35740,#35741,#35742,#35743,#35744,#35745,#35746,#35747,
#35748,#35749,#35750,#35751,#35752,#35753,#35754,#35755,#35756,#35757,#35758,
#35759,#35760,#35761,#35762,#35763,#35764,#35765,#35766,#35767,#35768,#35769,
#35770,#35771,#35772,#35773,#35774,#35775,#35776,#35777,#35778,#35779,#35780,
#35781,#35782,#35783,#35784,#35785,#35786,#35787,#35788,#35789,#35790,#35791,
#35792,#35793,#35794,#35795,#35796,#35797),.UNSPECIFIED.,.F.,.F.,(4,3,3,
3,3,3,3,3,3,3,3,3,3,3,3,3,3,3,3,3,3,3,3,3,3,3,3,3,3,4),(-0.378621596831322,
-0.359799969507972,-0.347867708396688,-0.33979579913089,-0.335415727239428,
-0.315546447878259,-0.301208538396937,-0.297330058742659,-0.29323535595745,
-0.272834888678764,-0.252137021650703,-0.239313559244948,-0.228820730165096,
-0.224509890616438,-0.203205270049206,-0.200843172027682,-0.180354292423732,
-0.158315831096164,-0.154363773062407,-0.150814792225547,-0.129430310507984,
-0.107595624341076,-0.0856289821639265,-0.0802080776082638,-0.0759455830362766,
-0.0533977752247224,-0.0308256573292537,-0.00876662278122885,-0.00404660180318586,
0.),.UNSPECIFIED.);
#910=B_SPLINE_CURVE_WITH_KNOTS('',3,(#35798,#35799,#35800,#35801,#35802,
#35803,#35804,#35805,#35806,#35807,#35808,#35809,#35810,#35811,#35812,#35813,
#35814,#35815,#35816,#35817,#35818,#35819,#35820,#35821,#35822,#35823,#35824,
#35825,#35826,#35827,#35828,#35829,#35830,#35831,#35832,#35833,#35834,#35835,
#35836,#35837,#35838,#35839,#35840,#35841,#35842,#35843,#35844,#35845,#35846,
#35847,#35848,#35849,#35850,#35851,#35852,#35853,#35854,#35855,#35856,#35857,
#35858,#35859,#35860,#35861,#35862,#35863,#35864,#35865,#35866,#35867,#35868,
#35869,#35870,#35871,#35872,#35873,#35874,#35875,#35876,#35877,#35878,#35879,
#35880,#35881,#35882),.UNSPECIFIED.,.F.,.F.,(4,3,3,3,3,3,3,3,3,3,3,3,3,
3,3,3,3,3,3,3,3,3,3,3,3,3,3,3,4),(-0.376940817211723,-0.354635878503461,
-0.332914952590979,-0.328066886478521,-0.305818292205571,-0.290199564580325,
-0.284267357272115,-0.278599940003547,-0.256916539151692,-0.235698320438349,
-0.21494566539322,-0.208192980636845,-0.20440287701073,-0.183826064152281,
-0.180868471203602,-0.159885877939701,-0.140312002594464,-0.136050824265609,
-0.132607232292872,-0.112148153313923,-0.091783147541673,-0.0718536026117019,
-0.0676631199850014,-0.0636717626539058,-0.044113265676923,-0.024926094327708,
-0.00636123375821928,-0.00329487517780647,0.),.UNSPECIFIED.);
#911=B_SPLINE_CURVE_WITH_KNOTS('',3,(#35884,#35885,#35886,#35887,#35888,
#35889,#35890,#35891,#35892,#35893,#35894),.UNSPECIFIED.,.F.,.F.,(4,1,1,
1,1,1,1,1,4),(15.707963267949,15.851574626059,16.8490732815095,17.84657193696,
18.8440705924105,19.841569247861,20.8390679033115,21.836566558762,21.9911485751283),
 .UNSPECIFIED.);
#912=B_SPLINE_CURVE_WITH_KNOTS('',3,(#35895,#35896,#35897,#35898,#35899,
#35900,#35901,#35902,#35903,#35904),.UNSPECIFIED.,.F.,.F.,(4,1,1,1,1,1,
1,4),(15.707963267949,16.3931383236783,17.3906369791288,18.3881356345793,
19.3856342900298,20.3831329454803,21.3806316009308,21.9911485751283),
 .UNSPECIFIED.);
#913=B_SPLINE_CURVE_WITH_KNOTS('',3,(#36393,#36394,#36395,#36396,#36397,
#36398,#36399,#36400,#36401,#36402,#36403,#36404,#36405,#36406,#36407,#36408,
#36409,#36410,#36411,#36412,#36413,#36414,#36415,#36416,#36417,#36418,#36419,
#36420,#36421,#36422,#36423,#36424,#36425,#36426,#36427,#36428,#36429,#36430,
#36431,#36432,#36433,#36434,#36435,#36436,#36437,#36438,#36439,#36440,#36441,
#36442,#36443,#36444,#36445,#36446,#36447,#36448,#36449,#36450,#36451,#36452,
#36453,#36454,#36455,#36456,#36457,#36458,#36459,#36460,#36461,#36462,#36463,
#36464,#36465,#36466,#36467,#36468,#36469,#36470,#36471,#36472,#36473,#36474),
 .UNSPECIFIED.,.F.,.F.,(4,3,3,3,3,3,3,3,3,3,3,3,3,3,3,3,3,3,3,3,3,3,3,3,
3,3,3,4),(0.,0.0185948895377003,0.0384194830694538,0.0557660024097381,0.0644652551966428,
0.0684490537106689,0.0885013415914402,0.108910431860699,0.125980733343456,
0.133839903542633,0.13728041645897,0.158355509890479,0.177191637791728,
0.197720617947217,0.205647899666576,0.209124297504269,0.230131474933047,
0.25162452081887,0.268078696891712,0.278325050479978,0.284043739119617,
0.306312803494651,0.322962327743294,0.328177031572274,0.333185054637632,
0.355706470961523,0.372910900489225,0.376940817211566),.UNSPECIFIED.);
#914=B_SPLINE_CURVE_WITH_KNOTS('',3,(#36475,#36476,#36477,#36478,#36479,
#36480,#36481,#36482,#36483,#36484,#36485,#36486,#36487,#36488,#36489,#36490,
#36491,#36492,#36493,#36494,#36495,#36496,#36497,#36498,#36499),
 .UNSPECIFIED.,.F.,.F.,(4,3,3,3,3,3,3,3,4),(-10.1295685708716,-9.974986554505,
-8.9774878990545,-7.979989243604,-6.9824905881535,-5.984991932703,-4.9874932772525,
-3.989994621802,-3.84638326369194),.UNSPECIFIED.);
#915=B_SPLINE_CURVE_WITH_KNOTS('',3,(#36988,#36989,#36990,#36991,#36992,
#36993,#36994,#36995,#36996,#36997,#36998,#36999,#37000,#37001,#37002,#37003,
#37004,#37005,#37006,#37007,#37008,#37009),.UNSPECIFIED.,.F.,.F.,(4,3,3,
3,3,3,3,4),(7.59300756235101,7.979989243604,8.97748789905451,9.974986554505,
10.9724852099555,11.969983865406,12.9674825208565,13.8761928695306),
 .UNSPECIFIED.);
#916=B_SPLINE_CURVE_WITH_KNOTS('',3,(#37010,#37011,#37012,#37013,#37014,
#37015,#37016,#37017,#37018,#37019,#37020,#37021,#37022,#37023,#37024,#37025,
#37026,#37027,#37028,#37029,#37030,#37031,#37032,#37033,#37034,#37035,#37036,
#37037,#37038,#37039,#37040,#37041,#37042,#37043,#37044,#37045,#37046,#37047,
#37048,#37049,#37050,#37051,#37052,#37053,#37054,#37055,#37056,#37057,#37058,
#37059,#37060,#37061,#37062,#37063,#37064,#37065,#37066,#37067,#37068,#37069,
#37070,#37071,#37072,#37073,#37074,#37075,#37076,#37077,#37078,#37079,#37080,
#37081,#37082,#37083,#37084,#37085,#37086,#37087,#37088,#37089,#37090,#37091,
#37092,#37093,#37094),.UNSPECIFIED.,.F.,.F.,(4,3,3,3,3,3,3,3,3,3,3,3,3,
3,3,3,3,3,3,3,3,3,3,3,3,3,3,3,4),(0.,0.0219639745899241,0.0445412141859538,
0.0636172983846773,0.0720964162823181,0.0767535471614663,0.0810482755548609,
0.10299489032468,0.124771807189166,0.14286632733581,0.150422049452129,0.153915431031089,
0.157566138937898,0.178337571417637,0.197149887775741,0.219420483792501,
0.224320877927013,0.229403192462999,0.25006820807906,0.270729023346635,
0.285676319229185,0.296892510554946,0.300623396232423,0.320396468398677,
0.33429997541392,0.338766701437846,0.357793068763078,0.375314655909822,
0.378621596831473),.UNSPECIFIED.);
#917=B_SPLINE_CURVE_WITH_KNOTS('',3,(#37101,#37102,#37103,#37104,#37105,
#37106,#37107,#37108,#37109,#37110,#37111,#37112,#37113,#37114,#37115,#37116,
#37117,#37118,#37119,#37120,#37121,#37122,#37123,#37124,#37125,#37126,#37127,
#37128,#37129,#37130,#37131,#37132,#37133,#37134,#37135,#37136,#37137,#37138,
#37139,#37140,#37141,#37142,#37143,#37144,#37145,#37146,#37147,#37148,#37149,
#37150,#37151,#37152,#37153,#37154,#37155,#37156,#37157,#37158,#37159,#37160,
#37161,#37162,#37163,#37164,#37165,#37166,#37167,#37168,#37169,#37170,#37171,
#37172,#37173,#37174,#37175,#37176,#37177,#37178,#37179,#37180,#37181,#37182,
#37183,#37184,#37185,#37186,#37187,#37188),.UNSPECIFIED.,.F.,.F.,(4,3,3,
3,3,3,3,3,3,3,3,3,3,3,3,3,3,3,3,3,3,3,3,3,3,3,3,3,3,4),(-0.378621596831422,
-0.359796720372466,-0.347859447299365,-0.339722632399601,-0.335384312800265,
-0.315512099822729,-0.301178483848345,-0.297262500366189,-0.293227435760253,
-0.272824713995647,-0.252127134942234,-0.23930614421359,-0.228809794789834,
-0.224506446570609,-0.203201941946953,-0.200843172027657,-0.18035647359203,
-0.15831773961842,-0.154376205977353,-0.150816849886109,-0.129434137392224,
-0.107600238535838,-0.0856336136104227,-0.0802161718332497,-0.0759483538506766,
-0.0534009168486348,-0.0308287327199469,-0.00877004870084194,-0.00404660180315077,
0.),.UNSPECIFIED.);
#918=B_SPLINE_CURVE_WITH_KNOTS('',3,(#37189,#37190,#37191,#37192,#37193,
#37194,#37195,#37196,#37197,#37198,#37199,#37200,#37201,#37202,#37203,#37204,
#37205,#37206,#37207,#37208,#37209,#37210,#37211,#37212,#37213,#37214,#37215,
#37216,#37217,#37218,#37219,#37220,#37221,#37222,#37223,#37224,#37225,#37226,
#37227,#37228,#37229,#37230,#37231,#37232,#37233,#37234,#37235,#37236,#37237,
#37238,#37239,#37240,#37241,#37242,#37243,#37244,#37245,#37246,#37247,#37248,
#37249,#37250,#37251,#37252,#37253,#37254,#37255,#37256,#37257,#37258,#37259,
#37260,#37261,#37262,#37263,#37264,#37265,#37266,#37267,#37268,#37269,#37270,
#37271,#37272,#37273),.UNSPECIFIED.,.F.,.F.,(4,3,3,3,3,3,3,3,3,3,3,3,3,
3,3,3,3,3,3,3,3,3,3,3,3,3,3,3,4),(-0.376940817211671,-0.35463378592243,
-0.332913121582575,-0.328064780620112,-0.305816203186943,-0.290197736689024,
-0.284263301474814,-0.278600204901399,-0.25691713780292,-0.235699797645294,
-0.214947714870497,-0.208191635443227,-0.204403035574647,-0.183827074928476,
-0.180868471203591,-0.159885881087144,-0.140312005348477,-0.136052161826863,
-0.132608232099475,-0.112149009613445,-0.0917842308919543,-0.0718557743436045,
-0.0660574195493053,-0.0628401741813833,-0.0432952248143112,-0.0232950499960591,
-0.0047591197577418,-0.00329487517780703,0.),.UNSPECIFIED.);
#919=B_SPLINE_CURVE_WITH_KNOTS('',3,(#37275,#37276,#37277,#37278,#37279,
#37280,#37281,#37282,#37283,#37284,#37285),.UNSPECIFIED.,.F.,.F.,(4,1,1,
1,1,1,1,1,4),(15.7079632679488,15.8515746260587,16.8490732815092,17.8465719369597,
18.8440705924102,19.8415692478607,20.8390679033112,21.8365665587617,21.9911485751284),
 .UNSPECIFIED.);
#920=B_SPLINE_CURVE_WITH_KNOTS('',3,(#37286,#37287,#37288,#37289,#37290,
#37291,#37292,#37293,#37294,#37295),.UNSPECIFIED.,.F.,.F.,(4,1,1,1,1,1,
1,4),(15.7079632679489,16.3931383236779,17.3906369791284,18.3881356345789,
19.3856342900294,20.3831329454799,21.3806316009304,21.9911485751284),
 .UNSPECIFIED.);
#921=B_SPLINE_CURVE_WITH_KNOTS('',3,(#37784,#37785,#37786,#37787,#37788,
#37789,#37790,#37791,#37792,#37793,#37794,#37795,#37796,#37797,#37798,#37799,
#37800,#37801,#37802,#37803,#37804,#37805,#37806,#37807,#37808,#37809,#37810,
#37811,#37812,#37813,#37814,#37815,#37816,#37817,#37818,#37819,#37820,#37821,
#37822,#37823,#37824,#37825,#37826,#37827,#37828,#37829,#37830,#37831,#37832,
#37833,#37834,#37835,#37836,#37837,#37838,#37839,#37840,#37841,#37842,#37843,
#37844,#37845,#37846,#37847,#37848,#37849,#37850,#37851,#37852,#37853,#37854,
#37855,#37856,#37857,#37858,#37859,#37860,#37861,#37862,#37863,#37864,#37865),
 .UNSPECIFIED.,.F.,.F.,(4,3,3,3,3,3,3,3,3,3,3,3,3,3,3,3,3,3,3,3,3,3,3,3,
3,3,3,4),(0.,0.0185983140321727,0.0384224795021175,0.0557686242883193,0.0644697932614127,
0.0684502210277478,0.0885049607621097,0.108915120509374,0.125984249829963,
0.13384544115498,0.137283243835269,0.158358039582652,0.177191637791731,
0.197718921929196,0.205647026423371,0.209123684847396,0.230128871311592,
0.25162086484219,0.268079555535016,0.278327028951233,0.284043271874226,
0.306312209751215,0.32296188243573,0.32817603610564,0.333184545813206,0.35570598540302,
0.372910900489273,0.376940817211655),.UNSPECIFIED.);
#922=B_SPLINE_CURVE_WITH_KNOTS('',3,(#37866,#37867,#37868,#37869,#37870,
#37871,#37872,#37873,#37874,#37875,#37876,#37877,#37878,#37879,#37880,#37881,
#37882,#37883,#37884,#37885,#37886,#37887,#37888,#37889,#37890),
 .UNSPECIFIED.,.F.,.F.,(4,3,3,3,3,3,3,3,4),(-10.1295685708718,-9.97498655450501,
-8.97748789905451,-7.97998924360401,-6.98249058815351,-5.98499193270301,
-4.98749327725251,-3.98999462180201,-3.84638326369218),.UNSPECIFIED.);
#923=B_SPLINE_CURVE_WITH_KNOTS('',3,(#38379,#38380,#38381,#38382,#38383,
#38384,#38385,#38386,#38387,#38388,#38389,#38390,#38391,#38392,#38393,#38394,
#38395,#38396,#38397,#38398,#38399,#38400),.UNSPECIFIED.,.F.,.F.,(4,3,3,
3,3,3,3,4),(7.59300756235149,7.97998924360401,8.97748789905451,9.97498655450502,
10.9724852099555,11.969983865406,12.9674825208565,13.8761928695311),
 .UNSPECIFIED.);
#924=B_SPLINE_CURVE_WITH_KNOTS('',3,(#38401,#38402,#38403,#38404,#38405,
#38406,#38407,#38408,#38409,#38410,#38411,#38412,#38413,#38414,#38415,#38416,
#38417,#38418,#38419,#38420,#38421,#38422,#38423,#38424,#38425,#38426,#38427,
#38428,#38429,#38430,#38431,#38432,#38433,#38434,#38435,#38436,#38437,#38438,
#38439,#38440,#38441,#38442,#38443,#38444,#38445,#38446,#38447,#38448,#38449,
#38450,#38451,#38452,#38453,#38454,#38455,#38456,#38457,#38458,#38459,#38460,
#38461,#38462,#38463,#38464,#38465,#38466,#38467,#38468,#38469,#38470,#38471,
#38472,#38473,#38474,#38475,#38476,#38477,#38478,#38479,#38480,#38481,#38482,
#38483,#38484,#38485),.UNSPECIFIED.,.F.,.F.,(4,3,3,3,3,3,3,3,3,3,3,3,3,
3,3,3,3,3,3,3,3,3,3,3,3,3,3,3,4),(0.,0.0219667982761558,0.0445443217220367,
0.0636200174787497,0.0720972266024481,0.0767552653548233,0.0810487382353878,
0.102995309296695,0.124771387449721,0.142866012531226,0.150422220722031,
0.153916412782485,0.157566438108027,0.178337033896873,0.197149887775741,
0.219420483792492,0.224320671605659,0.229403188154647,0.250068321092155,
0.270729057144868,0.285673893016582,0.296888246100129,0.300622182306411,
0.32039429496601,0.334296359328725,0.33876343006628,0.357788259279217,0.375314655909755,
0.378621596831423),.UNSPECIFIED.);
#925=B_SPLINE_CURVE_WITH_KNOTS('',3,(#38488,#38489,#38490,#38491,#38492,
#38493,#38494,#38495,#38496,#38497,#38498,#38499,#38500,#38501,#38502,#38503,
#38504,#38505,#38506,#38507,#38508,#38509,#38510,#38511,#38512,#38513,#38514,
#38515,#38516,#38517,#38518,#38519,#38520,#38521,#38522,#38523,#38524,#38525,
#38526,#38527,#38528,#38529,#38530,#38531,#38532,#38533,#38534,#38535,#38536,
#38537,#38538,#38539,#38540,#38541,#38542,#38543,#38544,#38545,#38546,#38547,
#38548,#38549,#38550,#38551,#38552,#38553,#38554,#38555,#38556,#38557,#38558,
#38559,#38560,#38561,#38562,#38563,#38564,#38565,#38566,#38567,#38568,#38569,
#38570,#38571,#38572,#38573,#38574,#38575),.UNSPECIFIED.,.F.,.F.,(4,3,3,
3,3,3,3,3,3,3,3,3,3,3,3,3,3,3,3,3,3,3,3,3,3,3,3,3,3,4),(-0.378621596831422,
-0.359796715870711,-0.347859435880365,-0.339722530007006,-0.335384262776704,
-0.315512045618215,-0.301178436419395,-0.29726239278539,-0.29322742189176,
-0.272824696964274,-0.252127118373726,-0.239306131787209,-0.228809776489813,
-0.224506440767185,-0.20320193635774,-0.200843172027657,-0.180356476691574,
-0.158317742330522,-0.154376223555756,-0.150816852768337,-0.129434142783147,
-0.107600245031064,-0.0856336201278072,-0.080216183244537,-0.0759483577713782,
-0.0534009212866121,-0.0308287370694683,-0.00877005360278791,-0.00404660180315077,
0.),.UNSPECIFIED.);
#926=B_SPLINE_CURVE_WITH_KNOTS('',3,(#38576,#38577,#38578,#38579,#38580,
#38581,#38582,#38583,#38584,#38585,#38586,#38587,#38588,#38589,#38590,#38591,
#38592,#38593,#38594,#38595,#38596,#38597,#38598,#38599,#38600,#38601,#38602,
#38603,#38604,#38605,#38606,#38607,#38608,#38609,#38610,#38611,#38612,#38613,
#38614,#38615,#38616,#38617,#38618,#38619,#38620,#38621,#38622,#38623,#38624,
#38625,#38626,#38627,#38628,#38629,#38630,#38631,#38632,#38633,#38634,#38635,
#38636,#38637,#38638,#38639,#38640,#38641,#38642,#38643,#38644,#38645,#38646,
#38647,#38648,#38649,#38650,#38651,#38652,#38653,#38654,#38655,#38656,#38657,
#38658,#38659,#38660),.UNSPECIFIED.,.F.,.F.,(4,3,3,3,3,3,3,3,3,3,3,3,3,
3,3,3,3,3,3,3,3,3,3,3,3,3,3,3,4),(-0.376940817211671,-0.354633785210935,
-0.332913120960017,-0.328064779829376,-0.305816202409768,-0.290197736008996,
-0.284263299980245,-0.278600205016827,-0.256917138043544,-0.235699798192756,
-0.214947715616542,-0.208191634969854,-0.20440303563573,-0.183827075288029,
-0.180868471203591,-0.159885881090851,-0.14031200535172,-0.136052162326922,
-0.132608232466673,-0.112149009937429,-0.0917842313090905,-0.071855775169603,
-0.0660574218689477,-0.0628401747625342,-0.0432952256330311,-0.0232950504054191,
-0.00475912097892364,-0.00329487517780703,0.),.UNSPECIFIED.);
#927=B_SPLINE_CURVE_WITH_KNOTS('',3,(#38662,#38663,#38664,#38665,#38666,
#38667,#38668,#38669,#38670,#38671,#38672),.UNSPECIFIED.,.F.,.F.,(4,1,1,
1,1,1,1,1,4),(15.7079632679488,15.8515746260587,16.8490732815092,17.8465719369597,
18.8440705924102,19.8415692478607,20.8390679033112,21.8365665587617,21.9911485751284),
 .UNSPECIFIED.);
#928=B_SPLINE_CURVE_WITH_KNOTS('',3,(#38673,#38674,#38675,#38676,#38677,
#38678,#38679,#38680,#38681,#38682),.UNSPECIFIED.,.F.,.F.,(4,1,1,1,1,1,
1,4),(15.7079632679489,16.3931383236779,17.3906369791284,18.3881356345789,
19.3856342900294,20.3831329454799,21.3806316009304,21.9911485751284),
 .UNSPECIFIED.);
#929=B_SPLINE_CURVE_WITH_KNOTS('',3,(#39171,#39172,#39173,#39174,#39175,
#39176,#39177,#39178,#39179,#39180,#39181,#39182,#39183,#39184,#39185,#39186,
#39187,#39188,#39189,#39190,#39191,#39192,#39193,#39194,#39195,#39196,#39197,
#39198,#39199,#39200,#39201,#39202,#39203,#39204,#39205,#39206,#39207,#39208,
#39209,#39210,#39211,#39212,#39213,#39214,#39215,#39216,#39217,#39218,#39219,
#39220,#39221,#39222,#39223,#39224,#39225,#39226,#39227,#39228,#39229,#39230,
#39231,#39232,#39233,#39234,#39235,#39236,#39237,#39238,#39239,#39240,#39241,
#39242,#39243,#39244,#39245,#39246,#39247,#39248,#39249,#39250,#39251,#39252),
 .UNSPECIFIED.,.F.,.F.,(4,3,3,3,3,3,3,3,3,3,3,3,3,3,3,3,3,3,3,3,3,3,3,3,
3,3,3,4),(0.,0.018598315202886,0.0384224805264917,0.0557686251846467,0.0644697948116091,
0.0684502214259709,0.0885049619928401,0.108915122095826,0.125984251019803,
0.133845443026534,0.137283244809287,0.158358040441789,0.177191637791731,
0.197718921336747,0.205647026107811,0.209123684625284,0.230128870392712,
0.251620863557925,0.268079555819901,0.278327029600694,0.284043271715027,
0.306312209549515,0.322961882284454,0.328176035756772,0.33318454563508,
0.355705985227969,0.372910900489273,0.376940817211655),.UNSPECIFIED.);
#930=B_SPLINE_CURVE_WITH_KNOTS('',3,(#39253,#39254,#39255,#39256,#39257,
#39258,#39259,#39260,#39261,#39262,#39263,#39264,#39265,#39266,#39267,#39268,
#39269,#39270,#39271,#39272,#39273,#39274,#39275,#39276,#39277),
 .UNSPECIFIED.,.F.,.F.,(4,3,3,3,3,3,3,3,4),(-10.1295685708718,-9.97498655450501,
-8.97748789905451,-7.97998924360401,-6.98249058815351,-5.98499193270301,
-4.98749327725251,-3.98999462180201,-3.84638326369218),.UNSPECIFIED.);
#931=B_SPLINE_CURVE_WITH_KNOTS('',3,(#39766,#39767,#39768,#39769,#39770,
#39771,#39772,#39773,#39774,#39775,#39776,#39777,#39778,#39779,#39780,#39781,
#39782,#39783,#39784,#39785,#39786,#39787),.UNSPECIFIED.,.F.,.F.,(4,3,3,
3,3,3,3,4),(7.59300756235149,7.97998924360401,8.97748789905451,9.97498655450502,
10.9724852099555,11.969983865406,12.9674825208565,13.8761928695311),
 .UNSPECIFIED.);
#932=B_SPLINE_CURVE_WITH_KNOTS('',3,(#39788,#39789,#39790,#39791,#39792,
#39793,#39794,#39795,#39796,#39797,#39798,#39799,#39800,#39801,#39802,#39803,
#39804,#39805,#39806,#39807,#39808,#39809,#39810,#39811,#39812,#39813,#39814,
#39815,#39816,#39817,#39818,#39819,#39820,#39821,#39822,#39823,#39824,#39825,
#39826,#39827,#39828,#39829,#39830,#39831,#39832,#39833,#39834,#39835,#39836,
#39837,#39838,#39839,#39840,#39841,#39842,#39843,#39844,#39845,#39846,#39847,
#39848,#39849,#39850,#39851,#39852,#39853,#39854,#39855,#39856,#39857,#39858,
#39859,#39860,#39861,#39862,#39863,#39864,#39865,#39866,#39867,#39868,#39869,
#39870,#39871,#39872),.UNSPECIFIED.,.F.,.F.,(4,3,3,3,3,3,3,3,3,3,3,3,3,
3,3,3,3,3,3,3,3,3,3,3,3,3,3,3,4),(0.,0.0219668021829663,0.0445443259943986,
0.0636200212170664,0.072097227717834,0.0767552677136324,0.0810487388755533,
0.102995309847675,0.124771386807676,0.142866012049692,0.150422220909751,
0.153916413967334,0.157566438486861,0.178337033089236,0.197149887775741,
0.219420483792492,0.224320671278011,0.229403188144959,0.250068321231503,
0.27072905712376,0.285673889363844,0.296888239638748,0.300622180494816,
0.320394291714806,0.33429635396776,0.33876342528417,0.357788252225625,0.375314655909755,
0.378621596831423),.UNSPECIFIED.);
#933=B_SPLINE_CURVE_WITH_KNOTS('',3,(#39875,#39876,#39877,#39878,#39879,
#39880,#39881,#39882,#39883,#39884,#39885,#39886,#39887,#39888,#39889,#39890,
#39891,#39892,#39893,#39894,#39895,#39896,#39897,#39898,#39899,#39900,#39901,
#39902,#39903,#39904,#39905,#39906,#39907,#39908,#39909,#39910,#39911,#39912,
#39913,#39914,#39915,#39916,#39917,#39918,#39919,#39920,#39921,#39922,#39923,
#39924,#39925,#39926,#39927,#39928,#39929,#39930,#39931,#39932,#39933,#39934,
#39935,#39936,#39937,#39938,#39939,#39940,#39941,#39942,#39943,#39944,#39945,
#39946,#39947,#39948,#39949,#39950,#39951,#39952,#39953,#39954,#39955,#39956,
#39957,#39958,#39959,#39960,#39961,#39962),.UNSPECIFIED.,.F.,.F.,(4,3,3,
3,3,3,3,3,3,3,3,3,3,3,3,3,3,3,3,3,3,3,3,3,3,3,3,3,3,4),(-0.378621596831447,
-0.359796710872288,-0.347859423166103,-0.33972241597309,-0.335384206951527,
-0.315511985148213,-0.301178383508145,-0.297262272762722,-0.293227406416186,
-0.272824677970899,-0.252127099894785,-0.239306117928005,-0.228809756083023,
-0.224506434279775,-0.20320193009925,-0.200843172027666,-0.180356480134043,
-0.158317745342681,-0.154376243245955,-0.15081685599556,-0.129434148792156,
-0.107600252262854,-0.0856336273826065,-0.0802161959430344,-0.0759483620831669,
-0.0534009261697563,-0.0308287418563685,-0.00877005900130109,-0.00404660180315016,
0.),.UNSPECIFIED.);
#934=B_SPLINE_CURVE_WITH_KNOTS('',3,(#39963,#39964,#39965,#39966,#39967,
#39968,#39969,#39970,#39971,#39972,#39973,#39974,#39975,#39976,#39977,#39978,
#39979,#39980,#39981,#39982,#39983,#39984,#39985,#39986,#39987,#39988,#39989,
#39990,#39991,#39992,#39993,#39994,#39995,#39996,#39997,#39998,#39999,#40000,
#40001,#40002,#40003,#40004,#40005,#40006,#40007,#40008,#40009,#40010,#40011,
#40012,#40013,#40014,#40015,#40016,#40017,#40018,#40019,#40020,#40021,#40022,
#40023,#40024,#40025,#40026,#40027,#40028,#40029,#40030,#40031,#40032,#40033,
#40034,#40035,#40036,#40037,#40038,#40039,#40040,#40041,#40042,#40043,#40044,
#40045,#40046,#40047),.UNSPECIFIED.,.F.,.F.,(4,3,3,3,3,3,3,3,3,3,3,3,3,
3,3,3,3,3,3,3,3,3,3,3,3,3,3,3,4),(-0.376940817211671,-0.354633792851345,
-0.332913127645376,-0.328064787566693,-0.305816210006314,-0.290197742655974,
-0.284263314719502,-0.278600204072656,-0.256917135797309,-0.235699792648004,
-0.214947707908054,-0.208191639892869,-0.204403035028373,-0.183827071480399,
-0.180868471203591,-0.159885881051101,-0.140312005316939,-0.136052156980596,
-0.132608228475344,-0.112149006418658,-0.0917842267934174,-0.0718557663450377,
-0.0660573970583436,-0.0628401685443772,-0.0432952168894413,-0.0232950460336242,
-0.00475910796593208,-0.00329487517780703,0.),.UNSPECIFIED.);
#935=B_SPLINE_CURVE_WITH_KNOTS('',3,(#40049,#40050,#40051,#40052,#40053,
#40054,#40055,#40056,#40057,#40058,#40059),.UNSPECIFIED.,.F.,.F.,(4,1,1,
1,1,1,1,1,4),(15.7079632679488,15.8515746260587,16.8490732815092,17.8465719369597,
18.8440705924102,19.8415692478607,20.8390679033112,21.8365665587617,21.9911485751284),
 .UNSPECIFIED.);
#936=B_SPLINE_CURVE_WITH_KNOTS('',3,(#40060,#40061,#40062,#40063,#40064,
#40065,#40066,#40067,#40068,#40069),.UNSPECIFIED.,.F.,.F.,(4,1,1,1,1,1,
1,4),(15.7079632679489,16.3931383236779,17.3906369791284,18.3881356345789,
19.3856342900294,20.3831329454799,21.3806316009304,21.9911485751284),
 .UNSPECIFIED.);
#937=B_SPLINE_CURVE_WITH_KNOTS('',3,(#40558,#40559,#40560,#40561,#40562,
#40563,#40564,#40565,#40566,#40567,#40568,#40569,#40570,#40571,#40572,#40573,
#40574,#40575,#40576,#40577,#40578,#40579,#40580,#40581,#40582,#40583,#40584,
#40585,#40586,#40587,#40588,#40589,#40590,#40591,#40592,#40593,#40594,#40595,
#40596,#40597,#40598,#40599,#40600,#40601,#40602,#40603,#40604,#40605,#40606,
#40607,#40608,#40609,#40610,#40611,#40612,#40613,#40614,#40615,#40616,#40617,
#40618,#40619,#40620,#40621,#40622,#40623,#40624,#40625,#40626,#40627,#40628,
#40629,#40630,#40631,#40632,#40633,#40634,#40635,#40636,#40637,#40638,#40639),
 .UNSPECIFIED.,.F.,.F.,(4,3,3,3,3,3,3,3,3,3,3,3,3,3,3,3,3,3,3,3,3,3,3,3,
3,3,3,4),(0.,0.0185983026316204,0.0384224695266343,0.0557686155597714,0.0644697781641698,
0.0684502171318133,0.088504948753686,0.10891510503595,0.125984238224895,
0.133845422901441,0.137283234431239,0.158358031297179,0.177191637791731,
0.197718927698151,0.205647029496634,0.209123687024891,0.230128880274258,
0.251620877362912,0.268079552746722,0.278327022586856,0.284043273416826,
0.306312211709011,0.322961883904076,0.328176039524306,0.333184547554318,
0.355705987113168,0.372910900489273,0.376940817211655),.UNSPECIFIED.);
#938=B_SPLINE_CURVE_WITH_KNOTS('',3,(#40640,#40641,#40642,#40643,#40644,
#40645,#40646,#40647,#40648,#40649,#40650,#40651,#40652,#40653,#40654,#40655,
#40656,#40657,#40658,#40659,#40660,#40661,#40662,#40663,#40664),
 .UNSPECIFIED.,.F.,.F.,(4,3,3,3,3,3,3,3,4),(-10.1295685708718,-9.97498655450501,
-8.97748789905451,-7.97998924360401,-6.98249058815351,-5.98499193270301,
-4.98749327725251,-3.98999462180201,-3.84638326369218),.UNSPECIFIED.);
#939=B_SPLINE_CURVE_WITH_KNOTS('',3,(#41153,#41154,#41155,#41156,#41157,
#41158,#41159,#41160,#41161,#41162,#41163,#41164,#41165,#41166,#41167,#41168,
#41169,#41170,#41171,#41172,#41173,#41174),.UNSPECIFIED.,.F.,.F.,(4,3,3,
3,3,3,3,4),(7.59300756235149,7.97998924360401,8.97748789905451,9.97498655450501,
10.9724852099555,11.969983865406,12.9674825208565,13.8761928695311),
 .UNSPECIFIED.);
#940=B_SPLINE_CURVE_WITH_KNOTS('',3,(#41175,#41176,#41177,#41178,#41179,
#41180,#41181,#41182,#41183,#41184,#41185,#41186,#41187,#41188,#41189,#41190,
#41191,#41192,#41193,#41194,#41195,#41196,#41197,#41198,#41199,#41200,#41201,
#41202,#41203,#41204,#41205,#41206,#41207,#41208,#41209,#41210,#41211,#41212,
#41213,#41214,#41215,#41216,#41217,#41218,#41219,#41220,#41221,#41222,#41223,
#41224,#41225,#41226,#41227,#41228,#41229,#41230,#41231,#41232,#41233,#41234,
#41235,#41236,#41237,#41238,#41239,#41240,#41241,#41242,#41243,#41244,#41245,
#41246,#41247,#41248,#41249,#41250,#41251,#41252,#41253,#41254,#41255,#41256,
#41257,#41258,#41259),.UNSPECIFIED.,.F.,.F.,(4,3,3,3,3,3,3,3,3,3,3,3,3,
3,3,3,3,3,3,3,3,3,3,3,3,3,3,3,4),(0.,0.0219668065215099,0.044544330738594,
0.063620025368238,0.0720972289566785,0.0767552703331067,0.0810487395771697,
0.102995310450109,0.124771386085693,0.142866011508206,0.150422221112997,
0.153916415282172,0.157566438907463,0.178337032192192,0.197149887775746,
0.219420483792496,0.224320670914036,0.229403188139166,0.250068321391114,
0.270729057104618,0.28567388531636,0.29688823247747,0.300622178485964,0.320394288107146,
0.334296348018114,0.338763419960212,0.357788244378528,0.375314655909751,
0.378621596831419),.UNSPECIFIED.);
#941=B_SPLINE_CURVE_WITH_KNOTS('',3,(#41262,#41263,#41264,#41265,#41266,
#41267,#41268,#41269,#41270,#41271,#41272,#41273,#41274,#41275,#41276,#41277,
#41278,#41279,#41280,#41281,#41282,#41283,#41284,#41285,#41286,#41287,#41288,
#41289,#41290,#41291,#41292,#41293,#41294,#41295,#41296,#41297,#41298,#41299,
#41300,#41301,#41302,#41303,#41304,#41305,#41306,#41307,#41308,#41309,#41310,
#41311,#41312,#41313,#41314,#41315,#41316,#41317,#41318,#41319,#41320,#41321,
#41322,#41323,#41324,#41325,#41326,#41327,#41328,#41329,#41330,#41331,#41332,
#41333,#41334,#41335,#41336,#41337,#41338,#41339,#41340,#41341,#41342,#41343,
#41344,#41345,#41346,#41347,#41348,#41349),.UNSPECIFIED.,.F.,.F.,(4,3,3,
3,3,3,3,3,3,3,3,3,3,3,3,3,3,3,3,3,3,3,3,3,3,3,3,3,3,4),(-0.378621596831452,
-0.359796705378914,-0.347859409196764,-0.339722290714836,-0.335384145609123,
-0.315511918694978,-0.301178325361564,-0.297262140747381,-0.293227389389929,
-0.272824657081609,-0.252127079571064,-0.239306102685213,-0.228809733635619,
-0.224506427219249,-0.203201923301277,-0.200843172027663,-0.180356483920826,
-0.158317748656117,-0.15437626458939,-0.150816859497235,-0.129434155353511,
-0.107600260175084,-0.0856336353261905,-0.0802162098561028,-0.0759483668387633,
-0.0534009315506567,-0.0308287471341723,-0.00877006494761552,-0.00404660180315015,
0.),.UNSPECIFIED.);
#942=B_SPLINE_CURVE_WITH_KNOTS('',3,(#41350,#41351,#41352,#41353,#41354,
#41355,#41356,#41357,#41358,#41359,#41360,#41361,#41362,#41363,#41364,#41365,
#41366,#41367,#41368,#41369,#41370,#41371,#41372,#41373,#41374,#41375,#41376,
#41377,#41378,#41379,#41380,#41381,#41382,#41383,#41384,#41385,#41386,#41387,
#41388,#41389,#41390,#41391,#41392,#41393,#41394,#41395,#41396,#41397,#41398,
#41399,#41400,#41401,#41402,#41403,#41404,#41405,#41406,#41407,#41408,#41409,
#41410,#41411,#41412,#41413,#41414,#41415,#41416,#41417,#41418,#41419,#41420,
#41421,#41422,#41423,#41424,#41425,#41426,#41427,#41428,#41429,#41430,#41431,
#41432,#41433,#41434),.UNSPECIFIED.,.F.,.F.,(4,3,3,3,3,3,3,3,3,3,3,3,3,
3,3,3,3,3,3,3,3,3,3,3,3,3,3,3,4),(-0.37694081721169,-0.354633789541522,
-0.332913124749281,-0.328064784261468,-0.305816206760707,-0.290197739816068,
-0.284263308414124,-0.278600204509387,-0.256917136791431,-0.235699795068636,
-0.21494771125805,-0.208191637754358,-0.20440303529233,-0.183827073127399,
-0.180868471203594,-0.159885881066344,-0.140312005330277,-0.136052159286264,
-0.132608230235817,-0.112149007974764,-0.0917842287792549,-0.0718557701882082,
-0.0660574078525838,-0.0628401712479354,-0.0432952206848533,-0.0232950479313323,
-0.004759113596582,-0.00329487517781129,0.),.UNSPECIFIED.);
#943=B_SPLINE_CURVE_WITH_KNOTS('',3,(#41436,#41437,#41438,#41439,#41440,
#41441,#41442,#41443,#41444,#41445,#41446),.UNSPECIFIED.,.F.,.F.,(4,1,1,
1,1,1,1,1,4),(15.7079632679489,15.8515746260587,16.8490732815092,17.8465719369597,
18.8440705924102,19.8415692478607,20.8390679033112,21.8365665587617,21.9911485751284),
 .UNSPECIFIED.);
#944=B_SPLINE_CURVE_WITH_KNOTS('',3,(#41447,#41448,#41449,#41450,#41451,
#41452,#41453,#41454,#41455,#41456),.UNSPECIFIED.,.F.,.F.,(4,1,1,1,1,1,
1,4),(15.7079632679489,16.3931383236779,17.3906369791284,18.3881356345789,
19.3856342900294,20.3831329454799,21.3806316009304,21.9911485751284),
 .UNSPECIFIED.);
#945=B_SPLINE_CURVE_WITH_KNOTS('',3,(#41945,#41946,#41947,#41948,#41949,
#41950,#41951,#41952,#41953,#41954,#41955,#41956,#41957,#41958,#41959,#41960,
#41961,#41962,#41963,#41964,#41965,#41966,#41967,#41968,#41969,#41970,#41971,
#41972,#41973,#41974,#41975,#41976,#41977,#41978,#41979,#41980,#41981,#41982,
#41983,#41984,#41985,#41986,#41987,#41988,#41989,#41990,#41991,#41992,#41993,
#41994,#41995,#41996,#41997,#41998,#41999,#42000,#42001,#42002,#42003,#42004,
#42005,#42006,#42007,#42008,#42009,#42010,#42011,#42012,#42013,#42014,#42015,
#42016,#42017,#42018,#42019,#42020,#42021,#42022,#42023,#42024,#42025,#42026),
 .UNSPECIFIED.,.F.,.F.,(4,3,3,3,3,3,3,3,3,3,3,3,3,3,3,3,3,3,3,3,3,3,3,3,
3,3,3,4),(0.,0.0185983080711966,0.0384224742862614,0.0557686197244432,0.064469785367515,
0.0684502189902693,0.0885049544828708,0.108915112418223,0.125984243761596,
0.133845431610119,0.137283238917139,0.158358035249346,0.177191637791715,
0.197718924945687,0.205647028030362,0.20912368598177,0.230128875993472,
0.251620871384311,0.268079554079538,0.278327025631043,0.284043272680096,
0.306312210774225,0.32296188320297,0.328176037890519,0.333184546722924,
0.355705986296573,0.372910900489207,0.37694081721159),.UNSPECIFIED.);
#946=B_SPLINE_CURVE_WITH_KNOTS('',3,(#42027,#42028,#42029,#42030,#42031,
#42032,#42033,#42034,#42035,#42036,#42037,#42038,#42039,#42040,#42041,#42042,
#42043,#42044,#42045,#42046,#42047,#42048,#42049,#42050,#42051),
 .UNSPECIFIED.,.F.,.F.,(4,3,3,3,3,3,3,3,4),(-10.1295685708718,-9.97498655450501,
-8.97748789905451,-7.97998924360401,-6.98249058815351,-5.98499193270301,
-4.98749327725251,-3.98999462180201,-3.84638326369218),.UNSPECIFIED.);
#947=B_SPLINE_CURVE_WITH_KNOTS('',3,(#42540,#42541,#42542,#42543,#42544,
#42545,#42546,#42547,#42548,#42549,#42550,#42551,#42552,#42553,#42554,#42555,
#42556,#42557,#42558,#42559,#42560,#42561),.UNSPECIFIED.,.F.,.F.,(4,3,3,
3,3,3,3,4),(7.59300756235149,7.97998924360401,8.97748789905451,9.97498655450502,
10.9724852099555,11.969983865406,12.9674825208565,13.8761928695311),
 .UNSPECIFIED.);
#948=B_SPLINE_CURVE_WITH_KNOTS('',3,(#42562,#42563,#42564,#42565,#42566,
#42567,#42568,#42569,#42570,#42571,#42572,#42573,#42574,#42575,#42576,#42577,
#42578,#42579,#42580,#42581,#42582,#42583,#42584,#42585,#42586,#42587,#42588,
#42589,#42590,#42591,#42592,#42593,#42594,#42595,#42596,#42597,#42598,#42599,
#42600,#42601,#42602,#42603,#42604,#42605,#42606,#42607,#42608,#42609,#42610,
#42611,#42612,#42613,#42614,#42615,#42616,#42617,#42618,#42619,#42620,#42621,
#42622,#42623,#42624,#42625,#42626,#42627,#42628,#42629,#42630,#42631,#42632,
#42633,#42634,#42635,#42636,#42637,#42638,#42639,#42640,#42641,#42642,#42643,
#42644,#42645,#42646),.UNSPECIFIED.,.F.,.F.,(4,3,3,3,3,3,3,3,3,3,3,3,3,
3,3,3,3,3,3,3,3,3,3,3,3,3,3,3,4),(0.,0.0219668112926134,0.0445443359559021,
0.0636200299333845,0.0720972303188465,0.0767552732140828,0.0810487403619284,
0.102995311125728,0.124771385304016,0.142866010921953,0.150422221343388,
0.15391641673982,0.157566439371711,0.178337031207171,0.197149887775761,
0.219420483792519,0.224320670513702,0.229403188138886,0.250068321572831,
0.270729057089704,0.285673880884443,0.296888224632328,0.300622176283363,
0.320394284144993,0.334296341483546,0.338763414131696,0.357788235774701,
0.37531465590982,0.37862159683149),.UNSPECIFIED.);
#949=B_SPLINE_CURVE_WITH_KNOTS('',3,(#42678,#42679,#42680,#42681,#42682,
#42683,#42684,#42685,#42686,#42687,#42688,#42689,#42690,#42691,#42692,#42693,
#42694),.UNSPECIFIED.,.F.,.F.,(4,1,1,1,1,1,1,1,1,1,1,1,1,1,4),(15.7079632679489,
15.7742466509132,16.264560774171,16.7548748974288,17.2451890206866,17.7355031439444,
18.2258172672022,18.71613139046,19.2064455137178,19.6967596369755,20.1870737602333,
20.6773878834911,21.1677020067489,21.6580161300067,21.9911485751285),
 .UNSPECIFIED.);
#950=B_SPLINE_CURVE_WITH_KNOTS('',3,(#42695,#42696,#42697,#42698,#42699,
#42700,#42701,#42702,#42703,#42704,#42705,#42706,#42707,#42708,#42709,#42710,
#42711),.UNSPECIFIED.,.F.,.F.,(4,1,1,1,1,1,1,1,1,1,1,1,1,1,4),(15.7079632679489,
15.8693424967452,16.359656620003,16.8499707432608,17.3402848665186,17.8305989897764,
18.3209131130342,18.811227236292,19.3015413595498,19.7918554828076,20.2821696060654,
20.7724837293232,21.2627978525809,21.7531119758387,21.9911485751285),
 .UNSPECIFIED.);
#951=B_SPLINE_CURVE_WITH_KNOTS('',3,(#43092,#43093,#43094,#43095,#43096,
#43097,#43098,#43099,#43100,#43101,#43102,#43103,#43104,#43105,#43106,#43107,
#43108,#43109,#43110,#43111,#43112,#43113,#43114,#43115,#43116,#43117,#43118,
#43119,#43120,#43121,#43122,#43123,#43124,#43125,#43126,#43127,#43128,#43129,
#43130,#43131,#43132,#43133,#43134,#43135,#43136,#43137,#43138,#43139,#43140,
#43141,#43142,#43143,#43144,#43145,#43146,#43147,#43148,#43149,#43150,#43151,
#43152,#43153,#43154,#43155,#43156,#43157,#43158,#43159,#43160,#43161,#43162,
#43163,#43164,#43165,#43166,#43167,#43168,#43169,#43170,#43171,#43172,#43173,
#43174,#43175,#43176,#43177,#43178,#43179,#43180,#43181,#43182,#43183,#43184,
#43185,#43186,#43187,#43188,#43189,#43190,#43191,#43192,#43193,#43194,#43195,
#43196,#43197,#43198,#43199,#43200,#43201,#43202,#43203,#43204,#43205,#43206),
 .UNSPECIFIED.,.F.,.F.,(4,3,3,3,3,3,3,3,3,3,3,3,3,3,3,3,3,3,3,3,3,3,3,3,
3,3,3,3,3,3,3,3,3,3,3,3,3,3,4),(0.,0.0505708571042727,0.101542673109873,
0.152182389706113,0.202219346658589,0.225638835489441,0.233898271119954,
0.240735485265272,0.290357617639612,0.295897301981998,0.345686264875582,
0.395413843633949,0.441706626966609,0.453063312881571,0.461070828559911,
0.467176391962776,0.515730570603939,0.563915442824477,0.580584976964589,
0.629137535103161,0.657230420337627,0.674238537119372,0.682110594253873,
0.688083279696401,0.735480735434175,0.782731786350779,0.829225244483419,
0.853880616978884,0.886547113898524,0.894686952978892,0.901806441759792,
0.948290089624541,0.990020715302407,1.01021978261714,1.02166124456445,1.02855221389401,
1.0738110712865,1.11521259233601,1.14791015664657),.UNSPECIFIED.);
#952=B_SPLINE_CURVE_WITH_KNOTS('',3,(#43207,#43208,#43209,#43210,#43211,
#43212,#43213,#43214,#43215,#43216,#43217,#43218,#43219,#43220,#43221,#43222,
#43223,#43224,#43225,#43226,#43227,#43228,#43229,#43230,#43231,#43232,#43233,
#43234,#43235,#43236,#43237,#43238,#43239,#43240,#43241,#43242,#43243,#43244,
#43245,#43246,#43247,#43248,#43249,#43250,#43251,#43252,#43253,#43254,#43255,
#43256,#43257,#43258,#43259,#43260,#43261,#43262,#43263,#43264,#43265,#43266,
#43267,#43268,#43269,#43270,#43271,#43272,#43273,#43274,#43275,#43276,#43277,
#43278,#43279,#43280,#43281,#43282,#43283,#43284,#43285,#43286,#43287,#43288,
#43289,#43290,#43291,#43292,#43293,#43294,#43295,#43296,#43297,#43298,#43299,
#43300,#43301,#43302,#43303,#43304,#43305,#43306,#43307,#43308,#43309,#43310,
#43311,#43312,#43313,#43314,#43315,#43316,#43317,#43318,#43319,#43320,#43321),
 .UNSPECIFIED.,.F.,.F.,(4,3,3,3,3,3,3,3,3,3,3,3,3,3,3,3,3,3,3,3,3,3,3,3,
3,3,3,3,3,3,3,3,3,3,3,3,3,3,4),(0.,0.0442982788118636,0.0893818690181126,
0.135122693119257,0.180798269742455,0.192189224643416,0.201490490453158,
0.207330447631488,0.254018913968702,0.259381740752703,0.305561249420596,
0.352304439716772,0.396784766685594,0.407417643265349,0.413596814657803,
0.419491730417116,0.467135890742667,0.515289047534096,0.53022574759206,
0.578093773825496,0.607379019530261,0.623354033228688,0.630969399843706,
0.637303510397527,0.686063011063978,0.735282487221379,0.784567458473146,
0.812375739463615,0.848989885401632,0.855830972691235,0.862937690127921,
0.912534157810533,0.960722845099838,0.982643323209691,0.993796749973554,
1.00410992606059,1.05516230274151,1.10528890696775,1.14369947197754),
 .UNSPECIFIED.);
#953=B_SPLINE_CURVE_WITH_KNOTS('',3,(#43322,#43323,#43324,#43325,#43326,
#43327,#43328,#43329,#43330,#43331,#43332,#43333,#43334,#43335,#43336,#43337,
#43338,#43339,#43340,#43341,#43342,#43343,#43344,#43345,#43346,#43347,#43348,
#43349,#43350,#43351,#43352,#43353,#43354,#43355,#43356,#43357,#43358,#43359,
#43360,#43361,#43362,#43363,#43364),.UNSPECIFIED.,.F.,.F.,(4,3,3,3,3,3,
3,3,3,3,3,3,3,3,4),(-10.1394149102777,-9.80628246515584,-9.31596834189804,
-8.82565421864025,-8.33534009538246,-7.84502597212467,-7.35471184886688,
-6.86439772560908,-6.37408360235129,-5.8837694790935,-5.39345535583571,
-4.90314123257792,-4.41282710932013,-3.92251298606233,-3.85622960309808),
 .UNSPECIFIED.);
#954=B_SPLINE_CURVE_WITH_KNOTS('',3,(#43745,#43746,#43747,#43748,#43749,
#43750,#43751,#43752,#43753,#43754,#43755,#43756,#43757,#43758,#43759,#43760,
#43761,#43762,#43763,#43764,#43765,#43766,#43767,#43768,#43769,#43770,#43771,
#43772,#43773,#43774,#43775,#43776,#43777,#43778,#43779,#43780,#43781,#43782,
#43783,#43784,#43785,#43786,#43787,#43788,#43789,#43790,#43791,#43792,#43793,
#43794,#43795,#43796,#43797,#43798,#43799,#43800,#43801,#43802,#43803,#43804,
#43805,#43806,#43807,#43808,#43809,#43810,#43811,#43812,#43813,#43814,#43815,
#43816,#43817,#43818,#43819,#43820,#43821,#43822,#43823,#43824,#43825,#43826,
#43827,#43828,#43829,#43830,#43831,#43832,#43833,#43834,#43835,#43836,#43837,
#43838,#43839,#43840,#43841,#43842,#43843,#43844,#43845,#43846,#43847,#43848,
#43849,#43850,#43851,#43852,#43853,#43854,#43855,#43856,#43857,#43858,#43859),
 .UNSPECIFIED.,.F.,.F.,(4,3,3,3,3,3,3,3,3,3,3,3,3,3,3,3,3,3,3,3,3,3,3,3,
3,3,3,3,3,3,3,3,3,3,3,3,3,3,4),(0.,0.04429834024652,0.089381979475409,0.135122817034445,
0.18079838316134,0.192189399543316,0.20149081189225,0.207330624426604,0.254019121588896,
0.259381740752706,0.305561208101797,0.352304372648012,0.396784716384027,
0.407417348322894,0.41359569479113,0.419491539259941,0.467135664198151,
0.515288809852319,0.530225747592073,0.578093783520646,0.607379028013523,
0.623354030000456,0.63096936113017,0.637303502944702,0.686063016433146,
0.735282499868879,0.784567472007001,0.812375739463663,0.848989885401685,
0.85583097269828,0.862937690097506,0.912534156610552,0.960722844199872,
0.982643321680792,0.993796738994502,1.00410992500793,1.0551623020005,1.10528890696783,
1.14369947197762),.UNSPECIFIED.);
#955=B_SPLINE_CURVE_WITH_KNOTS('',3,(#43860,#43861,#43862,#43863,#43864,
#43865,#43866,#43867,#43868,#43869,#43870,#43871,#43872,#43873,#43874,#43875,
#43876,#43877,#43878,#43879,#43880,#43881,#43882,#43883,#43884,#43885,#43886,
#43887,#43888,#43889,#43890,#43891,#43892,#43893,#43894,#43895,#43896,#43897,
#43898,#43899,#43900,#43901,#43902),.UNSPECIFIED.,.F.,.F.,(4,3,3,3,3,3,
3,3,3,3,3,3,3,3,4),(7.59274844815668,7.84502597212467,8.33534009538246,
8.82565421864025,9.31596834189804,9.80628246515583,10.2965965884136,10.7869107116714,
11.2772248349292,11.767538958187,12.2578530814448,12.7481672047026,13.2384813279604,
13.7287954512182,13.8759337553363),.UNSPECIFIED.);
#956=B_SPLINE_CURVE_WITH_KNOTS('',3,(#43903,#43904,#43905,#43906,#43907,
#43908,#43909,#43910,#43911,#43912,#43913,#43914,#43915,#43916,#43917,#43918,
#43919,#43920,#43921,#43922,#43923,#43924,#43925,#43926,#43927,#43928,#43929,
#43930,#43931,#43932,#43933,#43934,#43935,#43936,#43937,#43938,#43939,#43940,
#43941,#43942,#43943,#43944,#43945,#43946,#43947,#43948,#43949,#43950,#43951,
#43952,#43953,#43954,#43955,#43956,#43957,#43958,#43959,#43960,#43961,#43962,
#43963,#43964,#43965,#43966,#43967,#43968,#43969,#43970,#43971,#43972,#43973,
#43974,#43975,#43976,#43977,#43978,#43979,#43980,#43981,#43982,#43983,#43984,
#43985,#43986,#43987,#43988,#43989,#43990,#43991,#43992,#43993,#43994,#43995,
#43996,#43997,#43998,#43999,#44000,#44001,#44002,#44003,#44004,#44005,#44006,
#44007,#44008,#44009,#44010,#44011,#44012,#44013,#44014,#44015,#44016,#44017),
 .UNSPECIFIED.,.F.,.F.,(4,3,3,3,3,3,3,3,3,3,3,3,3,3,3,3,3,3,3,3,3,3,3,3,
3,3,3,3,3,3,3,3,3,3,3,3,3,3,4),(0.,0.05057089589372,0.101542722275973,0.152182412916207,
0.202219333720841,0.225638825786133,0.233898233275305,0.24073547777789,
0.290357594353021,0.295897301982008,0.345686254294586,0.395413835081348,
0.44170662055217,0.453063297205788,0.461070756512692,0.467176281050606,
0.515730458090084,0.56391533759721,0.580584976964637,0.629137535716166,
0.657230420874013,0.674238539358194,0.682110620359464,0.688083286117201,
0.735480742780762,0.782731794499091,0.829225256981287,0.85388061697894,
0.886547113898585,0.894686952580864,0.901806441637606,0.948290090133573,
0.990020715684203,1.0102197832758,1.02166123242085,1.02855218820189,1.07381104284631,
1.11521259233609,1.14791015664666),.UNSPECIFIED.);
#957=B_SPLINE_CURVE_WITH_KNOTS('',3,(#44085,#44086,#44087,#44088),
 .UNSPECIFIED.,.F.,.F.,(4,4),(114.40689867021,115.114280422261),
 .UNSPECIFIED.);
#958=B_SPLINE_CURVE_WITH_KNOTS('',3,(#44093,#44094,#44095,#44096,#44097,
#44098,#44099,#44100,#44101,#44102),.UNSPECIFIED.,.F.,.F.,(4,3,3,4),(-113.097335529233,
-112.13125696422,-111.136915811539,-110.663124627694),.UNSPECIFIED.);
#959=B_SPLINE_CURVE_WITH_KNOTS('',3,(#44107,#44108,#44109,#44110,#44111,
#44112,#44113,#44114,#44115,#44116,#44117,#44118,#44119,#44120,#44121,#44122,
#44123,#44124,#44125,#44126,#44127,#44128,#44129,#44130,#44131),
 .UNSPECIFIED.,.F.,.F.,(4,3,3,3,3,3,3,3,4),(108.12371336303,108.173779859754,
109.165279940112,110.15678002047,111.148280100828,112.139780181187,113.131280261545,
114.122780341903,114.40689867021),.UNSPECIFIED.);
#960=B_SPLINE_CURVE_WITH_KNOTS('',3,(#44132,#44133,#44134,#44135,#44136,
#44137,#44138,#44139,#44140,#44141,#44142,#44143,#44144,#44145,#44146,#44147,
#44148,#44149,#44150,#44151,#44152,#44153),.UNSPECIFIED.,.F.,.F.,(4,3,3,
3,3,3,3,4),(-110.663124627694,-110.142574658859,-109.148233506178,-108.153892353498,
-107.159551200817,-106.165210048137,-105.170868895457,-104.379939320515),
 .UNSPECIFIED.);
#961=B_SPLINE_CURVE_WITH_KNOTS('',3,(#44158,#44159,#44160,#44161,#44162,
#44163,#44164,#44165,#44166,#44167,#44168,#44169,#44170,#44171,#44172,#44173,
#44174,#44175,#44176,#44177,#44178,#44179),.UNSPECIFIED.,.F.,.F.,(4,3,3,
3,3,3,3,4),(101.84052805585,102.224779377605,103.216279457963,104.207779538322,
105.19927961868,106.190779699038,107.182279779396,108.12371336303),
 .UNSPECIFIED.);
#962=B_SPLINE_CURVE_WITH_KNOTS('',3,(#44180,#44181,#44182,#44183,#44184,
#44185,#44186,#44187,#44188,#44189,#44190,#44191,#44192,#44193,#44194,#44195,
#44196,#44197,#44198,#44199,#44200,#44201,#44202,#44203,#44204),
 .UNSPECIFIED.,.F.,.F.,(4,3,3,3,3,3,3,3,4),(-104.379939320515,-104.176527742776,
-103.182186590096,-102.187845437415,-101.193504284735,-100.199163132054,
-99.204821979374,-98.2104808266935,-98.096754013335),.UNSPECIFIED.);
#963=B_SPLINE_CURVE_WITH_KNOTS('',3,(#44209,#44210,#44211,#44212,#44213,
#44214,#44215,#44216,#44217,#44218,#44219,#44220,#44221,#44222,#44223,#44224,
#44225,#44226,#44227,#44228,#44229,#44230),.UNSPECIFIED.,.F.,.F.,(4,3,3,
3,3,3,3,4),(95.5573427486709,96.2757788954565,97.2672789758147,98.2587790561728,
99.2502791365309,100.241779216889,101.233279297247,101.84052805585),
 .UNSPECIFIED.);
#964=B_SPLINE_CURVE_WITH_KNOTS('',3,(#44231,#44232,#44233,#44234,#44235,
#44236,#44237,#44238,#44239,#44240,#44241,#44242,#44243,#44244,#44245,#44246,
#44247,#44248,#44249,#44250,#44251,#44252),.UNSPECIFIED.,.F.,.F.,(4,3,3,
3,3,3,3,4),(-98.096754013335,-97.2161396740131,-96.2217985213327,-95.2274573686523,
-94.2331162159718,-93.2387750632914,-92.2444339106109,-91.8135687061554),
 .UNSPECIFIED.);
#965=B_SPLINE_CURVE_WITH_KNOTS('',3,(#44257,#44258,#44259,#44260,#44261,
#44262,#44263,#44264,#44265,#44266,#44267,#44268,#44269,#44270,#44271,#44272,
#44273,#44274,#44275,#44276,#44277,#44278,#44279,#44280,#44281),
 .UNSPECIFIED.,.F.,.F.,(4,3,3,3,3,3,3,3,4),(89.2741574414913,89.3352783329496,
90.3267784133077,91.3182784936659,92.309778574024,93.3012786543821,94.2927787347403,
95.2842788150984,95.5573427486709),.UNSPECIFIED.);
#966=B_SPLINE_CURVE_WITH_KNOTS('',3,(#44282,#44283,#44284,#44285,#44286,
#44287,#44288,#44289,#44290,#44291,#44292,#44293,#44294,#44295,#44296,#44297,
#44298,#44299,#44300,#44301,#44302,#44303),.UNSPECIFIED.,.F.,.F.,(4,3,3,
3,3,3,3,4),(-91.8135687061554,-91.2500927579305,-90.2557516052501,-89.2614104525696,
-88.2670692998892,-87.2727281472088,-86.2783869945283,-85.5303833989758),
 .UNSPECIFIED.);
#967=B_SPLINE_CURVE_WITH_KNOTS('',3,(#44308,#44309,#44310,#44311,#44312,
#44313,#44314,#44315,#44316,#44317,#44318,#44319,#44320,#44321,#44322,#44323,
#44324,#44325,#44326,#44327,#44328,#44329),.UNSPECIFIED.,.F.,.F.,(4,3,3,
3,3,3,3,4),(82.9909721343117,83.3862778508009,84.377777931159,85.3692780115171,
86.3607780918753,87.3522781722334,88.3437782525915,89.2741574414913),
 .UNSPECIFIED.);
#968=B_SPLINE_CURVE_WITH_KNOTS('',3,(#44330,#44331,#44332,#44333,#44334,
#44335,#44336,#44337,#44338,#44339,#44340,#44341,#44342,#44343,#44344,#44345,
#44346,#44347,#44348,#44349,#44350,#44351,#44352,#44353,#44354),
 .UNSPECIFIED.,.F.,.F.,(4,3,3,3,3,3,3,3,4),(-85.5303833989758,-85.2840458418479,
-84.2897046891674,-83.295363536487,-82.3010223838066,-81.3066812311261,
-80.3123400784457,-79.3179989257652,-79.2471980917962),.UNSPECIFIED.);
#969=B_SPLINE_CURVE_WITH_KNOTS('',3,(#44359,#44360,#44361,#44362,#44363,
#44364,#44365,#44366,#44367,#44368,#44369,#44370,#44371,#44372,#44373,#44374,
#44375,#44376,#44377,#44378,#44379,#44380),.UNSPECIFIED.,.F.,.F.,(4,3,3,
3,3,3,3,4),(76.7077868271321,77.4372773686521,78.4287774490102,79.4202775293683,
80.4117776097265,81.4032776900846,82.3947777704427,82.9909721343117),
 .UNSPECIFIED.);
#970=B_SPLINE_CURVE_WITH_KNOTS('',3,(#44381,#44382,#44383,#44384,#44385,
#44386,#44387,#44388,#44389,#44390,#44391,#44392,#44393,#44394,#44395,#44396,
#44397,#44398,#44399,#44400,#44401,#44402),.UNSPECIFIED.,.F.,.F.,(4,3,3,
3,3,3,3,4),(-79.2471980917962,-78.3236577730848,-77.3293166204044,-76.3349754677239,
-75.3406343150435,-74.3462931623631,-73.3519520096826,-72.9640127846166),
 .UNSPECIFIED.);
#971=B_SPLINE_CURVE_WITH_KNOTS('',3,(#44407,#44408,#44409,#44410,#44411,
#44412,#44413,#44414,#44415,#44416,#44417,#44418,#44419,#44420,#44421,#44422,
#44423,#44424,#44425,#44426,#44427,#44428,#44429,#44430,#44431),
 .UNSPECIFIED.,.F.,.F.,(4,3,3,3,3,3,3,3,4),(70.4246015199525,70.4967768061452,
71.4882768865033,72.4797769668614,73.4712770472196,74.4627771275777,75.4542772079358,
76.445777288294,76.7077868271321),.UNSPECIFIED.);
#972=B_SPLINE_CURVE_WITH_KNOTS('',3,(#44432,#44433,#44434,#44435,#44436,
#44437,#44438,#44439,#44440,#44441,#44442,#44443,#44444,#44445,#44446,#44447,
#44448,#44449,#44450,#44451,#44452,#44453),.UNSPECIFIED.,.F.,.F.,(4,3,3,
3,3,3,3,4),(-72.9640127846166,-72.3576108570022,-71.3632697043217,-70.3689285516413,
-69.3745873989609,-68.3802462462804,-67.3859050936,-66.680827477437),
 .UNSPECIFIED.);
#973=B_SPLINE_CURVE_WITH_KNOTS('',3,(#44458,#44459,#44460,#44461,#44462,
#44463,#44464,#44465,#44466,#44467,#44468,#44469,#44470,#44471,#44472,#44473,
#44474,#44475,#44476,#44477,#44478,#44479),.UNSPECIFIED.,.F.,.F.,(4,3,3,
3,3,3,3,4),(64.1414162127729,64.5477763239964,65.5392764043545,66.5307764847127,
67.5222765650708,68.5137766454289,69.5052767257871,70.4246015199525),
 .UNSPECIFIED.);
#974=B_SPLINE_CURVE_WITH_KNOTS('',3,(#44480,#44481,#44482,#44483,#44484,
#44485,#44486,#44487,#44488,#44489,#44490,#44491,#44492,#44493,#44494,#44495,
#44496,#44497,#44498,#44499,#44500,#44501,#44502,#44503,#44504),
 .UNSPECIFIED.,.F.,.F.,(4,3,3,3,3,3,3,3,4),(-66.680827477437,-66.3915639409195,
-65.3972227882391,-64.4028816355587,-63.4085404828782,-62.4141993301978,
-61.4198581775174,-60.4255170248369,-60.3976421702574),.UNSPECIFIED.);
#975=B_SPLINE_CURVE_WITH_KNOTS('',3,(#44509,#44510,#44511,#44512,#44513,
#44514,#44515,#44516,#44517,#44518,#44519,#44520,#44521,#44522,#44523,#44524,
#44525,#44526,#44527,#44528,#44529,#44530),.UNSPECIFIED.,.F.,.F.,(4,3,3,
3,3,3,3,4),(57.8582309055933,58.5987758418476,59.5902759222058,60.5817760025639,
61.573276082922,62.5647761632802,63.5562762436383,64.1414162127729),
 .UNSPECIFIED.);
#976=B_SPLINE_CURVE_WITH_KNOTS('',3,(#44531,#44532,#44533,#44534,#44535,
#44536,#44537,#44538,#44539,#44540,#44541,#44542,#44543,#44544,#44545,#44546,
#44547,#44548,#44549,#44550,#44551,#44552),.UNSPECIFIED.,.F.,.F.,(4,3,3,
3,3,3,3,4),(-60.3976421702574,-59.4311758721565,-58.4368347194761,-57.4424935667956,
-56.4481524141152,-55.4538112614347,-54.4594701087543,-54.1144568630778),
 .UNSPECIFIED.);
#977=B_SPLINE_CURVE_WITH_KNOTS('',3,(#44557,#44558,#44559,#44560,#44561,
#44562,#44563,#44564,#44565,#44566,#44567,#44568,#44569,#44570,#44571,#44572,
#44573,#44574,#44575,#44576,#44577,#44578,#44579,#44580,#44581),
 .UNSPECIFIED.,.F.,.F.,(4,3,3,3,3,3,3,3,4),(51.5750455984137,51.6582752793407,
52.6497753596989,53.641275440057,54.6327755204151,55.6242756007733,56.6157756811314,
57.6072757614895,57.8582309055933),.UNSPECIFIED.);
#978=B_SPLINE_CURVE_WITH_KNOTS('',3,(#44582,#44583,#44584,#44585,#44586,
#44587,#44588,#44589,#44590,#44591,#44592,#44593,#44594,#44595,#44596,#44597,
#44598,#44599,#44600,#44601,#44602,#44603),.UNSPECIFIED.,.F.,.F.,(4,3,3,
3,3,3,3,4),(-54.1144568630778,-53.4651289560739,-52.4707878033934,-51.476446650713,
-50.4821054980325,-49.4877643453521,-48.4934231926717,-47.8312715558982),
 .UNSPECIFIED.);
#979=B_SPLINE_CURVE_WITH_KNOTS('',3,(#44608,#44609,#44610,#44611,#44612,
#44613,#44614,#44615,#44616,#44617,#44618,#44619,#44620,#44621,#44622,#44623,
#44624,#44625,#44626,#44627,#44628,#44629),.UNSPECIFIED.,.F.,.F.,(4,3,3,
3,3,3,3,4),(45.2918602912341,45.709274797192,46.7007748775501,47.6922749579082,
48.6837750382664,49.6752751186245,50.6667751989826,51.5750455984137),
 .UNSPECIFIED.);
#980=B_SPLINE_CURVE_WITH_KNOTS('',3,(#44630,#44631,#44632,#44633,#44634,
#44635,#44636,#44637,#44638,#44639,#44640,#44641,#44642,#44643,#44644,#44645,
#44646,#44647,#44648,#44649,#44650,#44651),.UNSPECIFIED.,.F.,.F.,(4,3,3,
3,3,3,3,4),(-47.8312715558982,-47.4990820399912,-46.5047408873108,-45.5103997346304,
-44.5160585819499,-43.5217174292695,-42.5273762765891,-41.5480862487186),
 .UNSPECIFIED.);
#981=B_SPLINE_CURVE_WITH_KNOTS('',3,(#44656,#44657,#44658,#44659,#44660,
#44661,#44662,#44663,#44664,#44665,#44666,#44667,#44668,#44669,#44670,#44671,
#44672,#44673,#44674,#44675,#44676,#44677),.UNSPECIFIED.,.F.,.F.,(4,3,3,
3,3,3,3,4),(39.0086749840545,39.7602743150432,40.7517743954013,41.7432744757595,
42.7347745561176,43.7262746364757,44.7177747168338,45.2918602912341),
 .UNSPECIFIED.);
#982=B_SPLINE_CURVE_WITH_KNOTS('',3,(#44678,#44679,#44680,#44681,#44682,
#44683,#44684,#44685,#44686,#44687,#44688,#44689,#44690,#44691,#44692,#44693,
#44694,#44695,#44696,#44697,#44698,#44699,#44700,#44701,#44702),
 .UNSPECIFIED.,.F.,.F.,(4,3,3,3,3,3,3,3,4),(-41.5480862487186,-41.5330351239086,
-40.5386939712282,-39.5443528185478,-38.5500116658673,-37.5556705131869,
-36.5613293605064,-35.566988207826,-35.264900941539),.UNSPECIFIED.);
#983=B_SPLINE_CURVE_WITH_KNOTS('',3,(#44707,#44708,#44709,#44710,#44711,
#44712,#44713,#44714,#44715,#44716,#44717,#44718,#44719,#44720,#44721,#44722,
#44723,#44724,#44725,#44726,#44727,#44728,#44729,#44730,#44731),
 .UNSPECIFIED.,.F.,.F.,(4,3,3,3,3,3,3,3,4),(32.725489676875,32.8197737525363,
33.8112738328944,34.8027739132525,35.7942739936107,36.7857740739688,37.7772741543269,
38.7687742346851,39.0086749840545),.UNSPECIFIED.);
#984=B_SPLINE_CURVE_WITH_KNOTS('',3,(#44732,#44733,#44734,#44735,#44736,
#44737,#44738,#44739,#44740,#44741,#44742,#44743,#44744,#44745,#44746,#44747,
#44748,#44749,#44750,#44751,#44752,#44753),.UNSPECIFIED.,.F.,.F.,(4,3,3,
3,3,3,3,4),(-35.264900941539,-34.5726470551456,-33.5783059024651,-32.5839647497847,
-31.5896235971042,-30.5952824444238,-29.6009412917434,-28.9817156343595),
 .UNSPECIFIED.);
#985=B_SPLINE_CURVE_WITH_KNOTS('',3,(#44758,#44759,#44760,#44761,#44762,
#44763,#44764,#44765,#44766,#44767,#44768,#44769,#44770,#44771,#44772,#44773,
#44774,#44775,#44776,#44777,#44778,#44779),.UNSPECIFIED.,.F.,.F.,(4,3,3,
3,3,3,3,4),(26.4423043696954,26.8707732703875,27.8622733507456,28.8537734311038,
29.8452735114619,30.83677359182,31.8282736721782,32.725489676875),
 .UNSPECIFIED.);
#986=B_SPLINE_CURVE_WITH_KNOTS('',3,(#44780,#44781,#44782,#44783,#44784,
#44785,#44786,#44787,#44788,#44789,#44790,#44791,#44792,#44793,#44794,#44795,
#44796,#44797,#44798,#44799,#44800,#44801),.UNSPECIFIED.,.F.,.F.,(4,3,3,
3,3,3,3,4),(-28.9817156343595,-28.6066001390629,-27.6122589863825,-26.6179178337021,
-25.6235766810216,-24.6292355283412,-23.6348943756607,-22.6985303271799),
 .UNSPECIFIED.);
#987=B_SPLINE_CURVE_WITH_KNOTS('',3,(#44806,#44807,#44808,#44809,#44810,
#44811,#44812,#44813,#44814,#44815,#44816,#44817,#44818,#44819,#44820,#44821,
#44822,#44823,#44824,#44825,#44826,#44827),.UNSPECIFIED.,.F.,.F.,(4,3,3,
3,3,3,3,4),(20.1591190625158,20.9217727882387,21.9132728685969,22.904772948955,
23.8962730293131,24.8877731096713,25.8792731900294,26.4423043696954),
 .UNSPECIFIED.);
#988=B_SPLINE_CURVE_WITH_KNOTS('',3,(#44828,#44829,#44830,#44831,#44832,
#44833,#44834,#44835,#44836,#44837,#44838,#44839,#44840,#44841,#44842,#44843,
#44844,#44845,#44846,#44847,#44848,#44849,#44850,#44851,#44852),
 .UNSPECIFIED.,.F.,.F.,(4,3,3,3,3,3,3,3,4),(-22.6985303271799,-22.6405532229803,
-21.6462120702999,-20.6518709176194,-19.657529764939,-18.6631886122585,
-17.6688474595781,-16.6745063068977,-16.4153450200003),.UNSPECIFIED.);
#989=B_SPLINE_CURVE_WITH_KNOTS('',3,(#44857,#44858,#44859,#44860,#44861,
#44862,#44863,#44864,#44865,#44866,#44867,#44868,#44869,#44870,#44871,#44872,
#44873,#44874,#44875,#44876,#44877,#44878,#44879,#44880,#44881),
 .UNSPECIFIED.,.F.,.F.,(4,3,3,3,3,3,3,3,4),(13.8759337553362,13.9812722257318,
14.97277230609,15.9642723864481,16.9557724668062,17.9472725471644,18.9387726275225,
19.9302727078806,20.1591190625158),.UNSPECIFIED.);
#990=B_SPLINE_CURVE_WITH_KNOTS('',3,(#44882,#44883,#44884,#44885,#44886,
#44887,#44888,#44889,#44890,#44891,#44892,#44893,#44894,#44895,#44896,#44897,
#44898,#44899,#44900,#44901,#44902,#44903),.UNSPECIFIED.,.F.,.F.,(4,3,3,
3,3,3,3,4),(-16.4153450200003,-15.6801651542172,-14.6858240015368,-13.6914828488564,
-12.6971416961759,-11.7028005434955,-10.708459390815,-10.1321597128207),
 .UNSPECIFIED.);
#991=B_SPLINE_CURVE_WITH_KNOTS('',3,(#44909,#44910,#44911,#44912,#44913,
#44914,#44915,#44916,#44917,#44918,#44919,#44920,#44921),.UNSPECIFIED.,
 .F.,.F.,(4,3,3,3,4),(-3.84897440564112,-3.74807132205199,-2.75373016937155,
-1.75938901669111,-0.765047864010683),.UNSPECIFIED.);
#992=B_SPLINE_CURVE_WITH_KNOTS('',3,(#44923,#44924,#44925,#44926,#44927,
#44928,#44929,#44930,#44931,#44932,#44933,#44934,#44935,#44936,#44937,#44938),
 .UNSPECIFIED.,.F.,.F.,(4,2,2,2,2,2,2,4),(0.232635770676731,0.284684236160853,
0.379578792383291,0.47447334860573,0.569367904828168,0.664262744797375,
0.759157584766583,0.773538308589687),.UNSPECIFIED.);
#993=B_SPLINE_CURVE_WITH_KNOTS('',3,(#44939,#44940,#44941,#44942,#44943,
#44944,#44945,#44946,#44947,#44948,#44949,#44950,#44951,#44952,#44953,#44954,
#44955,#44956,#44957),.UNSPECIFIED.,.F.,.F.,(4,3,3,3,3,3,4),(2.26925352322945,
3.07477134179243,4.06627142215055,5.05777150250868,6.04927158286681,7.04077166322494,
7.59274844815659),.UNSPECIFIED.);
#994=B_SPLINE_CURVE_WITH_KNOTS('',3,(#44963,#44964,#44965,#44966,#44967,
#44968,#44969,#44970),.UNSPECIFIED.,.F.,.F.,(4,1,1,1,1,4),(122.522113490002,
122.995904673847,123.990245826527,124.984586979208,125.978928131888,126.973269284569),
 .UNSPECIFIED.);
#995=B_SPLINE_CURVE_WITH_KNOTS('',3,(#44975,#44976,#44977,#44978,#44979,
#44980,#44981,#44982,#44983),.UNSPECIFIED.,.F.,.F.,(4,1,1,1,1,1,4),(122.522113490002,
122.572179986726,123.563680067084,124.555180147442,125.5466802278,126.538180308158,
127.495735656204),.UNSPECIFIED.);
#996=B_SPLINE_CURVE_WITH_KNOTS('',3,(#44988,#44989,#44990,#44991,#44992,
#44993,#44994,#44995,#44996,#44997),.UNSPECIFIED.,.F.,.F.,(4,1,1,1,1,1,
1,4),(116.238928182822,117.029857757764,118.024198910445,119.018540063125,
120.012881215806,121.007222368486,122.001563521167,122.522113490002),
 .UNSPECIFIED.);
#997=B_SPLINE_CURVE_WITH_KNOTS('',3,(#44998,#44999,#45000,#45001,#45002,
#45003,#45004,#45005,#45006,#45007),.UNSPECIFIED.,.F.,.F.,(4,1,1,1,1,1,
1,4),(116.238928182822,116.623179504577,117.614679584935,118.606179665293,
119.597679745651,120.58917982601,121.580679906368,122.522113490002),
 .UNSPECIFIED.);
#998=B_SPLINE_CURVE_WITH_KNOTS('',3,(#45012,#45013,#45014,#45015,#45016,
#45017,#45018,#45019,#45020,#45021,#45022),.UNSPECIFIED.,.F.,.F.,(4,1,1,
1,1,1,1,1,4),(109.955742875643,110.069469689001,111.063810841682,112.058151994362,
113.052493147043,114.046834299723,115.041175452403,116.035516605084,116.238928182822),
 .UNSPECIFIED.);
#999=B_SPLINE_CURVE_WITH_KNOTS('',3,(#45023,#45024,#45025,#45026,#45027,
#45028,#45029,#45030,#45031,#45032),.UNSPECIFIED.,.F.,.F.,(4,1,1,1,1,1,
1,4),(109.955742875643,110.674179022428,111.665679102786,112.657179183145,
113.648679263503,114.640179343861,115.631679424219,116.238928182822),
 .UNSPECIFIED.);
#1000=B_SPLINE_CURVE_WITH_KNOTS('',3,(#45037,#45038,#45039,#45040,#45041,
#45042,#45043,#45044,#45045,#45046),.UNSPECIFIED.,.F.,.F.,(4,1,1,1,1,1,
1,4),(103.672557568463,104.103422772919,105.097763925599,106.09210507828,
107.08644623096,108.08078738364,109.075128536321,109.955742875643),
 .UNSPECIFIED.);
#1001=B_SPLINE_CURVE_WITH_KNOTS('',3,(#45047,#45048,#45049,#45050,#45051,
#45052,#45053,#45054,#45055,#45056,#45057),.UNSPECIFIED.,.F.,.F.,(4,1,1,
1,1,1,1,1,4),(103.672557568463,103.733678459921,104.72517854028,105.716678620638,
106.708178700996,107.699678781354,108.691178861712,109.68267894207,109.955742875643),
 .UNSPECIFIED.);
#1002=B_SPLINE_CURVE_WITH_KNOTS('',3,(#45062,#45063,#45064,#45065,#45066,
#45067,#45068,#45069,#45070,#45071),.UNSPECIFIED.,.F.,.F.,(4,1,1,1,1,1,
1,4),(97.3893722612835,98.137375856836,99.1317170095165,100.126058162197,
101.120399314877,102.114740467558,103.109081620238,103.672557568463),
 .UNSPECIFIED.);
#1003=B_SPLINE_CURVE_WITH_KNOTS('',3,(#45072,#45073,#45074,#45075,#45076,
#45077,#45078,#45079,#45080,#45081),.UNSPECIFIED.,.F.,.F.,(4,1,1,1,1,1,
1,4),(97.3893722612835,97.7846779777726,98.7761780581307,99.7676781384889,
100.759178218847,101.750678299205,102.742178379563,103.672557568463),
 .UNSPECIFIED.);
#1004=B_SPLINE_CURVE_WITH_KNOTS('',3,(#45086,#45087,#45088,#45089,#45090,
#45091,#45092,#45093,#45094,#45095,#45096),.UNSPECIFIED.,.F.,.F.,(4,1,1,
1,1,1,1,1,4),(91.1061869541039,91.176987788073,92.1713289407534,93.1656700934338,
94.1600112461143,95.1543523987947,96.1486935514752,97.1430347041556,97.3893722612835),
 .UNSPECIFIED.);
#1005=B_SPLINE_CURVE_WITH_KNOTS('',3,(#45097,#45098,#45099,#45100,#45101,
#45102,#45103,#45104,#45105,#45106),.UNSPECIFIED.,.F.,.F.,(4,1,1,1,1,1,
1,4),(91.1061869541039,91.8356774956238,92.827177575982,93.8186776563401,
94.8101777366982,95.8016778170563,96.7931778974145,97.3893722612835),
 .UNSPECIFIED.);
#1006=B_SPLINE_CURVE_WITH_KNOTS('',3,(#45111,#45112,#45113,#45114,#45115,
#45116,#45117,#45118,#45119,#45120),.UNSPECIFIED.,.F.,.F.,(4,1,1,1,1,1,
1,4),(84.8230016469244,85.2109408719903,86.2052820246708,87.1996231773512,
88.1939643300317,89.1883054827121,90.1826466353925,91.1061869541039),
 .UNSPECIFIED.);
#1007=B_SPLINE_CURVE_WITH_KNOTS('',3,(#45121,#45122,#45123,#45124,#45125,
#45126,#45127,#45128,#45129,#45130,#45131),.UNSPECIFIED.,.F.,.F.,(4,1,1,
1,1,1,1,1,4),(84.8230016469244,84.8951769331169,85.8866770134751,86.8781770938332,
87.8696771741913,88.8611772545494,89.8526773349076,90.8441774152657,91.1061869541039),
 .UNSPECIFIED.);
#1008=B_SPLINE_CURVE_WITH_KNOTS('',3,(#45136,#45137,#45138,#45139,#45140,
#45141,#45142,#45143,#45144,#45145),.UNSPECIFIED.,.F.,.F.,(4,1,1,1,1,1,
1,4),(78.5398163397448,79.2448939559077,80.2392351085882,81.2335762612686,
82.227917413949,83.2222585666295,84.2165997193099,84.8230016469244),
 .UNSPECIFIED.);
#1009=B_SPLINE_CURVE_WITH_KNOTS('',3,(#45146,#45147,#45148,#45149,#45150,
#45151,#45152,#45153,#45154,#45155),.UNSPECIFIED.,.F.,.F.,(4,1,1,1,1,1,
1,4),(78.5398163397448,78.9461764509682,79.9376765313263,80.9291766116844,
81.9206766920425,82.9121767724007,83.9036768527588,84.8230016469244),
 .UNSPECIFIED.);
#1010=B_SPLINE_CURVE_WITH_KNOTS('',3,(#45160,#45161,#45162,#45163,#45164,
#45165,#45166,#45167,#45168,#45169,#45170),.UNSPECIFIED.,.F.,.F.,(4,1,1,
1,1,1,1,1,4),(72.2566310325652,72.2845058871447,73.2788470398251,74.2731881925055,
75.267529345186,76.2618704978664,77.2562116505468,78.2505528032273,78.5398163397448),
 .UNSPECIFIED.);
#1011=B_SPLINE_CURVE_WITH_KNOTS('',3,(#45171,#45172,#45173,#45174,#45175,
#45176,#45177,#45178,#45179,#45180),.UNSPECIFIED.,.F.,.F.,(4,1,1,1,1,1,
1,4),(72.2566310325652,72.9971759688194,73.9886760491775,74.9801761295356,
75.9716762098938,76.9631762902519,77.95467637061,78.5398163397448),
 .UNSPECIFIED.);
#1012=B_SPLINE_CURVE_WITH_KNOTS('',3,(#45185,#45186,#45187,#45188,#45189,
#45190,#45191,#45192,#45193,#45194),.UNSPECIFIED.,.F.,.F.,(4,1,1,1,1,1,
1,4),(65.9734457253856,66.318458971062,67.3128001237425,68.3071412764229,
69.3014824291033,70.2958235817838,71.2901647344642,72.2566310325652),
 .UNSPECIFIED.);
#1013=B_SPLINE_CURVE_WITH_KNOTS('',3,(#45195,#45196,#45197,#45198,#45199,
#45200,#45201,#45202,#45203,#45204,#45205),.UNSPECIFIED.,.F.,.F.,(4,1,1,
1,1,1,1,1,4),(65.9734457253856,66.0566754063125,67.0481754866706,68.0396755670287,
69.0311756473869,70.022675727745,71.0141758081031,72.0056758884613,72.2566310325652),
 .UNSPECIFIED.);
#1014=B_SPLINE_CURVE_WITH_KNOTS('',3,(#45210,#45211,#45212,#45213,#45214,
#45215,#45216,#45217,#45218,#45219),.UNSPECIFIED.,.F.,.F.,(4,1,1,1,1,1,
1,4),(59.690260418206,60.3524120549794,61.3467532076598,62.3410943603403,
63.3354355130207,64.3297766657012,65.3241178183816,65.9734457253856),
 .UNSPECIFIED.);
#1015=B_SPLINE_CURVE_WITH_KNOTS('',3,(#45220,#45221,#45222,#45223,#45224,
#45225,#45226,#45227,#45228,#45229),.UNSPECIFIED.,.F.,.F.,(4,1,1,1,1,1,
1,4),(59.690260418206,60.1076749241637,61.0991750045218,62.09067508488,
63.0821751652381,64.0736752455962,65.0651753259544,65.9734457253856),
 .UNSPECIFIED.);
#1016=B_SPLINE_CURVE_WITH_KNOTS('',3,(#45234,#45235,#45236,#45237,#45238,
#45239,#45240,#45241,#45242,#45243),.UNSPECIFIED.,.F.,.F.,(4,1,1,1,1,1,
1,4),(53.4070751110264,54.3863651388968,55.3807062915772,56.3750474442577,
57.3693885969381,58.3637297496185,59.358070902299,59.690260418206),
 .UNSPECIFIED.);
#1017=B_SPLINE_CURVE_WITH_KNOTS('',3,(#45244,#45245,#45246,#45247,#45248,
#45249,#45250,#45251,#45252,#45253),.UNSPECIFIED.,.F.,.F.,(4,1,1,1,1,1,
1,4),(53.4070751110264,54.1586744420149,55.1501745223731,56.1416746027312,
57.1331746830893,58.1246747634475,59.1161748438056,59.690260418206),
 .UNSPECIFIED.);
#1018=B_SPLINE_CURVE_WITH_KNOTS('',3,(#45258,#45259,#45260,#45261,#45262,
#45263,#45264,#45265,#45266,#45267,#45268),.UNSPECIFIED.,.F.,.F.,(4,1,1,
1,1,1,1,1,4),(47.1238898038468,47.4259770701337,48.4203182228142,49.4146593754946,
50.409000528175,51.4033416808555,52.3976828335359,53.3920239862163,53.4070751110264),
 .UNSPECIFIED.);
#1019=B_SPLINE_CURVE_WITH_KNOTS('',3,(#45269,#45270,#45271,#45272,#45273,
#45274,#45275,#45276,#45277,#45278,#45279),.UNSPECIFIED.,.F.,.F.,(4,1,1,
1,1,1,1,1,4),(47.1238898038468,47.218173879508,48.2096739598662,49.2011740402243,
50.1926741205824,51.1841742009405,52.1756742812987,53.1671743616568,53.4070751110264),
 .UNSPECIFIED.);
#1020=B_SPLINE_CURVE_WITH_KNOTS('',3,(#45284,#45285,#45286,#45287,#45288,
#45289,#45290,#45291,#45292,#45293),.UNSPECIFIED.,.F.,.F.,(4,1,1,1,1,1,
1,4),(40.8407044966672,41.4599301540511,42.4542713067315,43.448612459412,
44.4429536120924,45.4372947647728,46.4316359174533,47.1238898038468),
 .UNSPECIFIED.);
#1021=B_SPLINE_CURVE_WITH_KNOTS('',3,(#45294,#45295,#45296,#45297,#45298,
#45299,#45300,#45301,#45302,#45303),.UNSPECIFIED.,.F.,.F.,(4,1,1,1,1,1,
1,4),(40.8407044966672,41.2691733973593,42.2606734777174,43.2521735580755,
44.2436736384336,45.2351737187918,46.2266737991499,47.1238898038468),
 .UNSPECIFIED.);
#1022=B_SPLINE_CURVE_WITH_KNOTS('',3,(#45308,#45309,#45310,#45311,#45312,
#45313,#45314,#45315,#45316,#45317),.UNSPECIFIED.,.F.,.F.,(4,1,1,1,1,1,
1,4),(34.5575191894876,35.4938832379685,36.4882243906489,37.4825655433293,
38.4769066960098,39.4712478486902,40.4655890013707,40.8407044966672),
 .UNSPECIFIED.);
#1023=B_SPLINE_CURVE_WITH_KNOTS('',3,(#45318,#45319,#45320,#45321,#45322,
#45323,#45324,#45325,#45326,#45327),.UNSPECIFIED.,.F.,.F.,(4,1,1,1,1,1,
1,4),(34.5575191894876,35.3201729152105,36.3116729955686,37.3031730759268,
38.2946731562849,39.286173236643,40.2776733170011,40.8407044966672),
 .UNSPECIFIED.);
#1024=B_SPLINE_CURVE_WITH_KNOTS('',3,(#45332,#45333,#45334,#45335,#45336,
#45337,#45338,#45339,#45340,#45341,#45342),.UNSPECIFIED.,.F.,.F.,(4,1,1,
1,1,1,1,1,4),(28.274333882308,28.5334951692054,29.5278363218858,30.5221774745663,
31.5165186272467,32.5108597799272,33.5052009326076,34.499542085288,34.5575191894876),
 .UNSPECIFIED.);
#1025=B_SPLINE_CURVE_WITH_KNOTS('',3,(#45343,#45344,#45345,#45346,#45347,
#45348,#45349,#45350,#45351,#45352,#45353),.UNSPECIFIED.,.F.,.F.,(4,1,1,
1,1,1,1,1,4),(28.274333882308,28.3796723527036,29.3711724330617,30.3626725134198,
31.354172593778,32.3456726741361,33.3371727544942,34.3286728348524,34.5575191894876),
 .UNSPECIFIED.);
#1026=B_SPLINE_CURVE_WITH_KNOTS('',3,(#45358,#45359,#45360,#45361,#45362,
#45363,#45364,#45365,#45366,#45367),.UNSPECIFIED.,.F.,.F.,(4,1,1,1,1,1,
1,4),(21.9911485751284,22.5674482531228,23.5617894058032,24.5561305584837,
25.5504717111641,26.5448128638445,27.539154016525,28.274333882308),
 .UNSPECIFIED.);
#1027=B_SPLINE_CURVE_WITH_KNOTS('',3,(#45368,#45369,#45370,#45371,#45372,
#45373,#45374,#45375,#45376,#45377),.UNSPECIFIED.,.F.,.F.,(4,1,1,1,1,1,
1,4),(21.9911485751284,22.4306718705548,23.4221719509129,24.4136720312711,
25.4051721116292,26.3966721919873,27.3881722723455,28.274333882308),
 .UNSPECIFIED.);
#1028=B_SPLINE_CURVE_WITH_KNOTS('',3,(#45383,#45384,#45385,#45386),
 .UNSPECIFIED.,.F.,.F.,(4,4),(15.4901713080479,15.7079632679489),
 .UNSPECIFIED.);
#1029=B_SPLINE_CURVE_WITH_KNOTS('',3,(#45388,#45389,#45390,#45391,#45392,
#45393,#45394,#45395,#45396,#45397),.UNSPECIFIED.,.F.,.F.,(4,2,2,2,4),(1.39069260388053,
1.50658326762018,1.62247393135982,1.73836536826693,1.78923484994644),
 .UNSPECIFIED.);
#1030=B_SPLINE_CURVE_WITH_KNOTS('',3,(#45399,#45400,#45401,#45402),
 .UNSPECIFIED.,.F.,.F.,(4,4),(1.32762608770811,1.39069260388053),
 .UNSPECIFIED.);
#1031=B_SPLINE_CURVE_WITH_KNOTS('',3,(#45403,#45404,#45405,#45406,#45407,
#45408),.UNSPECIFIED.,.F.,.F.,(4,1,1,4),(13.9260590743719,14.6127190316793,
15.6070601843597,15.7079632679489),.UNSPECIFIED.);
#1032=B_SPLINE_CURVE_WITH_KNOTS('',3,(#45924,#45925,#45926,#45927,#45928,
#45929,#45930,#45931,#45932,#45933),.UNSPECIFIED.,.F.,.F.,(4,2,2,2,4),(0.,
0.0922653926040451,0.19687474867418,0.27592539811023,0.366392236014044),
 .UNSPECIFIED.);
#1033=B_SPLINE_CURVE_WITH_KNOTS('',3,(#45934,#45935,#45936,#45937,#45938,
#45939,#45940,#45941,#45942,#45943,#45944,#45945,#45946,#45947,#45948,#45949,
#45950,#45951,#45952,#45953,#45954,#45955),.UNSPECIFIED.,.F.,.F.,(4,3,3,
3,3,3,3,4),(-10.1321597128207,-9.71411823813461,-8.71977708545417,-7.72543593277374,
-6.7310947800933,-5.73675362741286,-4.74241247473242,-3.84897440564112),
 .UNSPECIFIED.);
#1034=B_SPLINE_CURVE_WITH_KNOTS('',3,(#45956,#45957,#45958,#45959,#45960,
#45961,#45962,#45963,#45964,#45965,#45966,#45967,#45968,#45969,#45970,#45971,
#45972,#45973,#45974,#45975,#45976,#45977,#45978,#45979,#45980,#45981,#45982,
#45983,#45984,#45985,#45986,#45987,#45988,#45989,#45990,#45991,#45992,#45993,
#45994,#45995,#45996,#45997,#45998,#45999,#46000,#46001,#46002,#46003,#46004,
#46005,#46006,#46007,#46008,#46009,#46010,#46011,#46012,#46013,#46014,#46015,
#46016,#46017,#46018,#46019,#46020,#46021,#46022,#46023,#46024,#46025,#46026,
#46027,#46028,#46029,#46030,#46031,#46032,#46033,#46034,#46035,#46036,#46037,
#46038,#46039,#46040,#46041,#46042,#46043,#46044,#46045,#46046,#46047,#46048,
#46049),.UNSPECIFIED.,.F.,.F.,(4,3,3,3,3,3,3,3,3,3,3,3,3,3,3,3,3,3,3,3,
3,3,3,3,3,3,3,3,3,3,3,4),(-0.566847306048092,-0.536659932336638,-0.506051628309191,
-0.497421280406101,-0.490480107277087,-0.460332319899778,-0.437026301553265,
-0.424536425828322,-0.419839798678714,-0.39041568100221,-0.361282804033577,
-0.332973937139576,-0.318201496136602,-0.312453900617058,-0.308226501095536,
-0.280245932615023,-0.273884173127677,-0.245401703722135,-0.215623103089417,
-0.205167690233524,-0.200844138142904,-0.173009394645689,-0.1452391401898,
-0.117941713188566,-0.104095611372543,-0.0998982711600488,-0.0958071190833449,
-0.0691345029495114,-0.0429122063821633,-0.0175007642606556,-0.00717289866038673,
0.),.UNSPECIFIED.);
#1035=B_SPLINE_CURVE_WITH_KNOTS('',3,(#46050,#46051,#46052,#46053,#46054,
#46055,#46056,#46057,#46058,#46059),.UNSPECIFIED.,.F.,.F.,(4,1,1,1,1,1,
1,4),(15.7079632679489,16.6014013370402,17.5957424897206,18.590083642401,
19.5844247950815,20.5787659477619,21.5731071004423,21.9911485751284),
 .UNSPECIFIED.);
#1036=B_SPLINE_CURVE_WITH_KNOTS('',3,(#46061,#46062,#46063,#46064,#46065,
#46066,#46067,#46068,#46069,#46070),.UNSPECIFIED.,.F.,.F.,(4,1,1,1,1,1,
1,4),(15.7079632679489,16.481671388406,17.4731714687642,18.4646715491223,
19.4561716294804,20.4476717098386,21.4391717901967,21.9911485751284),
 .UNSPECIFIED.);
#1037=B_SPLINE_CURVE_WITH_KNOTS('',3,(#46543,#46544,#46545,#46546,#46547,
#46548,#46549,#46550,#46551,#46552,#46553,#46554,#46555,#46556,#46557,#46558,
#46559,#46560,#46561,#46562,#46563,#46564,#46565,#46566,#46567,#46568,#46569,
#46570,#46571,#46572,#46573,#46574,#46575,#46576,#46577,#46578,#46579,#46580,
#46581,#46582,#46583,#46584,#46585,#46586,#46587,#46588,#46589,#46590,#46591),
 .UNSPECIFIED.,.F.,.F.,(4,3,3,3,3,3,3,3,3,3,3,3,3,3,3,3,4),(0.,0.0248791739331723,
0.0501121717718979,0.0650752050475519,0.0910593995310815,0.117735388481178,
0.1391452357804,0.166055098965252,0.193202261006004,0.220029692886475,0.225091895299352,
0.25325494877503,0.279552389918125,0.281418002250707,0.290257524611623,
0.319505113634681,0.339076691562976),.UNSPECIFIED.);
#1038=B_SPLINE_CURVE_WITH_KNOTS('',3,(#46592,#46593,#46594,#46595,#46596,
#46597,#46598,#46599,#46600,#46601,#46602,#46603,#46604,#46605,#46606,#46607,
#46608,#46609,#46610,#46611,#46612,#46613,#46614,#46615,#46616,#46617,#46618,
#46619,#46620,#46621,#46622,#46623,#46624,#46625,#46626,#46627,#46628,#46629,
#46630,#46631,#46632,#46633,#46634,#46635,#46636,#46637,#46638,#46639,#46640,
#46641,#46642,#46643,#46644,#46645,#46646,#46647,#46648,#46649,#46650,#46651,
#46652,#46653,#46654,#46655,#46656,#46657,#46658,#46659,#46660,#46661,#46662,
#46663,#46664,#46665,#46666,#46667,#46668,#46669,#46670,#46671,#46672,#46673,
#46674,#46675,#46676,#46677,#46678,#46679,#46680,#46681,#46682,#46683,#46684,
#46685,#46686,#46687,#46688),.UNSPECIFIED.,.F.,.F.,(4,3,3,3,3,3,3,3,3,3,
3,3,3,3,3,3,3,3,3,3,3,3,3,3,3,3,3,3,3,3,3,3,4),(-0.569248610399451,-0.543564147881696,
-0.517253215506404,-0.5103603769831,-0.504797172077816,-0.477729530540692,
-0.455926184899551,-0.447499120623838,-0.442666727878697,-0.414934144456378,
-0.386773112743309,-0.358832030543205,-0.344949714260295,-0.340765289286146,
-0.336287711713791,-0.3073583091604,-0.303302765411564,-0.275496663855623,
-0.247058322334847,-0.237724074505435,-0.232212001847737,-0.227959645025499,
-0.198971930287922,-0.169410328510115,-0.139612457779761,-0.123469388622888,
-0.118279464491879,-0.114057511149134,-0.0835165944488132,-0.0529401030670342,
-0.0229717557625582,-0.01046790452478,0.),.UNSPECIFIED.);
#1039=B_SPLINE_CURVE_WITH_KNOTS('',3,(#46689,#46690,#46691,#46692,#46693,
#46694,#46695,#46696,#46697,#46698,#46699,#46700,#46701,#46702,#46703,#46704,
#46705,#46706,#46707,#46708,#46709,#46710),.UNSPECIFIED.,.F.,.F.,(4,3,3,
3,3,3,3,4),(7.59274844815659,8.03227174358307,9.0237718239412,10.0152719042993,
11.0067719846575,11.9982720650156,12.9897721453737,13.8759337553362),
 .UNSPECIFIED.);
#1040=B_SPLINE_CURVE_WITH_KNOTS('',3,(#46845,#46846,#46847,#46848,#46849,
#46850,#46851,#46852,#46853,#46854,#46855,#46856,#46857,#46858,#46859,#46860,
#46861,#46862,#46863),.UNSPECIFIED.,.F.,.F.,(4,3,3,3,3,3,4),(-10.3757270560179,
-9.99454710422085,-8.99509239379876,-7.99563768337668,-6.9961829729546,
-5.99672826253251,-5.36129569184721),.UNSPECIFIED.);
#1041=B_SPLINE_CURVE_WITH_KNOTS('',3,(#46866,#46867,#46868,#46869,#46870,
#46871,#46872,#46873,#46874,#46875,#46876,#46877,#46878,#46879,#46880,#46881),
 .UNSPECIFIED.,.F.,.F.,(4,3,3,3,3,4),(3.29149150306132,3.89964483836103,
4.89929550487756,5.8989461713941,6.89859683791064,7.40204040071886),
 .UNSPECIFIED.);
#1042=B_SPLINE_CURVE_WITH_KNOTS('',3,(#46886,#46887,#46888,#46889,#46890,
#46891,#46892,#46893,#46894,#46895,#46896,#46897,#46898,#46899,#46900,#46901,
#46902,#46903,#46904,#46905,#46906,#46907),.UNSPECIFIED.,.F.,.F.,(4,3,3,
3,3,3,3,4),(-16.6589123631975,-15.9912753667534,-14.9918206563313,-13.9923659459092,
-12.9929112354871,-11.993456525065,-10.9940018146429,-10.3757270560179),
 .UNSPECIFIED.);
#1043=B_SPLINE_CURVE_WITH_KNOTS('',3,(#46908,#46909,#46910,#46911,#46912,
#46913,#46914,#46915,#46916,#46917,#46918,#46919,#46920,#46921,#46922,#46923,
#46924,#46925,#46926,#46927,#46928,#46929),.UNSPECIFIED.,.F.,.F.,(4,3,3,
3,3,3,3,4),(7.40204040071886,7.89824750442719,8.89789817094375,9.89754883746032,
10.8971995039769,11.8968501704934,12.89650083701,13.6852257078984),
 .UNSPECIFIED.);
#1044=B_SPLINE_CURVE_WITH_KNOTS('',3,(#46934,#46935,#46936,#46937,#46938,
#46939,#46940,#46941,#46942,#46943,#46944,#46945,#46946,#46947,#46948,#46949,
#46950,#46951,#46952,#46953,#46954,#46955),.UNSPECIFIED.,.F.,.F.,(4,3,3,
3,3,3,3,4),(-22.9420976703771,-21.9880036292859,-20.9885489188638,-19.9890942084417,
-18.9896394980196,-17.9901847875975,-16.9907300771754,-16.6589123631975),
 .UNSPECIFIED.);
#1045=B_SPLINE_CURVE_WITH_KNOTS('',3,(#46956,#46957,#46958,#46959,#46960,
#46961,#46962,#46963,#46964,#46965,#46966,#46967,#46968,#46969,#46970,#46971,
#46972,#46973,#46974,#46975,#46976,#46977,#46978,#46979,#46980),
 .UNSPECIFIED.,.F.,.F.,(4,3,3,3,3,3,3,3,4),(13.6852257078984,13.8961515035266,
14.8958021700431,15.8954528365597,16.8951035030762,17.8947541695928,18.8944048361093,
19.8940555026259,19.968411015078),.UNSPECIFIED.);
#1046=B_SPLINE_CURVE_WITH_KNOTS('',3,(#46985,#46986,#46987,#46988,#46989,
#46990,#46991,#46992,#46993,#46994,#46995,#46996,#46997,#46998,#46999,#47000,
#47001,#47002,#47003,#47004,#47005,#47006,#47007,#47008,#47009),
 .UNSPECIFIED.,.F.,.F.,(4,3,3,3,3,3,3,3,4),(-29.2252829775566,-28.9841866022405,
-27.9847318918184,-26.9852771813963,-25.9858224709742,-24.9863677605521,
-23.98691305013,-22.987458339708,-22.9420976703771),.UNSPECIFIED.);
#1047=B_SPLINE_CURVE_WITH_KNOTS('',3,(#47010,#47011,#47012,#47013,#47014,
#47015,#47016,#47017,#47018,#47019,#47020,#47021,#47022,#47023,#47024,#47025,
#47026,#47027,#47028,#47029,#47030,#47031),.UNSPECIFIED.,.F.,.F.,(4,3,3,
3,3,3,3,4),(19.968411015078,20.8937061691424,21.8933568356589,22.8930075021755,
23.892658168692,24.8923088352086,25.8919595017251,26.2515963222576),
 .UNSPECIFIED.);
#1048=B_SPLINE_CURVE_WITH_KNOTS('',3,(#47036,#47037,#47038,#47039,#47040,
#47041,#47042,#47043,#47044,#47045,#47046,#47047,#47048,#47049,#47050,#47051,
#47052,#47053,#47054,#47055,#47056,#47057),.UNSPECIFIED.,.F.,.F.,(4,3,3,
3,3,3,3,4),(-35.5084682847362,-34.980914864773,-33.9814601543509,-32.9820054439288,
-31.9825507335067,-30.9830960230846,-29.9836413126625,-29.2252829775566),
 .UNSPECIFIED.);
#1049=B_SPLINE_CURVE_WITH_KNOTS('',3,(#47058,#47059,#47060,#47061,#47062,
#47063,#47064,#47065,#47066,#47067,#47068,#47069,#47070,#47071,#47072,#47073,
#47074,#47075,#47076,#47077,#47078,#47079),.UNSPECIFIED.,.F.,.F.,(4,3,3,
3,3,3,3,4),(26.2515963222576,26.8916101682417,27.8912608347582,28.8909115012748,
29.8905621677914,30.8902128343079,31.8898635008245,32.5347816294372),
 .UNSPECIFIED.);
#1050=B_SPLINE_CURVE_WITH_KNOTS('',3,(#47084,#47085,#47086,#47087,#47088,
#47089,#47090,#47091,#47092,#47093,#47094,#47095,#47096,#47097,#47098,#47099,
#47100,#47101,#47102,#47103,#47104,#47105),.UNSPECIFIED.,.F.,.F.,(4,3,3,
3,3,3,3,4),(-41.7916535919158,-40.9776431273055,-39.9781884168834,-38.9787337064613,
-37.9792789960392,-36.9798242856171,-35.9803695751951,-35.5084682847362),
 .UNSPECIFIED.);
#1051=B_SPLINE_CURVE_WITH_KNOTS('',3,(#47106,#47107,#47108,#47109,#47110,
#47111,#47112,#47113,#47114,#47115,#47116,#47117,#47118,#47119,#47120,#47121,
#47122,#47123,#47124,#47125,#47126,#47127),.UNSPECIFIED.,.F.,.F.,(4,3,3,
3,3,3,3,4),(32.5347816294372,32.889514167341,33.8891648338576,34.8888155003741,
35.8884661668906,36.8881168334072,37.8877674999237,38.8179669366168),
 .UNSPECIFIED.);
#1052=B_SPLINE_CURVE_WITH_KNOTS('',3,(#47132,#47133,#47134,#47135,#47136,
#47137,#47138,#47139,#47140,#47141,#47142,#47143,#47144,#47145,#47146,#47147,
#47148,#47149,#47150,#47151,#47152,#47153,#47154,#47155,#47156),
 .UNSPECIFIED.,.F.,.F.,(4,3,3,3,3,3,3,3,4),(-48.0748388990954,-47.9738261002601,
-46.974371389838,-45.9749166794159,-44.9754619689938,-43.9760072585717,
-42.9765525481497,-41.9770978377276,-41.7916535919158),.UNSPECIFIED.);
#1053=B_SPLINE_CURVE_WITH_KNOTS('',3,(#47157,#47158,#47159,#47160,#47161,
#47162,#47163,#47164,#47165,#47166,#47167,#47168,#47169,#47170,#47171,#47172,
#47173,#47174,#47175,#47176,#47177,#47178,#47179,#47180,#47181),
 .UNSPECIFIED.,.F.,.F.,(4,3,3,3,3,3,3,3,4),(38.8179669366168,38.8874181664403,
39.8870688329568,40.8867194994734,41.8863701659899,42.8860208325065,43.8856714990231,
44.8853221655396,45.1011522437964),.UNSPECIFIED.);
#1054=B_SPLINE_CURVE_WITH_KNOTS('',3,(#47186,#47187,#47188,#47189,#47190,
#47191,#47192,#47193,#47194,#47195,#47196,#47197,#47198,#47199,#47200,#47201,
#47202,#47203,#47204,#47205,#47206,#47207),.UNSPECIFIED.,.F.,.F.,(4,3,3,
3,3,3,3,4),(-54.358024206275,-53.9705543627926,-52.9710996523705,-51.9716449419484,
-50.9721902315264,-49.9727355211043,-48.9732808106822,-48.0748388990954),
 .UNSPECIFIED.);
#1055=B_SPLINE_CURVE_WITH_KNOTS('',3,(#47208,#47209,#47210,#47211,#47212,
#47213,#47214,#47215,#47216,#47217,#47218,#47219,#47220,#47221,#47222,#47223,
#47224,#47225,#47226,#47227,#47228,#47229),.UNSPECIFIED.,.F.,.F.,(4,3,3,
3,3,3,3,4),(45.1011522437964,45.8849728320562,46.8846234985727,47.8842741650893,
48.8839248316058,49.8835754981223,50.8832261646389,51.384337550976),
 .UNSPECIFIED.);
#1056=B_SPLINE_CURVE_WITH_KNOTS('',3,(#47234,#47235,#47236,#47237,#47238,
#47239,#47240,#47241,#47242,#47243,#47244,#47245,#47246,#47247,#47248,#47249,
#47250,#47251,#47252,#47253,#47254,#47255),.UNSPECIFIED.,.F.,.F.,(4,3,3,
3,3,3,3,4),(-60.6412095134546,-59.9672826253251,-58.967827914903,-57.9683732044809,
-56.9689184940589,-55.9694637836368,-54.9700090732147,-54.358024206275),
 .UNSPECIFIED.);
#1057=B_SPLINE_CURVE_WITH_KNOTS('',3,(#47256,#47257,#47258,#47259,#47260,
#47261,#47262,#47263,#47264,#47265,#47266,#47267,#47268,#47269,#47270,#47271,
#47272,#47273,#47274,#47275,#47276,#47277),.UNSPECIFIED.,.F.,.F.,(4,3,3,
3,3,3,3,4),(51.384337550976,51.8828768311554,52.882527497672,53.8821781641886,
54.8818288307051,55.8814794972217,56.8811301637383,57.6675228581556),
 .UNSPECIFIED.);
#1058=B_SPLINE_CURVE_WITH_KNOTS('',3,(#47282,#47283,#47284,#47285,#47286,
#47287,#47288,#47289,#47290,#47291,#47292,#47293,#47294,#47295,#47296,#47297,
#47298,#47299,#47300,#47301,#47302,#47303),.UNSPECIFIED.,.F.,.F.,(4,3,3,
3,3,3,3,4),(-66.9243948206342,-65.9640108878576,-64.9645561774355,-63.9651014670135,
-62.9656467565914,-61.9661920461693,-60.9667373357472,-60.6412095134546),
 .UNSPECIFIED.);
#1059=B_SPLINE_CURVE_WITH_KNOTS('',3,(#47304,#47305,#47306,#47307,#47308,
#47309,#47310,#47311,#47312,#47313,#47314,#47315,#47316,#47317,#47318,#47319,
#47320,#47321,#47322,#47323,#47324,#47325,#47326,#47327,#47328),
 .UNSPECIFIED.,.F.,.F.,(4,3,3,3,3,3,3,3,4),(57.6675228581556,57.8807808302548,
58.8804314967713,59.8800821632879,60.8797328298044,61.8793834963209,62.8790341628375,
63.878684829354,63.9507081653352),.UNSPECIFIED.);
#1060=B_SPLINE_CURVE_WITH_KNOTS('',3,(#47333,#47334,#47335,#47336,#47337,
#47338,#47339,#47340,#47341,#47342,#47343,#47344,#47345,#47346,#47347,#47348,
#47349,#47350,#47351,#47352,#47353,#47354,#47355,#47356,#47357),
 .UNSPECIFIED.,.F.,.F.,(4,3,3,3,3,3,3,3,4),(-73.2075801278138,-72.9601938608122,
-71.9607391503901,-70.9612844399681,-69.9618297295459,-68.9623750191239,
-67.9629203087018,-66.9634655982797,-66.9243948206342),.UNSPECIFIED.);
#1061=B_SPLINE_CURVE_WITH_KNOTS('',3,(#47358,#47359,#47360,#47361,#47362,
#47363,#47364,#47365,#47366,#47367,#47368,#47369,#47370,#47371,#47372,#47373,
#47374,#47375,#47376,#47377,#47378,#47379),.UNSPECIFIED.,.F.,.F.,(4,3,3,
3,3,3,3,4),(63.9507081653352,64.8783354958706,65.8779861623872,66.8776368289037,
67.8772874954203,68.8769381619369,69.8765888284534,70.2338934725148),
 .UNSPECIFIED.);
#1062=B_SPLINE_CURVE_WITH_KNOTS('',3,(#47384,#47385,#47386,#47387,#47388,
#47389,#47390,#47391,#47392,#47393,#47394,#47395,#47396,#47397,#47398,#47399,
#47400,#47401,#47402,#47403,#47404,#47405),.UNSPECIFIED.,.F.,.F.,(4,3,3,
3,3,3,3,4),(-79.4907654349934,-78.9569221233447,-77.9574674129226,-76.9580127025006,
-75.9585579920785,-74.9591032816564,-73.9596485712343,-73.2075801278138),
 .UNSPECIFIED.);
#1063=B_SPLINE_CURVE_WITH_KNOTS('',3,(#47406,#47407,#47408,#47409,#47410,
#47411,#47412,#47413,#47414,#47415,#47416,#47417,#47418,#47419,#47420,#47421,
#47422,#47423,#47424,#47425,#47426,#47427),.UNSPECIFIED.,.F.,.F.,(4,3,3,
3,3,3,3,4),(70.2338934725148,70.87623949497,71.8758901614865,72.8755408280031,
73.8751914945196,74.8748421610361,75.8744928275527,76.5170787796944),
 .UNSPECIFIED.);
#1064=B_SPLINE_CURVE_WITH_KNOTS('',3,(#47432,#47433,#47434,#47435,#47436,
#47437,#47438,#47439,#47440,#47441,#47442,#47443,#47444,#47445,#47446,#47447,
#47448,#47449,#47450,#47451,#47452,#47453),.UNSPECIFIED.,.F.,.F.,(4,3,3,
3,3,3,3,4),(-85.773950742173,-84.9536503858773,-83.9541956754552,-82.9547409650331,
-81.955286254611,-80.9558315441889,-79.9563768337668,-79.4907654349934),
 .UNSPECIFIED.);
#1065=B_SPLINE_CURVE_WITH_KNOTS('',3,(#47454,#47455,#47456,#47457,#47458,
#47459,#47460,#47461,#47462,#47463,#47464,#47465,#47466,#47467,#47468,#47469,
#47470,#47471,#47472,#47473,#47474,#47475),.UNSPECIFIED.,.F.,.F.,(4,3,3,
3,3,3,3,4),(76.5170787796944,76.8741434940692,77.8737941605858,78.8734448271023,
79.8730954936189,80.8727461601354,81.872396826652,82.800264086874),
 .UNSPECIFIED.);
#1066=B_SPLINE_CURVE_WITH_KNOTS('',3,(#47480,#47481,#47482,#47483,#47484,
#47485,#47486,#47487,#47488,#47489,#47490,#47491,#47492,#47493,#47494,#47495,
#47496,#47497,#47498,#47499,#47500,#47501,#47502,#47503,#47504),
 .UNSPECIFIED.,.F.,.F.,(4,3,3,3,3,3,3,3,4),(-92.0571360493526,-91.9498333588318,
-90.9503786484097,-89.9509239379877,-88.9514692275656,-87.9520145171435,
-86.9525598067214,-85.9531050962993,-85.773950742173),.UNSPECIFIED.);
#1067=B_SPLINE_CURVE_WITH_KNOTS('',3,(#47505,#47506,#47507,#47508,#47509,
#47510,#47511,#47512,#47513,#47514,#47515,#47516,#47517,#47518,#47519,#47520,
#47521,#47522,#47523,#47524,#47525,#47526,#47527,#47528,#47529),
 .UNSPECIFIED.,.F.,.F.,(4,3,3,3,3,3,3,3,4),(82.800264086874,82.8720474931686,
83.8716981596851,84.8713488262017,85.8709994927182,86.8706501592348,87.8703008257513,
88.8699514922679,89.0834493940535),.UNSPECIFIED.);
#1068=B_SPLINE_CURVE_WITH_KNOTS('',3,(#47534,#47535,#47536,#47537,#47538,
#47539,#47540,#47541,#47542,#47543,#47544,#47545,#47546,#47547,#47548,#47549,
#47550,#47551,#47552,#47553,#47554,#47555),.UNSPECIFIED.,.F.,.F.,(4,3,3,
3,3,3,3,4),(-98.3403213565322,-97.9465616213644,-96.9471069109423,-95.9476522005202,
-94.9481974900981,-93.948742779676,-92.9492880692539,-92.0571360493526),
 .UNSPECIFIED.);
#1069=B_SPLINE_CURVE_WITH_KNOTS('',3,(#47556,#47557,#47558,#47559,#47560,
#47561,#47562,#47563,#47564,#47565,#47566,#47567,#47568,#47569,#47570,#47571,
#47572,#47573,#47574,#47575,#47576,#47577),.UNSPECIFIED.,.F.,.F.,(4,3,3,
3,3,3,3,4),(89.0834493940535,89.8696021587844,90.869252825301,91.8689034918175,
92.8685541583341,93.8682048248506,94.8678554913672,95.3666347012331),
 .UNSPECIFIED.);
#1070=B_SPLINE_CURVE_WITH_KNOTS('',3,(#47582,#47583,#47584,#47585,#47586,
#47587,#47588,#47589,#47590,#47591,#47592,#47593,#47594,#47595,#47596,#47597,
#47598,#47599,#47600,#47601,#47602,#47603),.UNSPECIFIED.,.F.,.F.,(4,3,3,
3,3,3,3,4),(-104.623506663712,-103.943289883897,-102.943835173475,-101.944380463053,
-100.944925752631,-99.9454710422085,-98.9460163317864,-98.3403213565322),
 .UNSPECIFIED.);
#1071=B_SPLINE_CURVE_WITH_KNOTS('',3,(#47604,#47605,#47606,#47607,#47608,
#47609,#47610,#47611,#47612,#47613,#47614,#47615,#47616,#47617,#47618,#47619,
#47620,#47621,#47622,#47623,#47624,#47625),.UNSPECIFIED.,.F.,.F.,(4,3,3,
3,3,3,3,4),(95.3666347012331,95.8675061578838,96.8671568244003,97.8668074909168,
98.8664581574334,99.8661088239499,100.865759490466,101.649820008413),
 .UNSPECIFIED.);
#1072=B_SPLINE_CURVE_WITH_KNOTS('',3,(#47630,#47631,#47632,#47633,#47634,
#47635,#47636,#47637,#47638,#47639,#47640,#47641,#47642,#47643,#47644,#47645,
#47646,#47647,#47648,#47649,#47650,#47651),.UNSPECIFIED.,.F.,.F.,(4,3,3,
3,3,3,3,4),(-110.906691970891,-109.940018146429,-108.940563436007,-107.941108725585,
-106.941654015163,-105.942199304741,-104.942744594319,-104.623506663712),
 .UNSPECIFIED.);
#1073=B_SPLINE_CURVE_WITH_KNOTS('',3,(#47652,#47653,#47654,#47655,#47656,
#47657,#47658,#47659,#47660,#47661,#47662,#47663,#47664,#47665,#47666,#47667,
#47668,#47669,#47670,#47671,#47672,#47673,#47674,#47675,#47676),
 .UNSPECIFIED.,.F.,.F.,(4,3,3,3,3,3,3,3,4),(101.649820008413,101.865410156983,
102.8650608235,103.864711490016,104.864362156533,105.864012823049,106.863663489566,
107.863314156082,107.933005315592),.UNSPECIFIED.);
#1074=B_SPLINE_CURVE_WITH_KNOTS('',3,(#47681,#47682,#47683,#47684,#47685,
#47686,#47687,#47688,#47689,#47690,#47691,#47692,#47693,#47694,#47695,#47696,
#47697,#47698,#47699,#47700,#47701,#47702,#47703,#47704,#47705),
 .UNSPECIFIED.,.F.,.F.,(4,3,3,3,3,3,3,3,4),(-117.189877278071,-116.936201119384,
-115.936746408962,-114.93729169854,-113.937836988118,-112.938382277696,
-111.938927567274,-110.939472856851,-110.906691970891),.UNSPECIFIED.);
#1075=B_SPLINE_CURVE_WITH_KNOTS('',3,(#47706,#47707,#47708,#47709,#47710,
#47711,#47712,#47713,#47714,#47715,#47716,#47717,#47718,#47719,#47720,#47721,
#47722,#47723,#47724,#47725,#47726,#47727),.UNSPECIFIED.,.F.,.F.,(4,3,3,
3,3,3,3,4),(107.933005315592,108.862964822599,109.862615489115,110.862266155632,
111.861916822149,112.861567488665,113.861218155182,114.216190622772),
 .UNSPECIFIED.);
#1076=B_SPLINE_CURVE_WITH_KNOTS('',3,(#47732,#47733,#47734,#47735,#47736,
#47737,#47738,#47739,#47740,#47741,#47742,#47743,#47744,#47745,#47746,#47747,
#47748,#47749,#47750,#47751,#47752,#47753),.UNSPECIFIED.,.F.,.F.,(4,3,3,
3,3,3,3,4),(-123.473062585251,-122.932929381916,-121.933474671494,-120.934019961072,
-119.93456525065,-118.935110540228,-117.935655829806,-117.189877278071),
 .UNSPECIFIED.);
#1077=B_SPLINE_CURVE_WITH_KNOTS('',3,(#47754,#47755,#47756,#47757,#47758,
#47759,#47760,#47761,#47762,#47763,#47764,#47765,#47766,#47767,#47768,#47769,
#47770,#47771,#47772,#47773,#47774,#47775),.UNSPECIFIED.,.F.,.F.,(4,3,3,
3,3,3,3,4),(114.216190622772,114.860868821698,115.860519488215,116.860170154731,
117.859820821248,118.859471487764,119.859122154281,120.499375929952),
 .UNSPECIFIED.);
#1078=B_SPLINE_CURVE_WITH_KNOTS('',3,(#47780,#47781,#47782,#47783,#47784,
#47785,#47786,#47787,#47788,#47789,#47790,#47791,#47792,#47793,#47794,#47795,
#47796,#47797,#47798,#47799,#47800,#47801),.UNSPECIFIED.,.F.,.F.,(4,3,3,
3,3,3,3,4),(-129.75624789243,-128.929657644449,-127.930202934027,-126.930748223605,
-125.931293513183,-124.931838802761,-123.932384092339,-123.473062585251),
 .UNSPECIFIED.);
#1079=B_SPLINE_CURVE_WITH_KNOTS('',3,(#47802,#47803,#47804,#47805,#47806,
#47807,#47808,#47809,#47810,#47811,#47812,#47813,#47814,#47815,#47816,#47817,
#47818,#47819,#47820,#47821,#47822,#47823),.UNSPECIFIED.,.F.,.F.,(4,3,3,
3,3,3,3,4),(120.499375929952,120.858772820798,121.858423487314,122.858074153831,
123.857724820347,124.857375486864,125.85702615338,126.782561237131),
 .UNSPECIFIED.);
#1080=B_SPLINE_CURVE_WITH_KNOTS('',3,(#47828,#47829,#47830,#47831,#47832,
#47833,#47834,#47835,#47836,#47837,#47838,#47839,#47840,#47841,#47842,#47843,
#47844,#47845,#47846,#47847,#47848,#47849,#47850,#47851,#47852),
 .UNSPECIFIED.,.F.,.F.,(4,3,3,3,3,3,3,3,4),(-136.03943319961,-135.925840617404,
-134.926385906981,-133.926931196559,-132.927476486137,-131.928021775715,
-130.928567065293,-129.929112354871,-129.75624789243),.UNSPECIFIED.);
#1081=B_SPLINE_CURVE_WITH_KNOTS('',3,(#47853,#47854,#47855,#47856,#47857,
#47858,#47859,#47860,#47861,#47862,#47863,#47864,#47865,#47866,#47867,#47868,
#47869,#47870,#47871,#47872,#47873,#47874,#47875,#47876,#47877),
 .UNSPECIFIED.,.F.,.F.,(4,3,3,3,3,3,3,3,4),(126.782561237131,126.856676819897,
127.856327486413,128.85597815293,129.855628819447,130.855279485963,131.85493015248,
132.854580818996,133.065746544311),.UNSPECIFIED.);
#1082=B_SPLINE_CURVE_WITH_KNOTS('',3,(#47882,#47883,#47884,#47885,#47886,
#47887,#47888,#47889,#47890,#47891,#47892,#47893,#47894,#47895,#47896,#47897,
#47898,#47899,#47900,#47901,#47902,#47903),.UNSPECIFIED.,.F.,.F.,(4,3,3,
3,3,3,3,4),(-142.322618506789,-141.922568879936,-140.923114169514,-139.923659459092,
-138.92420474867,-137.924750038248,-136.925295327826,-136.03943319961),
 .UNSPECIFIED.);
#1083=B_SPLINE_CURVE_WITH_KNOTS('',3,(#47904,#47905,#47906,#47907,#47908,
#47909,#47910,#47911,#47912,#47913,#47914,#47915,#47916,#47917,#47918,#47919,
#47920,#47921,#47922,#47923,#47924,#47925),.UNSPECIFIED.,.F.,.F.,(4,3,3,
3,3,3,3,4),(133.065746544311,133.854231485513,134.853882152029,135.853532818546,
136.853183485062,137.852834151579,138.852484818095,139.34893185149),
 .UNSPECIFIED.);
#1084=B_SPLINE_CURVE_WITH_KNOTS('',3,(#47930,#47931,#47932,#47933,#47934,
#47935,#47936,#47937,#47938,#47939,#47940,#47941,#47942,#47943,#47944,#47945,
#47946,#47947,#47948,#47949,#47950,#47951),.UNSPECIFIED.,.F.,.F.,(4,3,3,
3,3,3,3,4),(-148.605803813969,-147.919297142469,-146.919842432047,-145.920387721624,
-144.920933011202,-143.92147830078,-142.922023590358,-142.322618506789),
 .UNSPECIFIED.);
#1085=B_SPLINE_CURVE_WITH_KNOTS('',3,(#47952,#47953,#47954,#47955,#47956,
#47957,#47958,#47959,#47960,#47961,#47962,#47963,#47964,#47965,#47966,#47967,
#47968,#47969,#47970,#47971,#47972,#47973),.UNSPECIFIED.,.F.,.F.,(4,3,3,
3,3,3,3,4),(139.34893185149,139.852135484612,140.851786151129,141.851436817645,
142.851087484162,143.850738150678,144.850388817195,145.63211715867),
 .UNSPECIFIED.);
#1086=B_SPLINE_CURVE_WITH_KNOTS('',3,(#47978,#47979,#47980,#47981,#47982,
#47983,#47984,#47985,#47986,#47987,#47988,#47989,#47990,#47991,#47992,#47993,
#47994,#47995,#47996,#47997,#47998,#47999),.UNSPECIFIED.,.F.,.F.,(4,3,3,
3,3,3,3,4),(-154.888989121148,-153.916025405001,-152.916570694579,-151.917115984157,
-150.917661273735,-149.918206563313,-148.918751852891,-148.605803813969),
 .UNSPECIFIED.);
#1087=B_SPLINE_CURVE_WITH_KNOTS('',3,(#48000,#48001,#48002,#48003,#48004,
#48005,#48006,#48007,#48008,#48009,#48010,#48011,#48012,#48013,#48014,#48015,
#48016,#48017,#48018,#48019,#48020,#48021,#48022,#48023,#48024),
 .UNSPECIFIED.,.F.,.F.,(4,3,3,3,3,3,3,3,4),(145.63211715867,145.850039483711,
146.849690150228,147.849340816744,148.848991483261,149.848642149777,150.848292816294,
151.847943482811,151.915302465849),.UNSPECIFIED.);
#1088=B_SPLINE_CURVE_WITH_KNOTS('',3,(#48029,#48030,#48031,#48032,#48033,
#48034,#48035,#48036,#48037,#48038,#48039,#48040,#48041,#48042,#48043,#48044,
#48045,#48046,#48047,#48048,#48049,#48050,#48051,#48052,#48053),
 .UNSPECIFIED.,.F.,.F.,(4,3,3,3,3,3,3,3,4),(-161.172174428328,-160.912208377956,
-159.912753667534,-158.913298957112,-157.913844246689,-156.914389536267,
-155.914934825845,-154.915480115423,-154.888989121148),.UNSPECIFIED.);
#1089=B_SPLINE_CURVE_WITH_KNOTS('',3,(#48054,#48055,#48056,#48057,#48058,
#48059,#48060,#48061,#48062,#48063,#48064,#48065,#48066,#48067,#48068,#48069,
#48070,#48071,#48072,#48073,#48074,#48075),.UNSPECIFIED.,.F.,.F.,(4,3,3,
3,3,3,3,4),(151.915302465849,152.847594149327,153.847244815844,154.84689548236,
155.846546148877,156.846196815393,157.84584748191,158.198487773029),
 .UNSPECIFIED.);
#1090=B_SPLINE_CURVE_WITH_KNOTS('',3,(#48080,#48081,#48082,#48083,#48084,
#48085,#48086,#48087,#48088,#48089,#48090,#48091,#48092,#48093,#48094,#48095,
#48096,#48097,#48098,#48099,#48100,#48101),.UNSPECIFIED.,.F.,.F.,(4,3,3,
3,3,3,3,4),(-167.455359735508,-166.908936640488,-165.909481930066,-164.910027219644,
-163.910572509222,-162.9111177988,-161.911663088378,-161.172174428328),
 .UNSPECIFIED.);
#1091=B_SPLINE_CURVE_WITH_KNOTS('',3,(#48102,#48103,#48104,#48105,#48106,
#48107,#48108,#48109,#48110,#48111,#48112,#48113,#48114,#48115,#48116,#48117,
#48118,#48119,#48120,#48121,#48122,#48123),.UNSPECIFIED.,.F.,.F.,(4,3,3,
3,3,3,3,4),(158.198487773029,158.845498148427,159.845148814943,160.84479948146,
161.844450147976,162.844100814493,163.843751481009,164.481673080209),
 .UNSPECIFIED.);
#1092=B_SPLINE_CURVE_WITH_KNOTS('',3,(#48128,#48129,#48130,#48131,#48132,
#48133,#48134,#48135,#48136,#48137,#48138,#48139,#48140,#48141,#48142,#48143,
#48144,#48145,#48146,#48147,#48148,#48149),.UNSPECIFIED.,.F.,.F.,(4,3,3,
3,3,3,3,4),(-173.738545042687,-172.905664903021,-171.906210192599,-170.906755482177,
-169.907300771755,-168.907846061332,-167.90839135091,-167.455359735508),
 .UNSPECIFIED.);
#1093=B_SPLINE_CURVE_WITH_KNOTS('',3,(#48150,#48151,#48152,#48153,#48154,
#48155,#48156,#48157,#48158,#48159,#48160,#48161,#48162,#48163,#48164,#48165,
#48166,#48167,#48168,#48169,#48170,#48171),.UNSPECIFIED.,.F.,.F.,(4,3,3,
3,3,3,3,4),(164.481673080209,164.843402147526,165.843052814042,166.842703480559,
167.842354147075,168.842004813592,169.841655480109,170.764858387388),
 .UNSPECIFIED.);
#1094=B_SPLINE_CURVE_WITH_KNOTS('',3,(#48176,#48177,#48178,#48179,#48180,
#48181,#48182,#48183,#48184,#48185,#48186,#48187,#48188,#48189,#48190,#48191,
#48192,#48193,#48194,#48195,#48196,#48197,#48198,#48199,#48200),
 .UNSPECIFIED.,.F.,.F.,(4,3,3,3,3,3,3,3,4),(-180.021730349867,-179.901847875975,
-178.902393165553,-177.902938455131,-176.903483744709,-175.904029034287,
-174.904574323865,-173.905119613443,-173.738545042687),.UNSPECIFIED.);
#1095=B_SPLINE_CURVE_WITH_KNOTS('',3,(#48201,#48202,#48203,#48204,#48205,
#48206,#48207,#48208,#48209,#48210,#48211,#48212,#48213,#48214,#48215,#48216,
#48217,#48218,#48219,#48220,#48221,#48222,#48223,#48224,#48225),
 .UNSPECIFIED.,.F.,.F.,(4,3,3,3,3,3,3,3,4),(170.764858387388,170.841306146625,
171.840956813142,172.840607479658,173.840258146175,174.839908812691,175.839559479208,
176.839210145724,177.048043694568),.UNSPECIFIED.);
#1096=B_SPLINE_CURVE_WITH_KNOTS('',3,(#48230,#48231,#48232,#48233,#48234,
#48235,#48236,#48237,#48238,#48239,#48240,#48241,#48242,#48243,#48244,#48245,
#48246,#48247,#48248,#48249,#48250,#48251),.UNSPECIFIED.,.F.,.F.,(4,3,3,
3,3,3,3,4),(-186.304915657046,-185.898576138508,-184.899121428086,-183.899666717664,
-182.900212007242,-181.90075729682,-180.901302586397,-180.021730349867),
 .UNSPECIFIED.);
#1097=B_SPLINE_CURVE_WITH_KNOTS('',3,(#48252,#48253,#48254,#48255,#48256,
#48257,#48258,#48259,#48260,#48261,#48262,#48263,#48264,#48265,#48266,#48267,
#48268,#48269,#48270,#48271,#48272,#48273),.UNSPECIFIED.,.F.,.F.,(4,3,3,
3,3,3,3,4),(177.048043694568,177.838860812241,178.838511478758,179.838162145274,
180.837812811791,181.837463478307,182.837114144824,183.331229001747),
 .UNSPECIFIED.);
#1098=B_SPLINE_CURVE_WITH_KNOTS('',3,(#48278,#48279,#48280,#48281,#48282,
#48283,#48284,#48285,#48286,#48287,#48288,#48289,#48290,#48291,#48292,#48293,
#48294,#48295,#48296,#48297,#48298,#48299),.UNSPECIFIED.,.F.,.F.,(4,3,3,
3,3,3,3,4),(-192.588100964226,-191.89530440104,-190.895849690618,-189.896394980196,
-188.896940269774,-187.897485559352,-186.89803084893,-186.304915657046),
 .UNSPECIFIED.);
#1099=B_SPLINE_CURVE_WITH_KNOTS('',3,(#48300,#48301,#48302,#48303,#48304,
#48305,#48306,#48307,#48308,#48309,#48310,#48311,#48312,#48313,#48314,#48315,
#48316,#48317,#48318,#48319,#48320,#48321),.UNSPECIFIED.,.F.,.F.,(4,3,3,
3,3,3,3,4),(183.331229001747,183.83676481134,184.836415477857,185.836066144373,
186.83571681089,187.835367477406,188.835018143923,189.614414308927),
 .UNSPECIFIED.);
#1100=B_SPLINE_CURVE_WITH_KNOTS('',3,(#48326,#48327,#48328,#48329,#48330,
#48331,#48332,#48333,#48334,#48335,#48336,#48337,#48338,#48339,#48340,#48341,
#48342,#48343,#48344,#48345,#48346,#48347),.UNSPECIFIED.,.F.,.F.,(4,3,3,
3,3,3,3,4),(-198.871286271405,-197.892032663573,-196.892577953151,-195.893123242729,
-194.893668532307,-193.894213821885,-192.894759111462,-192.588100964226),
 .UNSPECIFIED.);
#1101=B_SPLINE_CURVE_WITH_KNOTS('',3,(#48348,#48349,#48350,#48351,#48352,
#48353,#48354,#48355,#48356,#48357,#48358,#48359,#48360,#48361,#48362,#48363,
#48364,#48365,#48366,#48367,#48368,#48369,#48370,#48371,#48372),
 .UNSPECIFIED.,.F.,.F.,(4,3,3,3,3,3,3,3,4),(189.614414308927,189.834668810439,
190.834319476956,191.833970143473,192.833620809989,193.833271476506,194.832922143022,
195.832572809539,195.897599616106),.UNSPECIFIED.);
#1102=B_SPLINE_CURVE_WITH_KNOTS('',3,(#48377,#48378,#48379,#48380,#48381,
#48382,#48383,#48384,#48385,#48386,#48387,#48388,#48389,#48390,#48391,#48392,
#48393,#48394,#48395,#48396,#48397,#48398,#48399,#48400,#48401),
 .UNSPECIFIED.,.F.,.F.,(4,3,3,3,3,3,3,3,4),(-205.154471578585,-204.888215636527,
-203.888760926105,-202.889306215683,-201.889851505261,-200.890396794839,
-199.890942084417,-198.891487373995,-198.871286271405),.UNSPECIFIED.);
#1103=B_SPLINE_CURVE_WITH_KNOTS('',3,(#48402,#48403,#48404,#48405,#48406,
#48407,#48408,#48409,#48410,#48411,#48412,#48413,#48414,#48415,#48416,#48417,
#48418,#48419,#48420,#48421,#48422,#48423),.UNSPECIFIED.,.F.,.F.,(4,3,3,
3,3,3,3,4),(195.897599616106,196.832223476055,197.831874142572,198.831524809089,
199.831175475605,200.830826142122,201.830476808638,202.180784923286),
 .UNSPECIFIED.);
#1104=B_SPLINE_CURVE_WITH_KNOTS('',3,(#48428,#48429,#48430,#48431,#48432,
#48433,#48434,#48435,#48436,#48437,#48438,#48439,#48440,#48441,#48442,#48443,
#48444,#48445,#48446,#48447,#48448,#48449),.UNSPECIFIED.,.F.,.F.,(4,3,3,
3,3,3,3,4),(-211.437656885764,-210.88494389906,-209.885489188638,-208.886034478216,
-207.886579767794,-206.887125057372,-205.88767034695,-205.154471578585),
 .UNSPECIFIED.);
#1105=B_SPLINE_CURVE_WITH_KNOTS('',3,(#48450,#48451,#48452,#48453,#48454,
#48455,#48456,#48457,#48458,#48459,#48460,#48461,#48462,#48463,#48464,#48465,
#48466,#48467,#48468,#48469,#48470,#48471),.UNSPECIFIED.,.F.,.F.,(4,3,3,
3,3,3,3,4),(202.180784923286,202.830127475155,203.829778141671,204.829428808188,
205.829079474704,206.828730141221,207.828380807737,208.463970230465),
 .UNSPECIFIED.);
#1106=B_SPLINE_CURVE_WITH_KNOTS('',3,(#48476,#48477,#48478,#48479,#48480,
#48481,#48482,#48483,#48484,#48485,#48486,#48487,#48488,#48489,#48490,#48491,
#48492,#48493,#48494,#48495,#48496,#48497),.UNSPECIFIED.,.F.,.F.,(4,3,3,
3,3,3,3,4),(-217.720842192944,-216.881672161592,-215.88221745117,-214.882762740748,
-213.883308030326,-212.883853319904,-211.884398609482,-211.437656885764),
 .UNSPECIFIED.);
#1107=B_SPLINE_CURVE_WITH_KNOTS('',3,(#48498,#48499,#48500,#48501,#48502,
#48503,#48504,#48505,#48506,#48507,#48508,#48509,#48510,#48511,#48512,#48513,
#48514,#48515,#48516,#48517,#48518,#48519),.UNSPECIFIED.,.F.,.F.,(4,3,3,
3,3,3,3,4),(208.463970230465,208.828031474254,209.827682140771,210.827332807287,
211.826983473804,212.82663414032,213.826284806837,214.747155537645),
 .UNSPECIFIED.);
#1108=B_SPLINE_CURVE_WITH_KNOTS('',3,(#48524,#48525,#48526,#48527,#48528,
#48529,#48530,#48531,#48532,#48533,#48534,#48535,#48536,#48537,#48538,#48539,
#48540,#48541,#48542,#48543,#48544,#48545,#48546,#48547,#48548),
 .UNSPECIFIED.,.F.,.F.,(4,3,3,3,3,3,3,3,4),(-224.004027500124,-223.877855134547,
-222.878400424125,-221.878945713703,-220.879491003281,-219.880036292859,
-218.880581582437,-217.881126872015,-217.720842192944),.UNSPECIFIED.);
#1109=B_SPLINE_CURVE_WITH_KNOTS('',3,(#48549,#48550,#48551,#48552,#48553,
#48554,#48555,#48556,#48557,#48558,#48559,#48560,#48561,#48562,#48563,#48564,
#48565,#48566,#48567,#48568,#48569,#48570,#48571,#48572,#48573),
 .UNSPECIFIED.,.F.,.F.,(4,3,3,3,3,3,3,3,4),(214.747155537645,214.825935473353,
215.82558613987,216.825236806386,217.824887472903,218.82453813942,219.824188805936,
220.823839472453,221.030340844825),.UNSPECIFIED.);
#1110=B_SPLINE_CURVE_WITH_KNOTS('',3,(#48578,#48579,#48580,#48581,#48582,
#48583,#48584,#48585,#48586,#48587,#48588,#48589,#48590,#48591,#48592,#48593,
#48594,#48595,#48596,#48597,#48598,#48599),.UNSPECIFIED.,.F.,.F.,(4,3,3,
3,3,3,3,4),(-230.287212807303,-229.87458339708,-228.875128686658,-227.875673976235,
-226.876219265813,-225.876764555391,-224.877309844969,-224.004027500124),
 .UNSPECIFIED.);
#1111=B_SPLINE_CURVE_WITH_KNOTS('',3,(#48600,#48601,#48602,#48603,#48604,
#48605,#48606,#48607,#48608,#48609,#48610,#48611,#48612,#48613,#48614,#48615,
#48616,#48617,#48618,#48619,#48620,#48621),.UNSPECIFIED.,.F.,.F.,(4,3,3,
3,3,3,3,4),(221.030340844825,221.823490138969,222.823140805486,223.822791472002,
224.822442138519,225.822092805035,226.821743471552,227.313526152004),
 .UNSPECIFIED.);
#1112=B_SPLINE_CURVE_WITH_KNOTS('',3,(#48626,#48627,#48628,#48629,#48630,
#48631,#48632,#48633,#48634,#48635,#48636,#48637,#48638,#48639,#48640,#48641,
#48642,#48643,#48644,#48645,#48646,#48647),.UNSPECIFIED.,.F.,.F.,(4,3,3,
3,3,3,3,4),(-236.570398114483,-235.871311659612,-234.87185694919,-233.872402238768,
-232.872947528346,-231.873492817924,-230.874038107502,-230.287212807303),
 .UNSPECIFIED.);
#1113=B_SPLINE_CURVE_WITH_KNOTS('',3,(#48648,#48649,#48650,#48651,#48652,
#48653,#48654,#48655,#48656,#48657,#48658,#48659,#48660,#48661,#48662,#48663,
#48664,#48665,#48666,#48667,#48668,#48669),.UNSPECIFIED.,.F.,.F.,(4,3,3,
3,3,3,3,4),(227.313526152004,227.821394138069,228.821044804585,229.820695471102,
230.820346137618,231.819996804135,232.819647470651,233.596711459184),
 .UNSPECIFIED.);
#1114=B_SPLINE_CURVE_WITH_KNOTS('',3,(#48674,#48675,#48676,#48677,#48678,
#48679,#48680,#48681,#48682,#48683,#48684,#48685,#48686,#48687,#48688,#48689,
#48690,#48691,#48692,#48693,#48694,#48695),.UNSPECIFIED.,.F.,.F.,(4,3,3,
3,3,3,3,4),(-242.853583421662,-241.868039922145,-240.868585211723,-239.8691305013,
-238.869675790878,-237.870221080456,-236.870766370034,-236.570398114483),
 .UNSPECIFIED.);
#1115=B_SPLINE_CURVE_WITH_KNOTS('',3,(#48696,#48697,#48698,#48699,#48700,
#48701,#48702,#48703,#48704,#48705,#48706,#48707,#48708,#48709,#48710,#48711,
#48712,#48713,#48714,#48715,#48716,#48717,#48718,#48719,#48720),
 .UNSPECIFIED.,.F.,.F.,(4,3,3,3,3,3,3,3,4),(233.596711459184,233.819298137168,
234.818948803684,235.818599470201,236.818250136717,237.817900803234,238.817551469751,
239.817202136267,239.879896766363),.UNSPECIFIED.);
#1116=B_SPLINE_CURVE_WITH_KNOTS('',3,(#48725,#48726,#48727,#48728,#48729,
#48730,#48731,#48732,#48733,#48734,#48735,#48736,#48737,#48738,#48739,#48740,
#48741,#48742,#48743,#48744,#48745,#48746,#48747,#48748,#48749),
 .UNSPECIFIED.,.F.,.F.,(4,3,3,3,3,3,3,3,4),(-249.136768728842,-248.864222895099,
-247.864768184677,-246.865313474255,-245.865858763833,-244.866404053411,
-243.866949342989,-242.867494632567,-242.853583421662),.UNSPECIFIED.);
#1117=B_SPLINE_CURVE_WITH_KNOTS('',3,(#48750,#48751,#48752,#48753,#48754,
#48755,#48756,#48757,#48758,#48759,#48760,#48761,#48762,#48763,#48764,#48765,
#48766,#48767,#48768,#48769,#48770,#48771),.UNSPECIFIED.,.F.,.F.,(4,3,3,
3,3,3,3,4),(239.879896766363,240.816852802784,241.8165034693,242.816154135817,
243.815804802333,244.81545546885,245.815106135366,246.163082073543),
 .UNSPECIFIED.);
#1118=B_SPLINE_CURVE_WITH_KNOTS('',3,(#48776,#48777,#48778,#48779,#48780,
#48781,#48782,#48783,#48784,#48785,#48786,#48787,#48788,#48789,#48790,#48791,
#48792,#48793,#48794,#48795,#48796,#48797),.UNSPECIFIED.,.F.,.F.,(4,3,3,
3,3,3,3,4),(-255.419954036021,-254.860951157632,-253.86149644721,-252.862041736788,
-251.862587026365,-250.863132315943,-249.863677605521,-249.136768728842),
 .UNSPECIFIED.);
#1119=B_SPLINE_CURVE_WITH_KNOTS('',3,(#48798,#48799,#48800,#48801,#48802,
#48803,#48804,#48805,#48806,#48807,#48808,#48809,#48810,#48811,#48812,#48813,
#48814,#48815,#48816,#48817,#48818,#48819),.UNSPECIFIED.,.F.,.F.,(4,3,3,
3,3,3,3,4),(246.163082073543,246.814756801883,247.8144074684,248.814058134916,
249.813708801433,250.813359467949,251.813010134466,252.446267380722),
 .UNSPECIFIED.);
#1120=B_SPLINE_CURVE_WITH_KNOTS('',3,(#48824,#48825,#48826,#48827,#48828,
#48829,#48830,#48831,#48832,#48833,#48834,#48835,#48836,#48837,#48838,#48839,
#48840,#48841,#48842,#48843,#48844,#48845),.UNSPECIFIED.,.F.,.F.,(4,3,3,
3,3,3,3,4),(-261.703139343201,-260.857679420164,-259.858224709742,-258.85876999932,
-257.859315288898,-256.859860578476,-255.860405868054,-255.419954036021),
 .UNSPECIFIED.);
#1121=B_SPLINE_CURVE_WITH_KNOTS('',3,(#48846,#48847,#48848,#48849,#48850,
#48851,#48852,#48853,#48854,#48855,#48856,#48857,#48858,#48859,#48860,#48861,
#48862,#48863,#48864,#48865,#48866,#48867),.UNSPECIFIED.,.F.,.F.,(4,3,3,
3,3,3,3,4),(252.446267380722,252.812660800982,253.812311467499,254.811962134015,
255.811612800532,256.811263467048,257.810914133565,258.729452687902),
 .UNSPECIFIED.);
#1122=B_SPLINE_CURVE_WITH_KNOTS('',3,(#48872,#48873,#48874,#48875,#48876,
#48877,#48878,#48879,#48880,#48881,#48882,#48883,#48884,#48885,#48886,#48887,
#48888,#48889,#48890,#48891,#48892,#48893,#48894,#48895,#48896),
 .UNSPECIFIED.,.F.,.F.,(4,3,3,3,3,3,3,3,4),(-267.986324650381,-267.853862393119,
-266.854407682697,-265.854952972275,-264.855498261853,-263.85604355143,
-262.856588841008,-261.857134130586,-261.703139343201),.UNSPECIFIED.);
#1123=B_SPLINE_CURVE_WITH_KNOTS('',3,(#48897,#48898,#48899,#48900,#48901,
#48902,#48903,#48904,#48905,#48906,#48907,#48908,#48909,#48910,#48911,#48912,
#48913,#48914,#48915,#48916,#48917,#48918,#48919,#48920,#48921),
 .UNSPECIFIED.,.F.,.F.,(4,3,3,3,3,3,3,3,4),(258.729452687902,258.810564800082,
259.810215466598,260.809866133115,261.809516799631,262.809167466148,263.808818132664,
264.808468799181,265.012637995082),.UNSPECIFIED.);
#1124=B_SPLINE_CURVE_WITH_KNOTS('',3,(#48926,#48927,#48928,#48929,#48930,
#48931,#48932,#48933,#48934,#48935,#48936,#48937,#48938,#48939,#48940,#48941,
#48942,#48943,#48944,#48945,#48946,#48947),.UNSPECIFIED.,.F.,.F.,(4,3,3,
3,3,3,3,4),(-274.26950995756,-273.850590655651,-272.851135945229,-271.851681234807,
-270.852226524385,-269.852771813963,-268.853317103541,-267.986324650381),
 .UNSPECIFIED.);
#1125=B_SPLINE_CURVE_WITH_KNOTS('',3,(#48948,#48949,#48950,#48951,#48952,
#48953,#48954,#48955,#48956,#48957,#48958,#48959,#48960,#48961,#48962,#48963,
#48964,#48965,#48966,#48967,#48968,#48969),.UNSPECIFIED.,.F.,.F.,(4,3,3,
3,3,3,3,4),(265.012637995082,265.808119465698,266.807770132214,267.807420798731,
268.807071465247,269.806722131764,270.80637279828,271.295823302261),
 .UNSPECIFIED.);
#1126=B_SPLINE_CURVE_WITH_KNOTS('',3,(#48974,#48975,#48976,#48977,#48978,
#48979,#48980,#48981,#48982,#48983,#48984,#48985,#48986,#48987,#48988,#48989,
#48990,#48991,#48992,#48993,#48994,#48995),.UNSPECIFIED.,.F.,.F.,(4,3,3,
3,3,3,3,4),(-280.55269526474,-279.847318918184,-278.847864207762,-277.84840949734,
-276.848954786918,-275.849500076495,-274.850045366073,-274.26950995756),
 .UNSPECIFIED.);
#1127=B_SPLINE_CURVE_WITH_KNOTS('',3,(#48996,#48997,#48998,#48999,#49000,
#49001,#49002,#49003,#49004,#49005,#49006,#49007,#49008,#49009,#49010,#49011,
#49012,#49013,#49014,#49015,#49016,#49017),.UNSPECIFIED.,.F.,.F.,(4,3,3,
3,3,3,3,4),(271.295823302261,271.806023464797,272.805674131313,273.80532479783,
274.804975464346,275.804626130863,276.80427679738,277.579008609441),
 .UNSPECIFIED.);
#1128=B_SPLINE_CURVE_WITH_KNOTS('',3,(#49022,#49023,#49024,#49025,#49026,
#49027,#49028,#49029,#49030,#49031,#49032,#49033,#49034,#49035,#49036,#49037,
#49038,#49039,#49040,#49041,#49042,#49043),.UNSPECIFIED.,.F.,.F.,(4,3,3,
3,3,3,3,4),(-286.835880571919,-285.844047180716,-284.844592470294,-283.845137759872,
-282.84568304945,-281.846228339028,-280.846773628606,-280.55269526474),
 .UNSPECIFIED.);
#1129=B_SPLINE_CURVE_WITH_KNOTS('',3,(#49044,#49045,#49046,#49047,#49048,
#49049,#49050,#49051,#49052,#49053,#49054,#49055,#49056,#49057,#49058,#49059,
#49060,#49061,#49062,#49063,#49064,#49065,#49066,#49067,#49068),
 .UNSPECIFIED.,.F.,.F.,(4,3,3,3,3,3,3,3,4),(277.579008609441,277.803927463896,
278.803578130413,279.803228796929,280.802879463446,281.802530129962,282.802180796479,
283.801831462995,283.86219391662),.UNSPECIFIED.);
#1130=B_SPLINE_CURVE_WITH_KNOTS('',3,(#49073,#49074,#49075,#49076,#49077,
#49078,#49079,#49080,#49081,#49082,#49083,#49084,#49085,#49086,#49087,#49088,
#49089,#49090,#49091,#49092,#49093,#49094,#49095,#49096,#49097),
 .UNSPECIFIED.,.F.,.F.,(4,3,3,3,3,3,3,3,4),(-293.119065879099,-292.840230153671,
-291.840775443249,-290.841320732827,-289.841866022405,-288.842411311983,
-287.842956601561,-286.843501891138,-286.835880571919),.UNSPECIFIED.);
#1131=B_SPLINE_CURVE_WITH_KNOTS('',3,(#49098,#49099,#49100,#49101,#49102,
#49103,#49104,#49105,#49106,#49107,#49108,#49109,#49110,#49111,#49112,#49113,
#49114,#49115,#49116,#49117,#49118,#49119),.UNSPECIFIED.,.F.,.F.,(4,3,3,
3,3,3,3,4),(283.86219391662,284.801482129512,285.801132796029,286.800783462545,
287.800434129062,288.800084795578,289.799735462095,290.1453792238),
 .UNSPECIFIED.);
#1132=B_SPLINE_CURVE_WITH_KNOTS('',3,(#49124,#49125,#49126,#49127,#49128,
#49129,#49130,#49131,#49132,#49133,#49134,#49135,#49136,#49137,#49138,#49139,
#49140,#49141,#49142,#49143,#49144,#49145),.UNSPECIFIED.,.F.,.F.,(4,3,3,
3,3,3,3,4),(-299.402251186278,-298.836958416203,-297.837503705781,-296.838048995359,
-295.838594284937,-294.839139574515,-293.839684864093,-293.119065879099),
 .UNSPECIFIED.);
#1133=B_SPLINE_CURVE_WITH_KNOTS('',3,(#49146,#49147,#49148,#49149,#49150,
#49151,#49152,#49153,#49154,#49155,#49156,#49157,#49158,#49159,#49160,#49161,
#49162,#49163,#49164,#49165,#49166,#49167),.UNSPECIFIED.,.F.,.F.,(4,3,3,
3,3,3,3,4),(290.1453792238,290.799386128611,291.799036795128,292.798687461644,
293.798338128161,294.797988794677,295.797639461194,296.428564530979),
 .UNSPECIFIED.);
#1134=B_SPLINE_CURVE_WITH_KNOTS('',3,(#49172,#49173,#49174,#49175,#49176,
#49177,#49178,#49179,#49180,#49181,#49182,#49183,#49184,#49185,#49186,#49187,
#49188,#49189,#49190,#49191,#49192,#49193),.UNSPECIFIED.,.F.,.F.,(4,3,3,
3,3,3,3,4),(-305.685436493458,-304.833686678736,-303.834231968314,-302.834777257892,
-301.83532254747,-300.835867837048,-299.836413126626,-299.402251186278),
 .UNSPECIFIED.);
#1135=B_SPLINE_CURVE_WITH_KNOTS('',3,(#49194,#49195,#49196,#49197,#49198,
#49199,#49200,#49201,#49202,#49203,#49204,#49205,#49206,#49207,#49208,#49209,
#49210,#49211,#49212,#49213,#49214,#49215),.UNSPECIFIED.,.F.,.F.,(4,3,3,
3,3,3,3,4),(296.428564530979,296.797290127711,297.796940794227,298.796591460744,
299.79624212726,300.795892793777,301.795543460293,302.711749838159),
 .UNSPECIFIED.);
#1136=B_SPLINE_CURVE_WITH_KNOTS('',3,(#49220,#49221,#49222,#49223,#49224,
#49225,#49226,#49227,#49228,#49229,#49230,#49231,#49232,#49233,#49234,#49235,
#49236,#49237,#49238,#49239,#49240,#49241,#49242,#49243,#49244),
 .UNSPECIFIED.,.F.,.F.,(4,3,3,3,3,3,3,3,4),(-311.968621800638,-311.829869651691,
-310.830414941268,-309.830960230846,-308.831505520424,-307.832050810002,
-306.83259609958,-305.833141389158,-305.685436493458),.UNSPECIFIED.);
#1137=B_SPLINE_CURVE_WITH_KNOTS('',3,(#49245,#49246,#49247,#49248,#49249,
#49250,#49251,#49252,#49253,#49254,#49255,#49256,#49257,#49258,#49259,#49260,
#49261,#49262,#49263,#49264,#49265,#49266,#49267,#49268,#49269),
 .UNSPECIFIED.,.F.,.F.,(4,3,3,3,3,3,3,3,4),(302.711749838159,302.79519412681,
303.794844793326,304.794495459843,305.79414612636,306.793796792876,307.793447459393,
308.793098125909,308.994935145339),.UNSPECIFIED.);
#1138=B_SPLINE_CURVE_WITH_KNOTS('',3,(#49274,#49275,#49276,#49277,#49278,
#49279,#49280,#49281,#49282,#49283,#49284,#49285,#49286,#49287,#49288,#49289,
#49290,#49291,#49292,#49293,#49294,#49295),.UNSPECIFIED.,.F.,.F.,(4,3,3,
3,3,3,3,4),(-318.251807107817,-317.826597914223,-316.827143203801,-315.827688493379,
-314.828233782957,-313.828779072535,-312.829324362113,-311.968621800638),
 .UNSPECIFIED.);
#1139=B_SPLINE_CURVE_WITH_KNOTS('',3,(#49296,#49297,#49298,#49299,#49300,
#49301,#49302,#49303,#49304,#49305,#49306,#49307,#49308,#49309,#49310,#49311,
#49312,#49313,#49314,#49315,#49316,#49317),.UNSPECIFIED.,.F.,.F.,(4,3,3,
3,3,3,3,4),(308.994935145339,309.792748792426,310.792399458942,311.792050125459,
312.791700791975,313.791351458492,314.791002125009,315.278120452518),
 .UNSPECIFIED.);
#1140=B_SPLINE_CURVE_WITH_KNOTS('',3,(#49322,#49323,#49324,#49325,#49326,
#49327,#49328,#49329,#49330,#49331,#49332,#49333,#49334,#49335,#49336,#49337,
#49338,#49339,#49340,#49341,#49342,#49343),.UNSPECIFIED.,.F.,.F.,(4,3,3,
3,3,3,3,4),(-324.534992414997,-323.823326176756,-322.823871466334,-321.824416755911,
-320.824962045489,-319.825507335067,-318.826052624645,-318.251807107817),
 .UNSPECIFIED.);
#1141=B_SPLINE_CURVE_WITH_KNOTS('',3,(#49344,#49345,#49346,#49347,#49348,
#49349,#49350,#49351,#49352,#49353,#49354,#49355,#49356,#49357,#49358,#49359,
#49360,#49361,#49362,#49363,#49364,#49365),.UNSPECIFIED.,.F.,.F.,(4,3,3,
3,3,3,3,4),(315.278120452518,315.790652791525,316.790303458042,317.789954124558,
318.789604791075,319.789255457591,320.788906124108,321.561305759698),
 .UNSPECIFIED.);
#1142=B_SPLINE_CURVE_WITH_KNOTS('',3,(#49370,#49371,#49372,#49373,#49374,
#49375,#49376,#49377,#49378,#49379,#49380,#49381,#49382,#49383,#49384,#49385,
#49386,#49387,#49388,#49389,#49390,#49391),.UNSPECIFIED.,.F.,.F.,(4,3,3,
3,3,3,3,4),(-330.818177722176,-329.820054439288,-328.820599728866,-327.821145018444,
-326.821690308022,-325.8222355976,-324.822780887178,-324.534992414997),
 .UNSPECIFIED.);
#1143=B_SPLINE_CURVE_WITH_KNOTS('',3,(#49392,#49393,#49394,#49395,#49396,
#49397,#49398,#49399,#49400,#49401,#49402,#49403,#49404,#49405,#49406,#49407,
#49408,#49409,#49410,#49411,#49412,#49413,#49414,#49415,#49416),
 .UNSPECIFIED.,.F.,.F.,(4,3,3,3,3,3,3,3,4),(321.561305759698,321.788556790624,
322.788207457141,323.787858123657,324.787508790174,325.787159456691,326.786810123207,
327.786460789724,327.844491066877),.UNSPECIFIED.);
#1144=B_SPLINE_CURVE_WITH_KNOTS('',3,(#49421,#49422,#49423,#49424,#49425,
#49426,#49427,#49428,#49429,#49430,#49431,#49432,#49433,#49434,#49435,#49436,
#49437,#49438,#49439,#49440,#49441,#49442),.UNSPECIFIED.,.F.,.F.,(4,3,3,
3,3,3,3,4),(-337.101363029356,-336.816237412243,-335.816782701821,-334.817327991398,
-333.817873280976,-332.818418570554,-331.818963860132,-330.818177722176),
 .UNSPECIFIED.);
#1145=B_SPLINE_CURVE_WITH_KNOTS('',3,(#49443,#49444,#49445,#49446,#49447,
#49448,#49449,#49450,#49451,#49452,#49453,#49454,#49455,#49456,#49457,#49458,
#49459,#49460,#49461,#49462,#49463,#49464),.UNSPECIFIED.,.F.,.F.,(4,3,3,
3,3,3,3,4),(327.844491066877,328.78611145624,329.785762122757,330.785412789273,
331.78506345579,332.784714122306,333.784364788823,334.127676374057),
 .UNSPECIFIED.);
#1146=B_SPLINE_CURVE_WITH_KNOTS('',3,(#49469,#49470,#49471,#49472,#49473,
#49474,#49475,#49476,#49477,#49478,#49479,#49480,#49481,#49482,#49483,#49484,
#49485,#49486,#49487,#49488,#49489,#49490),.UNSPECIFIED.,.F.,.F.,(4,3,3,
3,3,3,3,4),(-343.384548336535,-342.812965674775,-341.813510964353,-340.814056253931,
-339.814601543509,-338.815146833087,-337.815692122665,-337.101363029356),
 .UNSPECIFIED.);
#1147=B_SPLINE_CURVE_WITH_KNOTS('',3,(#49491,#49492,#49493,#49494,#49495,
#49496,#49497,#49498,#49499,#49500,#49501,#49502,#49503,#49504,#49505,#49506,
#49507,#49508,#49509,#49510,#49511,#49512),.UNSPECIFIED.,.F.,.F.,(4,3,3,
3,3,3,3,4),(334.127676374057,334.784015455339,335.783666121856,336.783316788373,
337.782967454889,338.782618121406,339.782268787922,340.410861681236),
 .UNSPECIFIED.);
#1148=B_SPLINE_CURVE_WITH_KNOTS('',3,(#49517,#49518,#49519,#49520,#49521,
#49522,#49523,#49524,#49525,#49526,#49527,#49528,#49529,#49530,#49531,#49532,
#49533,#49534,#49535,#49536,#49537,#49538),.UNSPECIFIED.,.F.,.F.,(4,3,3,
3,3,3,3,4),(-349.667733643715,-348.809693937308,-347.810239226886,-346.810784516464,
-345.811329806041,-344.811875095619,-343.812420385197,-343.384548336535),
 .UNSPECIFIED.);
#1149=B_SPLINE_CURVE_WITH_KNOTS('',3,(#49539,#49540,#49541,#49542,#49543,
#49544,#49545,#49546,#49547,#49548,#49549,#49550,#49551,#49552,#49553,#49554,
#49555,#49556,#49557,#49558,#49559,#49560),.UNSPECIFIED.,.F.,.F.,(4,3,3,
3,3,3,3,4),(340.410861681236,340.781919454439,341.781570120955,342.781220787472,
343.780871453988,344.780522120505,345.780172787022,346.694046988416),
 .UNSPECIFIED.);
#1150=B_SPLINE_CURVE_WITH_KNOTS('',3,(#49565,#49566,#49567,#49568,#49569,
#49570,#49571,#49572,#49573,#49574,#49575,#49576,#49577,#49578,#49579,#49580,
#49581,#49582,#49583,#49584,#49585,#49586,#49587,#49588,#49589),
 .UNSPECIFIED.,.F.,.F.,(4,3,3,3,3,3,3,3,4),(-355.950918950894,-355.805876910262,
-354.80642219984,-353.806967489418,-352.807512778996,-351.808058068574,
-350.808603358152,-349.80914864773,-349.667733643715),.UNSPECIFIED.);
#1151=B_SPLINE_CURVE_WITH_KNOTS('',3,(#49590,#49591,#49592,#49593,#49594,
#49595,#49596,#49597,#49598,#49599,#49600,#49601,#49602,#49603,#49604,#49605,
#49606,#49607,#49608,#49609,#49610,#49611,#49612,#49613,#49614),
 .UNSPECIFIED.,.F.,.F.,(4,3,3,3,3,3,3,3,4),(346.694046988416,346.779823453538,
347.779474120055,348.779124786571,349.778775453088,350.778426119604,351.778076786121,
352.777727452637,352.977232295595),.UNSPECIFIED.);
#1152=B_SPLINE_CURVE_WITH_KNOTS('',3,(#49619,#49620,#49621,#49622,#49623,
#49624,#49625,#49626,#49627,#49628,#49629,#49630,#49631,#49632,#49633,#49634,
#49635,#49636,#49637,#49638,#49639,#49640),.UNSPECIFIED.,.F.,.F.,(4,3,3,
3,3,3,3,4),(-362.234104258074,-361.802605172795,-360.803150462373,-359.803695751951,
-358.804241041529,-357.804786331106,-356.805331620684,-355.950918950894),
 .UNSPECIFIED.);
#1153=B_SPLINE_CURVE_WITH_KNOTS('',3,(#49641,#49642,#49643,#49644,#49645,
#49646,#49647,#49648,#49649,#49650,#49651,#49652,#49653,#49654,#49655,#49656,
#49657,#49658,#49659,#49660,#49661,#49662),.UNSPECIFIED.,.F.,.F.,(4,3,3,
3,3,3,3,4),(352.977232295595,353.777378119154,354.777028785671,355.776679452187,
356.776330118704,357.77598078522,358.775631451737,359.260417602775),
 .UNSPECIFIED.);
#1154=B_SPLINE_CURVE_WITH_KNOTS('',3,(#49667,#49668,#49669,#49670,#49671,
#49672,#49673,#49674,#49675,#49676,#49677,#49678,#49679,#49680,#49681,#49682,
#49683,#49684,#49685,#49686,#49687,#49688),.UNSPECIFIED.,.F.,.F.,(4,3,3,
3,3,3,3,4),(-368.517289565254,-367.799333435327,-366.799878724905,-365.800424014483,
-364.800969304061,-363.801514593639,-362.802059883217,-362.234104258074),
 .UNSPECIFIED.);
#1155=B_SPLINE_CURVE_WITH_KNOTS('',3,(#49689,#49690,#49691,#49692,#49693,
#49694,#49695,#49696,#49697,#49698,#49699,#49700,#49701,#49702,#49703,#49704,
#49705,#49706,#49707,#49708,#49709,#49710),.UNSPECIFIED.,.F.,.F.,(4,3,3,
3,3,3,3,4),(359.260417602775,359.775282118253,360.77493278477,361.774583451286,
362.774234117803,363.77388478432,364.773535450836,365.543602909955),
 .UNSPECIFIED.);
#1156=B_SPLINE_CURVE_WITH_KNOTS('',3,(#49715,#49716,#49717,#49718,#49719,
#49720,#49721,#49722,#49723,#49724,#49725,#49726,#49727,#49728,#49729,#49730,
#49731,#49732,#49733,#49734,#49735,#49736,#49737,#49738,#49739),
 .UNSPECIFIED.,.F.,.F.,(4,3,3,3,3,3,3,3,4),(-374.800474872433,-374.795516408282,
-373.79606169786,-372.796606987438,-371.797152277016,-370.797697566594,
-369.798242856171,-368.798788145749,-368.517289565254),.UNSPECIFIED.);
#1157=B_SPLINE_CURVE_WITH_KNOTS('',3,(#49740,#49741,#49742,#49743,#49744,
#49745,#49746,#49747,#49748,#49749,#49750,#49751,#49752,#49753,#49754,#49755,
#49756,#49757,#49758,#49759,#49760,#49761,#49762,#49763,#49764),
 .UNSPECIFIED.,.F.,.F.,(4,3,3,3,3,3,3,3,4),(365.543602909955,365.773186117353,
366.772836783869,367.772487450386,368.772138116902,369.771788783419,370.771439449935,
371.771090116452,371.826788217134),.UNSPECIFIED.);
#1158=B_SPLINE_CURVE_WITH_KNOTS('',3,(#49769,#49770,#49771,#49772,#49773,
#49774,#49775,#49776,#49777,#49778,#49779,#49780,#49781,#49782,#49783,#49784,
#49785,#49786,#49787,#49788,#49789,#49790),.UNSPECIFIED.,.F.,.F.,(4,3,3,
3,3,3,3,4),(-381.083660179613,-380.792244670814,-379.792789960392,-378.79333524997,
-377.793880539548,-376.794425829126,-375.794971118704,-374.800474872433),
 .UNSPECIFIED.);
#1159=B_SPLINE_CURVE_WITH_KNOTS('',3,(#49791,#49792,#49793,#49794,#49795,
#49796,#49797,#49798,#49799,#49800,#49801,#49802,#49803,#49804,#49805,#49806,
#49807,#49808,#49809,#49810,#49811,#49812),.UNSPECIFIED.,.F.,.F.,(4,3,3,
3,3,3,3,4),(371.826788217134,372.770740782968,373.770391449485,374.770042116002,
375.769692782518,376.769343449035,377.768994115551,378.109973524314),
 .UNSPECIFIED.);
#1160=B_SPLINE_CURVE_WITH_KNOTS('',3,(#49817,#49818,#49819,#49820,#49821,
#49822,#49823,#49824,#49825,#49826,#49827,#49828,#49829,#49830,#49831,#49832,
#49833,#49834,#49835,#49836,#49837,#49838),.UNSPECIFIED.,.F.,.F.,(4,3,3,
3,3,3,3,4),(-387.366845486792,-386.788972933347,-385.789518222925,-384.790063512503,
-383.790608802081,-382.791154091659,-381.791699381237,-381.083660179613),
 .UNSPECIFIED.);
#1161=B_SPLINE_CURVE_WITH_KNOTS('',3,(#49839,#49840,#49841,#49842,#49843,
#49844,#49845,#49846,#49847,#49848,#49849,#49850,#49851,#49852,#49853,#49854,
#49855,#49856,#49857,#49858,#49859,#49860),.UNSPECIFIED.,.F.,.F.,(4,3,3,
3,3,3,3,4),(378.109973524314,378.768644782068,379.768295448584,380.767946115101,
381.767596781617,382.767247448134,383.76689811465,384.393158831493),
 .UNSPECIFIED.);
#1162=B_SPLINE_CURVE_WITH_KNOTS('',3,(#49865,#49866,#49867,#49868,#49869,
#49870,#49871,#49872,#49873,#49874,#49875,#49876,#49877,#49878,#49879,#49880,
#49881,#49882,#49883,#49884,#49885,#49886),.UNSPECIFIED.,.F.,.F.,(4,3,3,
3,3,3,3,4),(-393.650030793972,-392.785701195879,-391.786246485457,-390.786791775035,
-389.787337064613,-388.787882354191,-387.788427643769,-387.366845486792),
 .UNSPECIFIED.);
#1163=B_SPLINE_CURVE_WITH_KNOTS('',3,(#49887,#49888,#49889,#49890,#49891,
#49892,#49893,#49894,#49895,#49896,#49897,#49898,#49899,#49900,#49901,#49902,
#49903,#49904,#49905,#49906,#49907,#49908),.UNSPECIFIED.,.F.,.F.,(4,3,3,
3,3,3,3,4),(384.393158831493,384.766548781167,385.766199447684,386.7658501142,
387.765500780717,388.765151447233,389.76480211375,390.676344138673),
 .UNSPECIFIED.);
#1164=B_SPLINE_CURVE_WITH_KNOTS('',3,(#49913,#49914,#49915,#49916,#49917,
#49918,#49919,#49920,#49921,#49922,#49923,#49924,#49925,#49926,#49927,#49928,
#49929,#49930,#49931,#49932,#49933,#49934,#49935,#49936,#49937),
 .UNSPECIFIED.,.F.,.F.,(4,3,3,3,3,3,3,3,4),(-399.933216101151,-399.781884168834,
-398.782429458412,-397.78297474799,-396.783520037568,-395.784065327146,
-394.784610616724,-393.785155906302,-393.650030793972),.UNSPECIFIED.);
#1165=B_SPLINE_CURVE_WITH_KNOTS('',3,(#49938,#49939,#49940,#49941,#49942,
#49943,#49944,#49945,#49946,#49947,#49948,#49949,#49950,#49951,#49952,#49953,
#49954,#49955,#49956,#49957,#49958,#49959,#49960,#49961,#49962),
 .UNSPECIFIED.,.F.,.F.,(4,3,3,3,3,3,3,3,4),(390.676344138673,390.764452780266,
391.764103446783,392.763754113299,393.763404779816,394.763055446333,395.762706112849,
396.762356779366,396.959529445852),.UNSPECIFIED.);
#1166=B_SPLINE_CURVE_WITH_KNOTS('',3,(#49967,#49968,#49969,#49970,#49971,
#49972,#49973,#49974,#49975,#49976,#49977,#49978,#49979,#49980,#49981,#49982,
#49983,#49984,#49985,#49986,#49987,#49988),.UNSPECIFIED.,.F.,.F.,(4,3,3,
3,3,3,3,4),(-406.216401408331,-405.778612431367,-404.779157720944,-403.779703010522,
-402.7802483001,-401.780793589678,-400.781338879256,-399.933216101151),
 .UNSPECIFIED.);
#1167=B_SPLINE_CURVE_WITH_KNOTS('',3,(#49989,#49990,#49991,#49992,#49993,
#49994,#49995,#49996,#49997,#49998,#49999,#50000,#50001,#50002,#50003,#50004,
#50005,#50006,#50007,#50008,#50009,#50010),.UNSPECIFIED.,.F.,.F.,(4,3,3,
3,3,3,3,4),(396.959529445852,397.762007445882,398.761658112399,399.761308778915,
400.760959445432,401.760610111948,402.760260778465,403.242714753032),
 .UNSPECIFIED.);
#1168=B_SPLINE_CURVE_WITH_KNOTS('',3,(#50015,#50016,#50017,#50018,#50019,
#50020,#50021,#50022,#50023,#50024,#50025,#50026,#50027,#50028,#50029,#50030,
#50031,#50032,#50033,#50034,#50035,#50036),.UNSPECIFIED.,.F.,.F.,(4,3,3,
3,3,3,3,4),(-412.499586715511,-411.775340693899,-410.775885983477,-409.776431273055,
-408.776976562633,-407.777521852211,-406.778067141789,-406.216401408331),
 .UNSPECIFIED.);
#1169=B_SPLINE_CURVE_WITH_KNOTS('',3,(#50037,#50038,#50039,#50040,#50041,
#50042,#50043,#50044,#50045,#50046,#50047,#50048,#50049,#50050,#50051,#50052,
#50053,#50054,#50055,#50056,#50057,#50058),.UNSPECIFIED.,.F.,.F.,(4,3,3,
3,3,3,3,4),(403.242714753032,403.759911444982,404.759562111498,405.759212778015,
406.758863444531,407.758514111048,408.758164777564,409.525900060212),
 .UNSPECIFIED.);
#1170=B_SPLINE_CURVE_WITH_KNOTS('',3,(#50063,#50064,#50065,#50066,#50067,
#50068,#50069,#50070,#50071,#50072,#50073,#50074,#50075,#50076,#50077,#50078,
#50079,#50080,#50081,#50082,#50083,#50084,#50085,#50086,#50087),
 .UNSPECIFIED.,.F.,.F.,(4,3,3,3,3,3,3,3,4),(-418.78277202269,-418.771523666854,
-417.772068956432,-416.772614246009,-415.773159535587,-414.773704825165,
-413.774250114743,-412.774795404321,-412.499586715511),.UNSPECIFIED.);
#1171=B_SPLINE_CURVE_WITH_KNOTS('',3,(#50088,#50089,#50090,#50091,#50092,
#50093,#50094,#50095,#50096,#50097,#50098,#50099,#50100,#50101,#50102,#50103,
#50104,#50105,#50106,#50107,#50108,#50109,#50110,#50111,#50112),
 .UNSPECIFIED.,.F.,.F.,(4,3,3,3,3,3,3,3,4),(409.525900060212,409.757815444081,
410.757466110597,411.757116777114,412.756767443631,413.756418110147,414.756068776664,
415.75571944318,415.809085367391),.UNSPECIFIED.);
#1172=B_SPLINE_CURVE_WITH_KNOTS('',3,(#50117,#50118,#50119,#50120,#50121,
#50122,#50123,#50124,#50125,#50126,#50127,#50128,#50129,#50130,#50131,#50132,
#50133,#50134,#50135,#50136,#50137,#50138),.UNSPECIFIED.,.F.,.F.,(4,3,3,
3,3,3,3,4),(-425.06595732987,-424.768251929386,-423.768797218964,-422.769342508542,
-421.76988779812,-420.770433087698,-419.770978377276,-418.78277202269),
 .UNSPECIFIED.);
#1173=B_SPLINE_CURVE_WITH_KNOTS('',3,(#50139,#50140,#50141,#50142,#50143,
#50144,#50145,#50146,#50147,#50148,#50149,#50150,#50151,#50152,#50153,#50154,
#50155,#50156,#50157,#50158,#50159,#50160),.UNSPECIFIED.,.F.,.F.,(4,3,3,
3,3,3,3,4),(415.809085367391,416.755370109697,417.755020776213,418.75467144273,
419.754322109246,420.753972775763,421.753623442279,422.092270674571),
 .UNSPECIFIED.);
#1174=B_SPLINE_CURVE_WITH_KNOTS('',3,(#50165,#50166,#50167,#50168,#50169,
#50170,#50171,#50172,#50173,#50174,#50175,#50176,#50177,#50178,#50179,#50180,
#50181,#50182,#50183,#50184,#50185,#50186),.UNSPECIFIED.,.F.,.F.,(4,3,3,
3,3,3,3,4),(-431.349142637049,-430.764980191919,-429.765525481497,-428.766070771075,
-427.766616060652,-426.76716135023,-425.767706639808,-425.06595732987),
 .UNSPECIFIED.);
#1175=B_SPLINE_CURVE_WITH_KNOTS('',3,(#50187,#50188,#50189,#50190,#50191,
#50192,#50193,#50194,#50195,#50196,#50197,#50198,#50199,#50200,#50201,#50202,
#50203,#50204,#50205,#50206,#50207,#50208),.UNSPECIFIED.,.F.,.F.,(4,3,3,
3,3,3,3,4),(422.092270674571,422.753274108796,423.752924775313,424.752575441829,
425.752226108346,426.751876774862,427.751527441379,428.37545598175),
 .UNSPECIFIED.);
#1176=B_SPLINE_CURVE_WITH_KNOTS('',3,(#50213,#50214,#50215,#50216,#50217,
#50218,#50219,#50220,#50221,#50222,#50223,#50224,#50225,#50226,#50227,#50228,
#50229,#50230,#50231,#50232,#50233,#50234),.UNSPECIFIED.,.F.,.F.,(4,3,3,
3,3,3,3,4),(-437.632327944229,-436.761708454451,-435.762253744029,-434.762799033607,
-433.763344323185,-432.763889612763,-431.764434902341,-431.349142637049),
 .UNSPECIFIED.);
#1177=B_SPLINE_CURVE_WITH_KNOTS('',3,(#50235,#50236,#50237,#50238,#50239,
#50240,#50241,#50242,#50243,#50244,#50245,#50246,#50247,#50248,#50249,#50250,
#50251,#50252,#50253,#50254,#50255,#50256),.UNSPECIFIED.,.F.,.F.,(4,3,3,
3,3,3,3,4),(428.37545598175,428.751178107895,429.750828774412,430.750479440928,
431.750130107445,432.749780773961,433.749431440478,434.65864128893),
 .UNSPECIFIED.);
#1178=B_SPLINE_CURVE_WITH_KNOTS('',3,(#50261,#50262,#50263,#50264,#50265,
#50266,#50267,#50268,#50269,#50270,#50271,#50272,#50273,#50274,#50275,#50276,
#50277,#50278,#50279,#50280,#50281,#50282,#50283,#50284,#50285),
 .UNSPECIFIED.,.F.,.F.,(4,3,3,3,3,3,3,3,4),(-443.915513251408,-443.757891427406,
-442.758436716984,-441.758982006562,-440.75952729614,-439.760072585717,
-438.760617875295,-437.761163164873,-437.632327944229),.UNSPECIFIED.);
#1179=B_SPLINE_CURVE_WITH_KNOTS('',3,(#50286,#50287,#50288,#50289,#50290,
#50291,#50292,#50293,#50294,#50295,#50296,#50297,#50298,#50299,#50300,#50301,
#50302,#50303,#50304,#50305,#50306,#50307,#50308,#50309,#50310),
 .UNSPECIFIED.,.F.,.F.,(4,3,3,3,3,3,3,3,4),(434.65864128893,434.749082106995,
435.748732773511,436.748383440028,437.748034106544,438.747684773061,439.747335439577,
440.746986106094,440.941826596109),.UNSPECIFIED.);
#1180=B_SPLINE_CURVE_WITH_KNOTS('',3,(#50315,#50316,#50317,#50318,#50319,
#50320,#50321,#50322,#50323,#50324,#50325,#50326,#50327,#50328,#50329,#50330,
#50331,#50332,#50333,#50334,#50335,#50336),.UNSPECIFIED.,.F.,.F.,(4,3,3,
3,3,3,3,4),(-450.198698558588,-449.754619689938,-448.755164979516,-447.755710269094,
-446.756255558672,-445.75680084825,-444.757346137828,-443.915513251408),
 .UNSPECIFIED.);
#1181=B_SPLINE_CURVE_WITH_KNOTS('',3,(#50337,#50338,#50339,#50340,#50341,
#50342,#50343,#50344,#50345,#50346,#50347,#50348,#50349,#50350,#50351,#50352,
#50353,#50354,#50355,#50356,#50357,#50358),.UNSPECIFIED.,.F.,.F.,(4,3,3,
3,3,3,3,4),(440.941826596109,441.74663677261,442.746287439127,443.745938105644,
444.74558877216,445.745239438677,446.744890105193,447.225011903289),
 .UNSPECIFIED.);
#1182=B_SPLINE_CURVE_WITH_KNOTS('',3,(#50363,#50364,#50365,#50366,#50367,
#50368,#50369,#50370,#50371,#50372,#50373,#50374,#50375,#50376,#50377,#50378,
#50379,#50380,#50381,#50382,#50383,#50384),.UNSPECIFIED.,.F.,.F.,(4,3,3,
3,3,3,3,4),(-456.481883865768,-455.751347952471,-454.751893242049,-453.752438531627,
-452.752983821205,-451.753529110783,-450.75407440036,-450.198698558588),
 .UNSPECIFIED.);
#1183=B_SPLINE_CURVE_WITH_KNOTS('',3,(#50385,#50386,#50387,#50388,#50389,
#50390,#50391,#50392,#50393,#50394,#50395,#50396,#50397,#50398,#50399,#50400,
#50401,#50402,#50403,#50404,#50405,#50406),.UNSPECIFIED.,.F.,.F.,(4,3,3,
3,3,3,3,4),(447.225011903289,447.74454077171,448.744191438226,449.743842104743,
450.74349277126,451.743143437776,452.742794104293,453.508197210468),
 .UNSPECIFIED.);
#1184=B_SPLINE_CURVE_WITH_KNOTS('',3,(#50411,#50412,#50413,#50414,#50415,
#50416,#50417,#50418,#50419,#50420,#50421,#50422,#50423,#50424,#50425,#50426,
#50427,#50428,#50429,#50430,#50431,#50432,#50433,#50434,#50435),
 .UNSPECIFIED.,.F.,.F.,(4,3,3,3,3,3,3,3,4),(-462.765069172947,-462.747530925425,
-461.748076215003,-460.748621504581,-459.749166794159,-458.749712083737,
-457.750257373315,-456.750802662893,-456.481883865768),.UNSPECIFIED.);
#1185=B_SPLINE_CURVE_WITH_KNOTS('',3,(#50436,#50437,#50438,#50439,#50440,
#50441,#50442,#50443,#50444,#50445,#50446,#50447,#50448,#50449,#50450,#50451,
#50452,#50453,#50454,#50455,#50456,#50457,#50458,#50459,#50460),
 .UNSPECIFIED.,.F.,.F.,(4,3,3,3,3,3,3,3,4),(453.508197210468,453.742444770809,
454.742095437326,455.741746103842,456.741396770359,457.741047436875,458.740698103392,
459.740348769908,459.791382517648),.UNSPECIFIED.);
#1186=B_SPLINE_CURVE_WITH_KNOTS('',3,(#50465,#50466,#50467,#50468,#50469,
#50470,#50471,#50472,#50473,#50474,#50475,#50476,#50477,#50478,#50479,#50480,
#50481,#50482,#50483,#50484,#50485,#50486),.UNSPECIFIED.,.F.,.F.,(4,3,3,
3,3,3,3,4),(-469.048254480127,-468.744259187958,-467.744804477536,-466.745349767114,
-465.745895056692,-464.74644034627,-463.746985635847,-462.765069172947),
 .UNSPECIFIED.);
#1187=B_SPLINE_CURVE_WITH_KNOTS('',3,(#50487,#50488,#50489,#50490,#50491,
#50492,#50493,#50494,#50495,#50496,#50497,#50498,#50499,#50500,#50501,#50502,
#50503,#50504,#50505,#50506,#50507,#50508),.UNSPECIFIED.,.F.,.F.,(4,3,3,
3,3,3,3,4),(459.791382517648,460.739999436425,461.739650102942,462.739300769458,
463.738951435975,464.738602102491,465.738252769008,466.074567824828),
 .UNSPECIFIED.);
#1188=B_SPLINE_CURVE_WITH_KNOTS('',3,(#50513,#50514,#50515,#50516,#50517,
#50518,#50519,#50520,#50521,#50522,#50523,#50524,#50525,#50526,#50527,#50528,
#50529,#50530,#50531,#50532,#50533,#50534),.UNSPECIFIED.,.F.,.F.,(4,3,3,
3,3,3,3,4),(-475.331439787306,-474.74098745049,-473.741532740068,-472.742078029646,
-471.742623319224,-470.743168608802,-469.74371389838,-469.048254480127),
 .UNSPECIFIED.);
#1189=B_SPLINE_CURVE_WITH_KNOTS('',3,(#50535,#50536,#50537,#50538,#50539,
#50540,#50541,#50542,#50543,#50544,#50545,#50546,#50547,#50548,#50549,#50550,
#50551,#50552,#50553,#50554,#50555,#50556),.UNSPECIFIED.,.F.,.F.,(4,3,3,
3,3,3,3,4),(466.074567824828,466.737903435524,467.737554102041,468.737204768557,
469.736855435074,470.736506101591,471.736156768107,472.357753132007),
 .UNSPECIFIED.);
#1190=B_SPLINE_CURVE_WITH_KNOTS('',3,(#50561,#50562,#50563,#50564,#50565,
#50566,#50567,#50568,#50569,#50570,#50571,#50572,#50573,#50574,#50575,#50576,
#50577,#50578,#50579,#50580,#50581,#50582),.UNSPECIFIED.,.F.,.F.,(4,3,3,
3,3,3,3,4),(-481.614625094486,-480.737715713023,-479.738261002601,-478.738806292179,
-477.739351581757,-476.739896871335,-475.740442160912,-475.331439787306),
 .UNSPECIFIED.);
#1191=B_SPLINE_CURVE_WITH_KNOTS('',3,(#50583,#50584,#50585,#50586,#50587,
#50588,#50589,#50590,#50591,#50592,#50593,#50594,#50595,#50596,#50597,#50598,
#50599,#50600,#50601,#50602,#50603,#50604),.UNSPECIFIED.,.F.,.F.,(4,3,3,
3,3,3,3,4),(472.357753132007,472.735807434623,473.73545810114,474.735108767657,
475.734759434173,476.73441010069,477.734060767206,478.640938439187),
 .UNSPECIFIED.);
#1192=B_SPLINE_CURVE_WITH_KNOTS('',3,(#50609,#50610,#50611,#50612,#50613,
#50614,#50615,#50616,#50617,#50618,#50619,#50620,#50621,#50622,#50623,#50624,
#50625,#50626,#50627,#50628,#50629,#50630,#50631,#50632,#50633),
 .UNSPECIFIED.,.F.,.F.,(4,3,3,3,3,3,3,3,4),(-487.897810401665,-487.733898685978,
-486.734443975555,-485.734989265133,-484.735534554711,-483.736079844289,
-482.736625133867,-481.737170423445,-481.614625094486),.UNSPECIFIED.);
#1193=B_SPLINE_CURVE_WITH_KNOTS('',3,(#50634,#50635,#50636,#50637,#50638,
#50639,#50640,#50641,#50642,#50643,#50644,#50645,#50646,#50647,#50648,#50649,
#50650,#50651,#50652,#50653,#50654,#50655,#50656,#50657,#50658),
 .UNSPECIFIED.,.F.,.F.,(4,3,3,3,3,3,3,3,4),(478.640938439187,478.733711433723,
479.733362100239,480.733012766756,481.732663433272,482.732314099789,483.731964766306,
484.731615432822,484.924123746366),.UNSPECIFIED.);
#1194=B_SPLINE_CURVE_WITH_KNOTS('',3,(#50663,#50664,#50665,#50666,#50667,
#50668,#50669,#50670,#50671,#50672,#50673,#50674,#50675,#50676,#50677,#50678,
#50679,#50680,#50681,#50682,#50683,#50684),.UNSPECIFIED.,.F.,.F.,(4,3,3,
3,3,3,3,4),(-494.180995708845,-493.73062694851,-492.731172238088,-491.731717527666,
-490.732262817244,-489.732808106822,-488.7333533964,-487.897810401665),
 .UNSPECIFIED.);
#1195=B_SPLINE_CURVE_WITH_KNOTS('',3,(#50685,#50686,#50687,#50688,#50689,
#50690,#50691,#50692,#50693,#50694,#50695,#50696,#50697,#50698,#50699,#50700,
#50701,#50702,#50703,#50704,#50705,#50706),.UNSPECIFIED.,.F.,.F.,(4,3,3,
3,3,3,3,4),(484.924123746366,485.731266099339,486.730916765855,487.730567432372,
488.730218098888,489.729868765405,490.729519431921,491.207309053546),
 .UNSPECIFIED.);
#1196=B_SPLINE_CURVE_WITH_KNOTS('',3,(#50715,#50716,#50717,#50718,#50719,
#50720,#50721,#50722,#50723,#50724,#50725,#50726,#50727,#50728,#50729,#50730,
#50731,#50732,#50733),.UNSPECIFIED.,.F.,.F.,(4,3,3,3,3,3,4),(-504.724628763153,
-504.224901407942,-503.725174052731,-502.725719342309,-501.726264631887,
-500.726809921465,-500.464181016024),.UNSPECIFIED.);
#1197=B_SPLINE_CURVE_WITH_KNOTS('',3,(#50737,#50738,#50739,#50740,#50741,
#50742,#50743,#50744,#50745,#50746,#50747,#50748,#50749,#50750,#50751,#50752,
#50753,#50754,#50755),.UNSPECIFIED.,.F.,.F.,(4,3,3,3,3,3,4),(497.490494360725,
497.727074097537,498.726724764054,499.726375430571,500.726026097087,501.725676763604,
502.654824574367),.UNSPECIFIED.);
#1198=B_SPLINE_CURVE_WITH_KNOTS('',3,(#50762,#50763,#50764,#50765,#50766,
#50767,#50768,#50769,#50770,#50771),.UNSPECIFIED.,.F.,.F.,(4,3,3,4),(512.079602535136,
512.342231440576,513.341686150999,514.270246093479),.UNSPECIFIED.);
#1199=B_SPLINE_CURVE_WITH_KNOTS('',3,(#50774,#50775,#50776,#50777,#50778,
#50779,#50780),.UNSPECIFIED.,.F.,.F.,(4,3,4),(512.079602535136,512.530726297128,
513.030551630386),.UNSPECIFIED.);
#1200=B_SPLINE_CURVE_WITH_KNOTS('',3,(#50785,#50786,#50787,#50788,#50789,
#50790,#50791,#50792,#50793,#50794),.UNSPECIFIED.,.F.,.F.,(4,1,1,1,1,1,
1,4),(505.796417227957,506.345503178044,507.344957888466,508.344412598888,
509.34386730931,510.343322019732,511.342776730154,512.079602535136),
 .UNSPECIFIED.);
#1201=B_SPLINE_CURVE_WITH_KNOTS('',3,(#50795,#50796,#50797,#50798,#50799,
#50800,#50801,#50802,#50803,#50804,#50805),.UNSPECIFIED.,.F.,.F.,(4,1,1,
1,1,1,1,1,4),(505.796417227957,506.03299696477,507.032647631287,508.032298297803,
509.03194896432,510.031599630836,511.031250297353,512.030900963869,512.079602535136),
 .UNSPECIFIED.);
#1202=B_SPLINE_CURVE_WITH_KNOTS('',3,(#50810,#50811,#50812,#50813,#50814,
#50815,#50816,#50817,#50818,#50819),.UNSPECIFIED.,.F.,.F.,(4,1,1,1,1,1,
1,4),(499.513231920777,500.348774915511,501.348229625934,502.347684336356,
503.347139046778,504.3465937572,505.346048467622,505.796417227957),
 .UNSPECIFIED.);
#1203=B_SPLINE_CURVE_WITH_KNOTS('',3,(#50820,#50821,#50822,#50823,#50824,
#50825,#50826,#50827,#50828,#50829),.UNSPECIFIED.,.F.,.F.,(4,1,1,1,1,1,
1,4),(499.513231920777,500.035092965671,501.034743632187,502.034394298704,
503.03404496522,504.033695631737,505.033346298253,505.796417227957),
 .UNSPECIFIED.);
#1204=B_SPLINE_CURVE_WITH_KNOTS('',3,(#50834,#50835,#50836,#50837,#50838,
#50839,#50840,#50841,#50842,#50843,#50844),.UNSPECIFIED.,.F.,.F.,(4,1,1,
1,1,1,1,1,4),(493.230046613597,493.352591942557,494.352046652979,495.351501363401,
496.350956073823,497.350410784245,498.349865494667,499.349320205089,499.513231920777),
 .UNSPECIFIED.);
#1205=B_SPLINE_CURVE_WITH_KNOTS('',3,(#50845,#50846,#50847,#50848,#50849,
#50850,#50851,#50852,#50853,#50854),.UNSPECIFIED.,.F.,.F.,(4,1,1,1,1,1,
1,4),(493.230046613598,494.037188966571,495.036839633088,496.036490299605,
497.036140966121,498.035791632638,499.035442299154,499.513231920777),
 .UNSPECIFIED.);
#1206=B_SPLINE_CURVE_WITH_KNOTS('',3,(#50859,#50860,#50861,#50862,#50863,
#50864,#50865,#50866,#50867,#50868),.UNSPECIFIED.,.F.,.F.,(4,1,1,1,1,1,
1,4),(486.946861306418,487.355863680024,488.355318390446,489.354773100868,
490.354227811291,491.353682521713,492.353137232135,493.230046613597),
 .UNSPECIFIED.);
#1207=B_SPLINE_CURVE_WITH_KNOTS('',3,(#50869,#50870,#50871,#50872,#50873,
#50874,#50875,#50876,#50877,#50878,#50879),.UNSPECIFIED.,.F.,.F.,(4,1,1,
1,1,1,1,1,4),(486.946861306418,487.039634300956,488.039284967472,489.038935633989,
490.038586300505,491.038236967022,492.037887633538,493.037538300055,493.230046613598),
 .UNSPECIFIED.);
#1208=B_SPLINE_CURVE_WITH_KNOTS('',3,(#50884,#50885,#50886,#50887,#50888,
#50889,#50890,#50891,#50892,#50893),.UNSPECIFIED.,.F.,.F.,(4,1,1,1,1,1,
1,4),(480.663675999238,481.359135417492,482.358590127914,483.358044838336,
484.357499548758,485.35695425918,486.356408969602,486.946861306418),
 .UNSPECIFIED.);
#1209=B_SPLINE_CURVE_WITH_KNOTS('',3,(#50894,#50895,#50896,#50897,#50898,
#50899,#50900,#50901,#50902,#50903),.UNSPECIFIED.,.F.,.F.,(4,1,1,1,1,1,
1,4),(480.663675999238,481.041730301856,482.041380968373,483.041031634889,
484.040682301406,485.040332967922,486.039983634439,486.946861306418),
 .UNSPECIFIED.);
#1210=B_SPLINE_CURVE_WITH_KNOTS('',3,(#50908,#50909,#50910,#50911,#50912,
#50913,#50914,#50915,#50916,#50917),.UNSPECIFIED.,.F.,.F.,(4,1,1,1,1,1,
1,4),(474.380490692059,475.362407154959,476.361861865381,477.361316575803,
478.360771286226,479.360225996648,480.35968070707,480.663675999238),
 .UNSPECIFIED.);
#1211=B_SPLINE_CURVE_WITH_KNOTS('',3,(#50918,#50919,#50920,#50921,#50922,
#50923,#50924,#50925,#50926,#50927),.UNSPECIFIED.,.F.,.F.,(4,1,1,1,1,1,
1,4),(474.380490692059,475.043826302757,476.043476969273,477.04312763579,
478.042778302307,479.042428968823,480.04207963534,480.663675999238),
 .UNSPECIFIED.);
#1212=B_SPLINE_CURVE_WITH_KNOTS('',3,(#50932,#50933,#50934,#50935,#50936,
#50937,#50938,#50939,#50940,#50941,#50942),.UNSPECIFIED.,.F.,.F.,(4,1,1,
1,1,1,1,1,4),(468.097305384879,468.366224182005,469.365678892427,470.365133602849,
471.364588313271,472.364043023693,473.363497734115,474.362952444537,474.380490692059),
 .UNSPECIFIED.);
#1213=B_SPLINE_CURVE_WITH_KNOTS('',3,(#50943,#50944,#50945,#50946,#50947,
#50948,#50949,#50950,#50951,#50952),.UNSPECIFIED.,.F.,.F.,(4,1,1,1,1,1,
1,4),(468.097305384879,469.045922303658,470.045572970174,471.045223636691,
472.044874303207,473.044524969724,474.04417563624,474.380490692059),
 .UNSPECIFIED.);
#1214=B_SPLINE_CURVE_WITH_KNOTS('',3,(#50957,#50958,#50959,#50960,#50961,
#50962,#50963,#50964,#50965,#50966),.UNSPECIFIED.,.F.,.F.,(4,1,1,1,1,1,
1,4),(461.814120077699,462.369495919472,463.368950629894,464.368405340316,
465.367860050738,466.367314761161,467.366769471583,468.097305384879),
 .UNSPECIFIED.);
#1215=B_SPLINE_CURVE_WITH_KNOTS('',3,(#50967,#50968,#50969,#50970,#50971,
#50972,#50973,#50974,#50975,#50976,#50977),.UNSPECIFIED.,.F.,.F.,(4,1,1,
1,1,1,1,1,4),(461.8141200777,462.048367638042,463.048018304558,464.047668971075,
465.047319637591,466.046970304108,467.046620970625,468.046271637141,468.097305384879),
 .UNSPECIFIED.);
#1216=B_SPLINE_CURVE_WITH_KNOTS('',3,(#50982,#50983,#50984,#50985,#50986,
#50987,#50988,#50989,#50990,#50991),.UNSPECIFIED.,.F.,.F.,(4,1,1,1,1,1,
1,4),(455.53093477052,456.37276765694,457.372222367362,458.371677077784,
459.371131788206,460.370586498628,461.37004120905,461.814120077699),
 .UNSPECIFIED.);
#1217=B_SPLINE_CURVE_WITH_KNOTS('',3,(#50992,#50993,#50994,#50995,#50996,
#50997,#50998,#50999,#51000,#51001),.UNSPECIFIED.,.F.,.F.,(4,1,1,1,1,1,
1,4),(455.53093477052,456.050463638942,457.050114305459,458.049764971976,
459.049415638492,460.049066305009,461.048716971525,461.8141200777),
 .UNSPECIFIED.);
#1218=B_SPLINE_CURVE_WITH_KNOTS('',3,(#51006,#51007,#51008,#51009,#51010,
#51011,#51012,#51013,#51014,#51015,#51016),.UNSPECIFIED.,.F.,.F.,(4,1,1,
1,1,1,1,1,4),(449.24774946334,449.376584683985,450.376039394407,451.375494104829,
452.374948815251,453.374403525673,454.373858236095,455.373312946518,455.53093477052),
 .UNSPECIFIED.);
#1219=B_SPLINE_CURVE_WITH_KNOTS('',3,(#51017,#51018,#51019,#51020,#51021,
#51022,#51023,#51024,#51025,#51026),.UNSPECIFIED.,.F.,.F.,(4,1,1,1,1,1,
1,4),(449.247749463341,450.052559639843,451.05221030636,452.051860972876,
453.051511639393,454.051162305909,455.050812972426,455.53093477052),
 .UNSPECIFIED.);
#1220=B_SPLINE_CURVE_WITH_KNOTS('',3,(#51031,#51032,#51033,#51034,#51035,
#51036,#51037,#51038,#51039,#51040),.UNSPECIFIED.,.F.,.F.,(4,1,1,1,1,1,
1,4),(442.964564156161,443.379856421453,444.379311131875,445.378765842297,
446.378220552719,447.377675263141,448.377129973563,449.24774946334),
 .UNSPECIFIED.);
#1221=B_SPLINE_CURVE_WITH_KNOTS('',3,(#51041,#51042,#51043,#51044,#51045,
#51046,#51047,#51048,#51049,#51050,#51051),.UNSPECIFIED.,.F.,.F.,(4,1,1,
1,1,1,1,1,4),(442.964564156161,443.055004974227,444.054655640744,445.05430630726,
446.053956973777,447.053607640293,448.05325830681,449.052908973327,449.247749463341),
 .UNSPECIFIED.);
#1222=B_SPLINE_CURVE_WITH_KNOTS('',3,(#51056,#51057,#51058,#51059,#51060,
#51061,#51062,#51063,#51064,#51065),.UNSPECIFIED.,.F.,.F.,(4,1,1,1,1,1,
1,4),(436.681378848981,437.38312815892,438.382582869342,439.382037579764,
440.381492290186,441.380947000608,442.380401711031,442.964564156161),
 .UNSPECIFIED.);
#1223=B_SPLINE_CURVE_WITH_KNOTS('',3,(#51066,#51067,#51068,#51069,#51070,
#51071,#51072,#51073,#51074,#51075),.UNSPECIFIED.,.F.,.F.,(4,1,1,1,1,1,
1,4),(436.681378848981,437.057100975128,438.056751641645,439.056402308161,
440.056052974678,441.055703641194,442.055354307711,442.964564156161),
 .UNSPECIFIED.);
#1224=B_SPLINE_CURVE_WITH_KNOTS('',3,(#51080,#51081,#51082,#51083,#51084,
#51085,#51086,#51087,#51088,#51089),.UNSPECIFIED.,.F.,.F.,(4,1,1,1,1,1,
1,4),(430.398193541802,431.386399896388,432.38585460681,433.385309317232,
434.384764027654,435.384218738076,436.383673448498,436.681378848981),
 .UNSPECIFIED.);
#1225=B_SPLINE_CURVE_WITH_KNOTS('',3,(#51090,#51091,#51092,#51093,#51094,
#51095,#51096,#51097,#51098,#51099),.UNSPECIFIED.,.F.,.F.,(4,1,1,1,1,1,
1,4),(430.398193541802,431.059196976029,432.058847642545,433.058498309062,
434.058148975578,435.057799642095,436.057450308611,436.681378848981),
 .UNSPECIFIED.);
#1226=B_SPLINE_CURVE_WITH_KNOTS('',3,(#51104,#51105,#51106,#51107,#51108,
#51109,#51110,#51111,#51112,#51113,#51114),.UNSPECIFIED.,.F.,.F.,(4,1,1,
1,1,1,1,1,4),(424.115008234622,424.390216923433,425.389671633855,426.389126344277,
427.388581054699,428.388035765121,429.387490475543,430.386945185965,430.398193541802),
 .UNSPECIFIED.);
#1227=B_SPLINE_CURVE_WITH_KNOTS('',3,(#51115,#51116,#51117,#51118,#51119,
#51120,#51121,#51122,#51123,#51124),.UNSPECIFIED.,.F.,.F.,(4,1,1,1,1,1,
1,4),(424.115008234622,425.061292976929,426.060943643446,427.060594309962,
428.060244976479,429.059895642996,430.059546309512,430.398193541802),
 .UNSPECIFIED.);
#1228=B_SPLINE_CURVE_WITH_KNOTS('',3,(#51129,#51130,#51131,#51132,#51133,
#51134,#51135,#51136,#51137,#51138),.UNSPECIFIED.,.F.,.F.,(4,1,1,1,1,1,
1,4),(417.831822927443,418.3934886609,419.392943371323,420.392398081745,
421.391852792167,422.391307502589,423.390762213011,424.115008234622),
 .UNSPECIFIED.);
#1229=B_SPLINE_CURVE_WITH_KNOTS('',3,(#51139,#51140,#51141,#51142,#51143,
#51144,#51145,#51146,#51147,#51148,#51149),.UNSPECIFIED.,.F.,.F.,(4,1,1,
1,1,1,1,1,4),(417.831822927443,418.063738311314,419.06338897783,420.063039644347,
421.062690310863,422.06234097738,423.061991643896,424.061642310413,424.115008234622),
 .UNSPECIFIED.);
#1230=B_SPLINE_CURVE_WITH_KNOTS('',3,(#51154,#51155,#51156,#51157,#51158,
#51159,#51160,#51161,#51162,#51163),.UNSPECIFIED.,.F.,.F.,(4,1,1,1,1,1,
1,4),(411.548637620263,412.396760398368,413.39621510879,414.395669819212,
415.395124529634,416.394579240056,417.394033950478,417.831822927443),
 .UNSPECIFIED.);
#1231=B_SPLINE_CURVE_WITH_KNOTS('',3,(#51164,#51165,#51166,#51167,#51168,
#51169,#51170,#51171,#51172,#51173),.UNSPECIFIED.,.F.,.F.,(4,1,1,1,1,1,
1,4),(411.548637620263,412.065834312214,413.065484978731,414.065135645247,
415.064786311764,416.06443697828,417.064087644797,417.831822927443),
 .UNSPECIFIED.);
#1232=B_SPLINE_CURVE_WITH_KNOTS('',3,(#51178,#51179,#51180,#51181,#51182,
#51183,#51184,#51185,#51186,#51187,#51188),.UNSPECIFIED.,.F.,.F.,(4,1,1,
1,1,1,1,1,4),(405.265452313083,405.400577425413,406.400032135835,407.399486846258,
408.39894155668,409.398396267102,410.397850977524,411.397305687946,411.548637620263),
 .UNSPECIFIED.);
#1233=B_SPLINE_CURVE_WITH_KNOTS('',3,(#51189,#51190,#51191,#51192,#51193,
#51194,#51195,#51196,#51197,#51198),.UNSPECIFIED.,.F.,.F.,(4,1,1,1,1,1,
1,4),(405.265452313084,406.067930313115,407.067580979631,408.067231646148,
409.066882312665,410.066532979181,411.066183645698,411.548637620263),
 .UNSPECIFIED.);
#1234=B_SPLINE_CURVE_WITH_KNOTS('',3,(#51203,#51204,#51205,#51206,#51207,
#51208,#51209,#51210,#51211,#51212),.UNSPECIFIED.,.F.,.F.,(4,1,1,1,1,1,
1,4),(398.982267005904,399.403849162881,400.403303873303,401.402758583725,
402.402213294147,403.401668004569,404.401122714991,405.265452313083),
 .UNSPECIFIED.);
#1235=B_SPLINE_CURVE_WITH_KNOTS('',3,(#51213,#51214,#51215,#51216,#51217,
#51218,#51219,#51220,#51221,#51222,#51223),.UNSPECIFIED.,.F.,.F.,(4,1,1,
1,1,1,1,1,4),(398.982267005904,399.070375647499,400.070026314016,401.069676980532,
402.069327647049,403.068978313565,404.068628980082,405.068279646598,405.265452313084),
 .UNSPECIFIED.);
#1236=B_SPLINE_CURVE_WITH_KNOTS('',3,(#51228,#51229,#51230,#51231,#51232,
#51233,#51234,#51235,#51236,#51237),.UNSPECIFIED.,.F.,.F.,(4,1,1,1,1,1,
1,4),(392.699081698724,393.407120900348,394.40657561077,395.406030321192,
396.405485031615,397.404939742037,398.404394452459,398.982267005904),
 .UNSPECIFIED.);
#1237=B_SPLINE_CURVE_WITH_KNOTS('',3,(#51238,#51239,#51240,#51241,#51242,
#51243,#51244,#51245,#51246,#51247),.UNSPECIFIED.,.F.,.F.,(4,1,1,1,1,1,
1,4),(392.699081698725,393.0724716484,394.072122314916,395.071772981433,
396.071423647949,397.071074314466,398.070724980982,398.982267005904),
 .UNSPECIFIED.);
#1238=B_SPLINE_CURVE_WITH_KNOTS('',3,(#51252,#51253,#51254,#51255,#51256,
#51257,#51258,#51259,#51260,#51261),.UNSPECIFIED.,.F.,.F.,(4,1,1,1,1,1,
1,4),(386.415896391545,387.410392637816,388.409847348238,389.40930205866,
390.408756769082,391.408211479504,392.407666189926,392.699081698724),
 .UNSPECIFIED.);
#1239=B_SPLINE_CURVE_WITH_KNOTS('',3,(#51262,#51263,#51264,#51265,#51266,
#51267,#51268,#51269,#51270,#51271),.UNSPECIFIED.,.F.,.F.,(4,1,1,1,1,1,
1,4),(386.415896391545,387.0745676493,388.074218315817,389.073868982334,
390.07351964885,391.073170315367,392.072820981883,392.699081698725),
 .UNSPECIFIED.);
#1240=B_SPLINE_CURVE_WITH_KNOTS('',3,(#51276,#51277,#51278,#51279,#51280,
#51281,#51282,#51283,#51284,#51285,#51286),.UNSPECIFIED.,.F.,.F.,(4,1,1,
1,1,1,1,1,4),(380.132711084365,380.414209664861,381.413664375283,382.413119085705,
383.412573796127,384.41202850655,385.411483216972,386.410937927394,386.415896391545),
 .UNSPECIFIED.);
#1241=B_SPLINE_CURVE_WITH_KNOTS('',3,(#51287,#51288,#51289,#51290,#51291,
#51292,#51293,#51294,#51295,#51296),.UNSPECIFIED.,.F.,.F.,(4,1,1,1,1,1,
1,4),(380.132711084365,381.076663650201,382.076314316718,383.075964983234,
384.075615649751,385.075266316267,386.074916982784,386.415896391545),
 .UNSPECIFIED.);
#1242=B_SPLINE_CURVE_WITH_KNOTS('',3,(#51301,#51302,#51303,#51304,#51305,
#51306,#51307,#51308,#51309,#51310),.UNSPECIFIED.,.F.,.F.,(4,1,1,1,1,1,
1,4),(373.849525777186,374.417481402329,375.416936112751,376.416390823173,
377.415845533595,378.415300244017,379.414754954439,380.132711084365),
 .UNSPECIFIED.);
#1243=B_SPLINE_CURVE_WITH_KNOTS('',3,(#51311,#51312,#51313,#51314,#51315,
#51316,#51317,#51318,#51319,#51320,#51321),.UNSPECIFIED.,.F.,.F.,(4,1,1,
1,1,1,1,1,4),(373.849525777186,374.079108984585,375.078759651102,376.078410317618,
377.078060984135,378.077711650651,379.077362317168,380.077012983685,380.132711084365),
 .UNSPECIFIED.);
#1244=B_SPLINE_CURVE_WITH_KNOTS('',3,(#51326,#51327,#51328,#51329,#51330,
#51331,#51332,#51333,#51334,#51335),.UNSPECIFIED.,.F.,.F.,(4,1,1,1,1,1,
1,4),(367.566340470006,368.420753139796,369.420207850218,370.41966256064,
371.419117271062,372.418571981485,373.418026691907,373.849525777186),
 .UNSPECIFIED.);
#1245=B_SPLINE_CURVE_WITH_KNOTS('',3,(#51336,#51337,#51338,#51339,#51340,
#51341,#51342,#51343,#51344,#51345),.UNSPECIFIED.,.F.,.F.,(4,1,1,1,1,1,
1,4),(367.566340470006,368.081204985486,369.080855652002,370.080506318519,
371.080156985036,372.079807651552,373.079458318069,373.849525777186),
 .UNSPECIFIED.);
#1246=B_SPLINE_CURVE_WITH_KNOTS('',3,(#51350,#51351,#51352,#51353,#51354,
#51355,#51356,#51357,#51358,#51359,#51360),.UNSPECIFIED.,.F.,.F.,(4,1,1,
1,1,1,1,1,4),(361.283155162826,361.424570166842,362.424024877264,363.423479587686,
364.422934298108,365.42238900853,366.421843718952,367.421298429374,367.566340470006),
 .UNSPECIFIED.);
#1247=B_SPLINE_CURVE_WITH_KNOTS('',3,(#51361,#51362,#51363,#51364,#51365,
#51366,#51367,#51368,#51369,#51370),.UNSPECIFIED.,.F.,.F.,(4,1,1,1,1,1,
1,4),(361.283155162827,362.083300986387,363.082951652903,364.08260231942,
365.082252985936,366.081903652453,367.081554318969,367.566340470006),
 .UNSPECIFIED.);
#1248=B_SPLINE_CURVE_WITH_KNOTS('',3,(#51375,#51376,#51377,#51378,#51379,
#51380,#51381,#51382,#51383,#51384,#51385,#51386,#51387,#51388,#51389,#51390,
#51391,#51392,#51393,#51394,#51395,#51396),.UNSPECIFIED.,.F.,.F.,(4,3,3,
3,3,3,3,4),(354.999969855647,355.427841904309,356.427296614731,357.426751325153,
358.426206035575,359.425660745998,360.42511545642,361.283155162826),
 .UNSPECIFIED.);
#1249=B_SPLINE_CURVE_WITH_KNOTS('',3,(#51397,#51398,#51399,#51400,#51401,
#51402,#51403,#51404,#51405,#51406,#51407),.UNSPECIFIED.,.F.,.F.,(4,1,1,
1,1,1,1,1,4),(354.999969855647,355.085746320771,356.085396987287,357.085047653804,
358.08469832032,359.084348986837,360.083999653354,361.08365031987,361.283155162827),
 .UNSPECIFIED.);
#1250=B_SPLINE_CURVE_WITH_KNOTS('',3,(#51412,#51413,#51414,#51415,#51416,
#51417,#51418,#51419,#51420,#51421,#51422,#51423,#51424,#51425,#51426,#51427,
#51428,#51429,#51430,#51431,#51432,#51433),.UNSPECIFIED.,.F.,.F.,(4,3,3,
3,3,3,3,4),(348.716784548467,349.431113641777,350.430568352199,351.430023062621,
352.429477773043,353.428932483465,354.428387193887,354.999969855647),
 .UNSPECIFIED.);
#1251=B_SPLINE_CURVE_WITH_KNOTS('',3,(#51434,#51435,#51436,#51437,#51438,
#51439,#51440,#51441,#51442,#51443),.UNSPECIFIED.,.F.,.F.,(4,1,1,1,1,1,
1,4),(348.716784548468,349.087842321671,350.087492988188,351.087143654705,
352.086794321221,353.086444987738,354.086095654254,354.999969855647),
 .UNSPECIFIED.);
#1252=B_SPLINE_CURVE_WITH_KNOTS('',3,(#51448,#51449,#51450,#51451,#51452,
#51453,#51454,#51455,#51456,#51457,#51458),.UNSPECIFIED.,.F.,.F.,(4,1,1,
1,1,1,1,1,4),(342.433599241288,342.434930668822,343.434385379244,344.433840089666,
345.433294800088,346.43274951051,347.432204220932,348.431658931354,348.716784548467),
 .UNSPECIFIED.);
#1253=B_SPLINE_CURVE_WITH_KNOTS('',3,(#51459,#51460,#51461,#51462,#51463,
#51464,#51465,#51466,#51467,#51468),.UNSPECIFIED.,.F.,.F.,(4,1,1,1,1,1,
1,4),(342.433599241288,343.089938322572,344.089588989089,345.089239655605,
346.088890322122,347.088540988638,348.088191655155,348.716784548468),
 .UNSPECIFIED.);
#1254=B_SPLINE_CURVE_WITH_KNOTS('',3,(#51473,#51474,#51475,#51476,#51477,
#51478,#51479,#51480,#51481,#51482),.UNSPECIFIED.,.F.,.F.,(4,1,1,1,1,1,
1,4),(336.150413934108,336.438202406289,337.437657116712,338.437111827134,
339.436566537556,340.436021247978,341.4354759584,342.433599241288),
 .UNSPECIFIED.);
#1255=B_SPLINE_CURVE_WITH_KNOTS('',3,(#51483,#51484,#51485,#51486,#51487,
#51488,#51489,#51490,#51491,#51492),.UNSPECIFIED.,.F.,.F.,(4,1,1,1,1,1,
1,4),(336.150413934108,337.092034323473,338.091684989989,339.091335656506,
340.090986323022,341.090636989539,342.090287656056,342.433599241288),
 .UNSPECIFIED.);
#1256=B_SPLINE_CURVE_WITH_KNOTS('',3,(#51497,#51498,#51499,#51500,#51501,
#51502,#51503,#51504,#51505,#51506),.UNSPECIFIED.,.F.,.F.,(4,1,1,1,1,1,
1,4),(329.867228626929,330.441474143757,331.440928854179,332.440383564601,
333.439838275023,334.439292985445,335.438747695867,336.150413934108),
 .UNSPECIFIED.);
#1257=B_SPLINE_CURVE_WITH_KNOTS('',3,(#51507,#51508,#51509,#51510,#51511,
#51512,#51513,#51514,#51515,#51516,#51517),.UNSPECIFIED.,.F.,.F.,(4,1,1,
1,1,1,1,1,4),(329.867228626929,330.094479657857,331.094130324374,332.09378099089,
333.093431657407,334.093082323923,335.09273299044,336.092383656956,336.150413934108),
 .UNSPECIFIED.);
#1258=B_SPLINE_CURVE_WITH_KNOTS('',3,(#51522,#51523,#51524,#51525,#51526,
#51527,#51528,#51529,#51530,#51531),.UNSPECIFIED.,.F.,.F.,(4,1,1,1,1,1,
1,4),(323.584043319749,324.444745881224,325.444200591647,326.443655302069,
327.443110012491,328.442564722913,329.442019433335,329.867228626929),
 .UNSPECIFIED.);
#1259=B_SPLINE_CURVE_WITH_KNOTS('',3,(#51532,#51533,#51534,#51535,#51536,
#51537,#51538,#51539,#51540,#51541),.UNSPECIFIED.,.F.,.F.,(4,1,1,1,1,1,
1,4),(323.584043319749,324.096575658758,325.096226325274,326.095876991791,
327.095527658307,328.095178324824,329.09482899134,329.867228626929),
 .UNSPECIFIED.);
#1260=B_SPLINE_CURVE_WITH_KNOTS('',3,(#51546,#51547,#51548,#51549,#51550,
#51551,#51552,#51553,#51554,#51555,#51556),.UNSPECIFIED.,.F.,.F.,(4,1,1,
1,1,1,1,1,4),(317.300858012569,317.44856290827,318.448017618692,319.447472329114,
320.446927039536,321.446381749958,322.44583646038,323.445291170802,323.584043319749),
 .UNSPECIFIED.);
#1261=B_SPLINE_CURVE_WITH_KNOTS('',3,(#51557,#51558,#51559,#51560,#51561,
#51562,#51563,#51564,#51565,#51566),.UNSPECIFIED.,.F.,.F.,(4,1,1,1,1,1,
1,4),(317.30085801257,318.098671659658,319.098322326175,320.097972992691,
321.097623659208,322.097274325725,323.096924992241,323.584043319749),
 .UNSPECIFIED.);
#1262=B_SPLINE_CURVE_WITH_KNOTS('',3,(#51571,#51572,#51573,#51574,#51575,
#51576,#51577,#51578,#51579,#51580),.UNSPECIFIED.,.F.,.F.,(4,1,1,1,1,1,
1,4),(311.01767270539,311.451834645737,312.451289356159,313.450744066582,
314.450198777004,315.449653487426,316.449108197848,317.300858012569),
 .UNSPECIFIED.);
#1263=B_SPLINE_CURVE_WITH_KNOTS('',3,(#51581,#51582,#51583,#51584,#51585,
#51586,#51587,#51588,#51589,#51590,#51591),.UNSPECIFIED.,.F.,.F.,(4,1,1,
1,1,1,1,1,4),(311.01767270539,311.101116994043,312.100767660559,313.100418327076,
314.100068993592,315.099719660109,316.099370326625,317.099020993142,317.30085801257),
 .UNSPECIFIED.);
#1264=B_SPLINE_CURVE_WITH_KNOTS('',3,(#51596,#51597,#51598,#51599,#51600,
#51601,#51602,#51603,#51604,#51605),.UNSPECIFIED.,.F.,.F.,(4,1,1,1,1,1,
1,4),(304.73448739821,305.455106383205,306.454561093627,307.454015804049,
308.453470514471,309.452925224893,310.452379935315,311.01767270539),
 .UNSPECIFIED.);
#1265=B_SPLINE_CURVE_WITH_KNOTS('',3,(#51606,#51607,#51608,#51609,#51610,
#51611,#51612,#51613,#51614,#51615),.UNSPECIFIED.,.F.,.F.,(4,1,1,1,1,1,
1,4),(304.734487398211,305.103212994943,306.10286366146,307.102514327976,
308.102164994493,309.101815661009,310.101466327526,311.01767270539),
 .UNSPECIFIED.);
#1266=B_SPLINE_CURVE_WITH_KNOTS('',3,(#51620,#51621,#51622,#51623,#51624,
#51625,#51626,#51627,#51628,#51629,#51630),.UNSPECIFIED.,.F.,.F.,(4,1,1,
1,1,1,1,1,4),(298.451302091031,298.45892341025,299.458378120672,300.457832831094,
301.457287541517,302.456742251939,303.456196962361,304.455651672783,304.73448739821),
 .UNSPECIFIED.);
#1267=B_SPLINE_CURVE_WITH_KNOTS('',3,(#51631,#51632,#51633,#51634,#51635,
#51636,#51637,#51638,#51639,#51640),.UNSPECIFIED.,.F.,.F.,(4,1,1,1,1,1,
1,4),(298.451302091031,299.105308995844,300.10495966236,301.104610328877,
302.104260995394,303.10391166191,304.103562328427,304.734487398211),
 .UNSPECIFIED.);
#1268=B_SPLINE_CURVE_WITH_KNOTS('',3,(#51645,#51646,#51647,#51648,#51649,
#51650,#51651,#51652,#51653,#51654),.UNSPECIFIED.,.F.,.F.,(4,1,1,1,1,1,
1,4),(292.168116783851,292.462195147718,293.46164985814,294.461104568562,
295.460559278984,296.460013989406,297.459468699828,298.451302091031),
 .UNSPECIFIED.);
#1269=B_SPLINE_CURVE_WITH_KNOTS('',3,(#51655,#51656,#51657,#51658,#51659,
#51660,#51661,#51662,#51663,#51664),.UNSPECIFIED.,.F.,.F.,(4,1,1,1,1,1,
1,4),(292.168116783851,293.107404996745,294.107055663261,295.106706329778,
296.106356996294,297.106007662811,298.105658329327,298.451302091031),
 .UNSPECIFIED.);
#1270=B_SPLINE_CURVE_WITH_KNOTS('',3,(#51669,#51670,#51671,#51672,#51673,
#51674,#51675,#51676,#51677,#51678),.UNSPECIFIED.,.F.,.F.,(4,1,1,1,1,1,
1,4),(285.884931476672,286.465466885185,287.464921595607,288.464376306029,
289.463831016451,290.463285726874,291.462740437296,292.168116783851),
 .UNSPECIFIED.);
#1271=B_SPLINE_CURVE_WITH_KNOTS('',3,(#51679,#51680,#51681,#51682,#51683,
#51684,#51685,#51686,#51687,#51688,#51689),.UNSPECIFIED.,.F.,.F.,(4,1,1,
1,1,1,1,1,4),(285.884931476672,286.109850331129,287.109500997645,288.109151664162,
289.108802330678,290.108452997195,291.108103663712,292.107754330228,292.168116783851),
 .UNSPECIFIED.);
#1272=B_SPLINE_CURVE_WITH_KNOTS('',3,(#51694,#51695,#51696,#51697,#51698,
#51699,#51700,#51701,#51702,#51703),.UNSPECIFIED.,.F.,.F.,(4,1,1,1,1,1,
1,4),(279.601746169492,280.468738622653,281.468193333075,282.467648043497,
283.467102753919,284.466557464341,285.466012174763,285.884931476672),
 .UNSPECIFIED.);
#1273=B_SPLINE_CURVE_WITH_KNOTS('',3,(#51704,#51705,#51706,#51707,#51708,
#51709,#51710,#51711,#51712,#51713),.UNSPECIFIED.,.F.,.F.,(4,1,1,1,1,1,
1,4),(279.601746169492,280.111946332029,281.111596998546,282.111247665063,
283.110898331579,284.110548998096,285.110199664612,285.884931476672),
 .UNSPECIFIED.);
#1274=B_SPLINE_CURVE_WITH_KNOTS('',3,(#51718,#51719,#51720,#51721,#51722,
#51723,#51724,#51725,#51726,#51727,#51728),.UNSPECIFIED.,.F.,.F.,(4,1,1,
1,1,1,1,1,4),(273.318560862312,273.472555649698,274.47201036012,275.471465070542,
276.470919780964,277.470374491386,278.469829201809,279.469283912231,279.601746169492),
 .UNSPECIFIED.);
#1275=B_SPLINE_CURVE_WITH_KNOTS('',3,(#51729,#51730,#51731,#51732,#51733,
#51734,#51735,#51736,#51737,#51738),.UNSPECIFIED.,.F.,.F.,(4,1,1,1,1,1,
1,4),(273.318560862313,274.11404233293,275.113692999447,276.113343665963,
277.11299433248,278.112644998996,279.112295665513,279.601746169492),
 .UNSPECIFIED.);
#1276=B_SPLINE_CURVE_WITH_KNOTS('',3,(#51743,#51744,#51745,#51746,#51747,
#51748,#51749,#51750,#51751,#51752),.UNSPECIFIED.,.F.,.F.,(4,1,1,1,1,1,
1,4),(267.035375555133,267.475827387166,268.475282097588,269.47473680801,
270.474191518432,271.473646228854,272.473100939276,273.318560862312),
 .UNSPECIFIED.);
#1277=B_SPLINE_CURVE_WITH_KNOTS('',3,(#51753,#51754,#51755,#51756,#51757,
#51758,#51759,#51760,#51761,#51762,#51763),.UNSPECIFIED.,.F.,.F.,(4,1,1,
1,1,1,1,1,4),(267.035375555133,267.116487667314,268.116138333831,269.115789000347,
270.115439666864,271.11509033338,272.114740999897,273.114391666414,273.318560862313),
 .UNSPECIFIED.);
#1278=B_SPLINE_CURVE_WITH_KNOTS('',3,(#51768,#51769,#51770,#51771,#51772,
#51773,#51774,#51775,#51776,#51777),.UNSPECIFIED.,.F.,.F.,(4,1,1,1,1,1,
1,4),(260.752190247953,261.479099124633,262.478553835055,263.478008545477,
264.477463255899,265.476917966321,266.476372676744,267.035375555133),
 .UNSPECIFIED.);
#1279=B_SPLINE_CURVE_WITH_KNOTS('',3,(#51778,#51779,#51780,#51781,#51782,
#51783,#51784,#51785,#51786,#51787),.UNSPECIFIED.,.F.,.F.,(4,1,1,1,1,1,
1,4),(260.752190247954,261.118583668215,262.118234334731,263.117885001248,
264.117535667765,265.117186334281,266.116837000798,267.035375555133),
 .UNSPECIFIED.);
#1280=B_SPLINE_CURVE_WITH_KNOTS('',3,(#51792,#51793,#51794,#51795,#51796,
#51797,#51798,#51799,#51800,#51801,#51802),.UNSPECIFIED.,.F.,.F.,(4,1,1,
1,1,1,1,1,4),(254.469004940774,254.482916151679,255.482370862101,256.481825572523,
257.481280282945,258.480734993367,259.480189703789,260.479644414211,260.752190247953),
 .UNSPECIFIED.);
#1281=B_SPLINE_CURVE_WITH_KNOTS('',3,(#51803,#51804,#51805,#51806,#51807,
#51808,#51809,#51810,#51811,#51812),.UNSPECIFIED.,.F.,.F.,(4,1,1,1,1,1,
1,4),(254.469004940774,255.120679669116,256.120330335632,257.119981002149,
258.119631668665,259.119282335182,260.118933001698,260.752190247954),
 .UNSPECIFIED.);
#1282=B_SPLINE_CURVE_WITH_KNOTS('',3,(#51817,#51818,#51819,#51820,#51821,
#51822,#51823,#51824,#51825,#51826),.UNSPECIFIED.,.F.,.F.,(4,1,1,1,1,1,
1,4),(248.185819633594,248.486187889146,249.485642599568,250.48509730999,
251.484552020412,252.484006730834,253.483461441256,254.469004940774),
 .UNSPECIFIED.);
#1283=B_SPLINE_CURVE_WITH_KNOTS('',3,(#51827,#51828,#51829,#51830,#51831,
#51832,#51833,#51834,#51835,#51836),.UNSPECIFIED.,.F.,.F.,(4,1,1,1,1,1,
1,4),(248.185819633595,249.122775670016,250.122426336533,251.122077003049,
252.121727669566,253.121378336083,254.121029002599,254.469004940774),
 .UNSPECIFIED.);
#1284=B_SPLINE_CURVE_WITH_KNOTS('',3,(#51841,#51842,#51843,#51844,#51845,
#51846,#51847,#51848,#51849,#51850),.UNSPECIFIED.,.F.,.F.,(4,1,1,1,1,1,
1,4),(241.902634326415,242.489459626613,243.488914337036,244.488369047458,
245.48782375788,246.487278468302,247.486733178724,248.185819633594),
 .UNSPECIFIED.);
#1285=B_SPLINE_CURVE_WITH_KNOTS('',3,(#51851,#51852,#51853,#51854,#51855,
#51856,#51857,#51858,#51859,#51860,#51861),.UNSPECIFIED.,.F.,.F.,(4,1,1,
1,1,1,1,1,4),(241.902634326415,242.1252210044,243.124871670917,244.124522337434,
245.12417300395,246.123823670467,247.123474336983,248.1231250035,248.185819633595),
 .UNSPECIFIED.);
#1286=B_SPLINE_CURVE_WITH_KNOTS('',3,(#51866,#51867,#51868,#51869,#51870,
#51871,#51872,#51873,#51874,#51875),.UNSPECIFIED.,.F.,.F.,(4,1,1,1,1,1,
1,4),(235.619449019235,236.492731364081,237.492186074503,238.491640784925,
239.491095495347,240.490550205769,241.490004916191,241.902634326415),
 .UNSPECIFIED.);
#1287=B_SPLINE_CURVE_WITH_KNOTS('',3,(#51876,#51877,#51878,#51879,#51880,
#51881,#51882,#51883,#51884,#51885),.UNSPECIFIED.,.F.,.F.,(4,1,1,1,1,1,
1,4),(235.619449019235,236.127317005301,237.126967671818,238.126618338334,
239.126269004851,240.125919671367,241.125570337884,241.902634326415),
 .UNSPECIFIED.);
#1288=B_SPLINE_CURVE_WITH_KNOTS('',3,(#51890,#51891,#51892,#51893,#51894,
#51895,#51896,#51897,#51898,#51899,#51900),.UNSPECIFIED.,.F.,.F.,(4,1,1,
1,1,1,1,1,4),(229.336263712056,229.496548391126,230.496003101548,231.495457811971,
232.494912522393,233.494367232815,234.493821943237,235.493276653659,235.619449019235),
 .UNSPECIFIED.);
#1289=B_SPLINE_CURVE_WITH_KNOTS('',3,(#51901,#51902,#51903,#51904,#51905,
#51906,#51907,#51908,#51909,#51910),.UNSPECIFIED.,.F.,.F.,(4,1,1,1,1,1,
1,4),(229.336263712056,230.129413006202,231.129063672718,232.128714339235,
233.128365005752,234.128015672268,235.127666338785,235.619449019235),
 .UNSPECIFIED.);
#1290=B_SPLINE_CURVE_WITH_KNOTS('',3,(#51915,#51916,#51917,#51918,#51919,
#51920,#51921,#51922,#51923,#51924),.UNSPECIFIED.,.F.,.F.,(4,1,1,1,1,1,
1,4),(223.053078404876,223.499820128594,224.499274839016,225.498729549438,
226.49818425986,227.497638970282,228.497093680704,229.336263712056),
 .UNSPECIFIED.);
#1291=B_SPLINE_CURVE_WITH_KNOTS('',3,(#51925,#51926,#51927,#51928,#51929,
#51930,#51931,#51932,#51933,#51934,#51935),.UNSPECIFIED.,.F.,.F.,(4,1,1,
1,1,1,1,1,4),(223.053078404876,223.131858340586,224.131509007103,225.131159673619,
226.130810340136,227.130461006652,228.130111673169,229.129762339685,229.336263712056),
 .UNSPECIFIED.);
#1292=B_SPLINE_CURVE_WITH_KNOTS('',3,(#51940,#51941,#51942,#51943,#51944,
#51945,#51946,#51947,#51948,#51949),.UNSPECIFIED.,.F.,.F.,(4,1,1,1,1,1,
1,4),(216.769893097696,217.503091866061,218.502546576483,219.502001286906,
220.501455997328,221.50091070775,222.500365418172,223.053078404876),
 .UNSPECIFIED.);
#1293=B_SPLINE_CURVE_WITH_KNOTS('',3,(#51950,#51951,#51952,#51953,#51954,
#51955,#51956,#51957,#51958,#51959),.UNSPECIFIED.,.F.,.F.,(4,1,1,1,1,1,
1,4),(216.769893097697,217.133954341487,218.133605008003,219.13325567452,
220.132906341036,221.132557007553,222.132207674069,223.053078404876),
 .UNSPECIFIED.);
#1294=B_SPLINE_CURVE_WITH_KNOTS('',3,(#51964,#51965,#51966,#51967,#51968,
#51969,#51970,#51971,#51972,#51973,#51974),.UNSPECIFIED.,.F.,.F.,(4,1,1,
1,1,1,1,1,4),(210.486707790517,210.506908893107,211.506363603529,212.505818313951,
213.505273024373,214.504727734795,215.504182445217,216.503637155639,216.769893097696),
 .UNSPECIFIED.);
#1295=B_SPLINE_CURVE_WITH_KNOTS('',3,(#51975,#51976,#51977,#51978,#51979,
#51980,#51981,#51982,#51983,#51984),.UNSPECIFIED.,.F.,.F.,(4,1,1,1,1,1,
1,4),(210.486707790517,211.136050342387,212.135701008904,213.135351675421,
214.135002341937,215.134653008454,216.13430367497,216.769893097697),
 .UNSPECIFIED.);
#1296=B_SPLINE_CURVE_WITH_KNOTS('',3,(#51989,#51990,#51991,#51992,#51993,
#51994,#51995,#51996,#51997,#51998),.UNSPECIFIED.,.F.,.F.,(4,1,1,1,1,1,
1,4),(204.203522483337,204.510180630574,205.509635340996,206.509090051418,
207.508544761841,208.507999472263,209.507454182685,210.486707790517),
 .UNSPECIFIED.);
#1297=B_SPLINE_CURVE_WITH_KNOTS('',3,(#51999,#52000,#52001,#52002,#52003,
#52004,#52005,#52006,#52007,#52008),.UNSPECIFIED.,.F.,.F.,(4,1,1,1,1,1,
1,4),(204.203522483338,205.138146343288,206.137797009805,207.137447676321,
208.137098342838,209.136749009354,210.136399675871,210.486707790517),
 .UNSPECIFIED.);
#1298=B_SPLINE_CURVE_WITH_KNOTS('',3,(#52013,#52014,#52015,#52016,#52017,
#52018,#52019,#52020,#52021,#52022),.UNSPECIFIED.,.F.,.F.,(4,1,1,1,1,1,
1,4),(197.920337176158,198.513452368042,199.512907078464,200.512361788886,
201.511816499308,202.51127120973,203.510725920152,204.203522483337),
 .UNSPECIFIED.);
#1299=B_SPLINE_CURVE_WITH_KNOTS('',3,(#52023,#52024,#52025,#52026,#52027,
#52028,#52029,#52030,#52031,#52032,#52033),.UNSPECIFIED.,.F.,.F.,(4,1,1,
1,1,1,1,1,4),(197.920337176158,198.140591677672,199.140242344189,200.139893010705,
201.139543677222,202.139194343738,203.138845010255,204.138495676772,204.203522483338),
 .UNSPECIFIED.);
#1300=B_SPLINE_CURVE_WITH_KNOTS('',3,(#52038,#52039,#52040,#52041,#52042,
#52043,#52044,#52045,#52046,#52047),.UNSPECIFIED.,.F.,.F.,(4,1,1,1,1,1,
1,4),(191.637151868978,192.516724105509,193.516178815931,194.515633526353,
195.515088236775,196.514542947198,197.51399765762,197.920337176158),
 .UNSPECIFIED.);
#1301=B_SPLINE_CURVE_WITH_KNOTS('',3,(#52048,#52049,#52050,#52051,#52052,
#52053,#52054,#52055,#52056,#52057),.UNSPECIFIED.,.F.,.F.,(4,1,1,1,1,1,
1,4),(191.637151868978,192.142687678573,193.142338345089,194.141989011606,
195.141639678123,196.141290344639,197.140941011156,197.920337176158),
 .UNSPECIFIED.);
#1302=B_SPLINE_CURVE_WITH_KNOTS('',3,(#52062,#52063,#52064,#52065,#52066,
#52067,#52068,#52069,#52070,#52071,#52072),.UNSPECIFIED.,.F.,.F.,(4,1,1,
1,1,1,1,1,4),(185.353966561799,185.520541132555,186.519995842977,187.519450553399,
188.518905263821,189.518359974243,190.517814684665,191.517269395087,191.637151868978),
 .UNSPECIFIED.);
#1303=B_SPLINE_CURVE_WITH_KNOTS('',3,(#52073,#52074,#52075,#52076,#52077,
#52078,#52079,#52080,#52081,#52082),.UNSPECIFIED.,.F.,.F.,(4,1,1,1,1,1,
1,4),(185.353966561799,186.144783679474,187.14443434599,188.144085012507,
189.143735679023,190.14338634554,191.143037012056,191.637151868978),
 .UNSPECIFIED.);
#1304=B_SPLINE_CURVE_WITH_KNOTS('',3,(#52087,#52088,#52089,#52090,#52091,
#52092,#52093,#52094,#52095,#52096),.UNSPECIFIED.,.F.,.F.,(4,1,1,1,1,1,
1,4),(179.070781254619,179.523812870022,180.523267580444,181.522722290866,
182.522177001288,183.52163171171,184.521086422133,185.353966561799),
 .UNSPECIFIED.);
#1305=B_SPLINE_CURVE_WITH_KNOTS('',3,(#52097,#52098,#52099,#52100,#52101,
#52102,#52103,#52104,#52105,#52106,#52107),.UNSPECIFIED.,.F.,.F.,(4,1,1,
1,1,1,1,1,4),(179.070781254619,179.147229013858,180.146879680374,181.146530346891,
182.146181013407,183.145831679924,184.145482346441,185.145133012957,185.353966561799),
 .UNSPECIFIED.);
#1306=B_SPLINE_CURVE_WITH_KNOTS('',3,(#52112,#52113,#52114,#52115,#52116,
#52117,#52118,#52119,#52120,#52121),.UNSPECIFIED.,.F.,.F.,(4,1,1,1,1,1,
1,4),(172.787595947439,173.52708460749,174.526539317912,175.525994028334,
176.525448738756,177.524903449178,178.5243581596,179.070781254619),
 .UNSPECIFIED.);
#1307=B_SPLINE_CURVE_WITH_KNOTS('',3,(#52122,#52123,#52124,#52125,#52126,
#52127,#52128,#52129,#52130,#52131),.UNSPECIFIED.,.F.,.F.,(4,1,1,1,1,1,
1,4),(172.78759594744,173.149325014758,174.148975681275,175.148626347792,
176.148277014308,177.147927680825,178.147578347341,179.070781254619),
 .UNSPECIFIED.);
#1308=B_SPLINE_CURVE_WITH_KNOTS('',3,(#52136,#52137,#52138,#52139,#52140,
#52141,#52142,#52143,#52144,#52145,#52146),.UNSPECIFIED.,.F.,.F.,(4,1,1,
1,1,1,1,1,4),(166.50441064026,166.530901634535,167.530356344957,168.529811055379,
169.529265765801,170.528720476223,171.528175186645,172.527629897068,172.787595947439),
 .UNSPECIFIED.);
#1309=B_SPLINE_CURVE_WITH_KNOTS('',3,(#52147,#52148,#52149,#52150,#52151,
#52152,#52153,#52154,#52155,#52156),.UNSPECIFIED.,.F.,.F.,(4,1,1,1,1,1,
1,4),(166.50441064026,167.151421015659,168.151071682176,169.150722348692,
170.150373015209,171.150023681725,172.149674348242,172.78759594744),
 .UNSPECIFIED.);
#1310=B_SPLINE_CURVE_WITH_KNOTS('',3,(#52161,#52162,#52163,#52164,#52165,
#52166,#52167,#52168,#52169,#52170),.UNSPECIFIED.,.F.,.F.,(4,1,1,1,1,1,
1,4),(160.22122533308,160.534173372003,161.533628082425,162.533082792847,
163.532537503269,164.531992213691,165.531446924113,166.50441064026),
 .UNSPECIFIED.);
#1311=B_SPLINE_CURVE_WITH_KNOTS('',3,(#52171,#52172,#52173,#52174,#52175,
#52176,#52177,#52178,#52179,#52180),.UNSPECIFIED.,.F.,.F.,(4,1,1,1,1,1,
1,4),(160.221225333081,161.15351701656,162.153167683076,163.152818349593,
164.152469016109,165.152119682626,166.151770349143,166.50441064026),
 .UNSPECIFIED.);
#1312=B_SPLINE_CURVE_WITH_KNOTS('',3,(#52185,#52186,#52187,#52188,#52189,
#52190,#52191,#52192,#52193,#52194),.UNSPECIFIED.,.F.,.F.,(4,1,1,1,1,1,
1,4),(153.938040025901,154.53744510947,155.536899819892,156.536354530314,
157.535809240736,158.535263951158,159.53471866158,160.22122533308),
 .UNSPECIFIED.);
#1313=B_SPLINE_CURVE_WITH_KNOTS('',3,(#52195,#52196,#52197,#52198,#52199,
#52200,#52201,#52202,#52203,#52204,#52205),.UNSPECIFIED.,.F.,.F.,(4,1,1,
1,1,1,1,1,4),(153.938040025901,154.155962350944,155.155613017461,156.155263683977,
157.154914350494,158.15456501701,159.154215683527,160.153866350043,160.221225333081),
 .UNSPECIFIED.);
#1314=B_SPLINE_CURVE_WITH_KNOTS('',3,(#52210,#52211,#52212,#52213,#52214,
#52215,#52216,#52217,#52218,#52219),.UNSPECIFIED.,.F.,.F.,(4,1,1,1,1,1,
1,4),(147.654854718721,148.540716846937,149.54017155736,150.539626267782,
151.539080978204,152.538535688626,153.537990399048,153.938040025901),
 .UNSPECIFIED.);
#1315=B_SPLINE_CURVE_WITH_KNOTS('',3,(#52220,#52221,#52222,#52223,#52224,
#52225,#52226,#52227,#52228,#52229),.UNSPECIFIED.,.F.,.F.,(4,1,1,1,1,1,
1,4),(147.654854718721,148.158058351845,149.157709018361,150.157359684878,
151.157010351394,152.156661017911,153.156311684427,153.938040025901),
 .UNSPECIFIED.);
#1316=B_SPLINE_CURVE_WITH_KNOTS('',3,(#52234,#52235,#52236,#52237,#52238,
#52239,#52240,#52241,#52242,#52243,#52244),.UNSPECIFIED.,.F.,.F.,(4,1,1,
1,1,1,1,1,4),(141.371669411542,141.544533873983,142.543988584405,143.543443294827,
144.542898005249,145.542352715671,146.541807426093,147.541262136515,147.654854718721),
 .UNSPECIFIED.);
#1317=B_SPLINE_CURVE_WITH_KNOTS('',3,(#52245,#52246,#52247,#52248,#52249,
#52250,#52251,#52252,#52253,#52254),.UNSPECIFIED.,.F.,.F.,(4,1,1,1,1,1,
1,4),(141.371669411542,142.160154352745,143.159805019262,144.159455685778,
145.159106352295,146.158757018812,147.158407685328,147.654854718721),
 .UNSPECIFIED.);
#1318=B_SPLINE_CURVE_WITH_KNOTS('',3,(#52259,#52260,#52261,#52262,#52263,
#52264,#52265,#52266,#52267,#52268),.UNSPECIFIED.,.F.,.F.,(4,1,1,1,1,1,
1,4),(135.088484104362,135.54780561145,136.547260321872,137.546715032295,
138.546169742717,139.545624453139,140.545079163561,141.371669411542),
 .UNSPECIFIED.);
#1319=B_SPLINE_CURVE_WITH_KNOTS('',3,(#52269,#52270,#52271,#52272,#52273,
#52274,#52275,#52276,#52277,#52278,#52279),.UNSPECIFIED.,.F.,.F.,(4,1,1,
1,1,1,1,1,4),(135.088484104362,135.16259968713,136.162250353646,137.161901020163,
138.161551686679,139.161202353196,140.160853019712,141.160503686229,141.371669411542),
 .UNSPECIFIED.);
#1320=B_SPLINE_CURVE_WITH_KNOTS('',3,(#52284,#52285,#52286,#52287,#52288,
#52289,#52290,#52291,#52292,#52293),.UNSPECIFIED.,.F.,.F.,(4,1,1,1,1,1,
1,4),(128.805298797183,129.551077348918,130.55053205934,131.549986769762,
132.549441480184,133.548896190606,134.548350901028,135.088484104362),
 .UNSPECIFIED.);
#1321=B_SPLINE_CURVE_WITH_KNOTS('',3,(#52294,#52295,#52296,#52297,#52298,
#52299,#52300,#52301,#52302,#52303),.UNSPECIFIED.,.F.,.F.,(4,1,1,1,1,1,
1,4),(128.805298797183,129.16469568803,130.164346354547,131.163997021063,
132.16364768758,133.163298354096,134.162949020613,135.088484104362),
 .UNSPECIFIED.);
#1322=B_SPLINE_CURVE_WITH_KNOTS('',3,(#52308,#52309,#52310,#52311,#52312,
#52313,#52314,#52315,#52316,#52317,#52318),.UNSPECIFIED.,.F.,.F.,(4,1,1,
1,1,1,1,1,4),(122.522113490003,122.554894375963,123.554349086385,124.553803796807,
125.55325850723,126.552713217652,127.552167928074,128.551622638496,128.805298797183),
 .UNSPECIFIED.);
#1323=B_SPLINE_CURVE_WITH_KNOTS('',3,(#52319,#52320,#52321,#52322,#52323,
#52324,#52325,#52326,#52327,#52328),.UNSPECIFIED.,.F.,.F.,(4,1,1,1,1,1,
1,4),(122.522113490003,123.166791688931,124.166442355447,125.166093021964,
126.165743688481,127.165394354997,128.165045021514,128.805298797183),
 .UNSPECIFIED.);
#1324=B_SPLINE_CURVE_WITH_KNOTS('',3,(#52333,#52334,#52335,#52336,#52337,
#52338,#52339,#52340,#52341,#52342),.UNSPECIFIED.,.F.,.F.,(4,1,1,1,1,1,
1,4),(116.238928182823,116.558166113431,117.557620823853,118.557075534275,
119.556530244697,120.555984955119,121.555439665541,122.522113490003),
 .UNSPECIFIED.);
#1325=B_SPLINE_CURVE_WITH_KNOTS('',3,(#52343,#52344,#52345,#52346,#52347,
#52348,#52349,#52350,#52351,#52352),.UNSPECIFIED.,.F.,.F.,(4,1,1,1,1,1,
1,4),(116.238928182824,117.168887689832,118.168538356348,119.168189022865,
120.167839689381,121.167490355898,122.167141022414,122.522113490003),
 .UNSPECIFIED.);
#1326=B_SPLINE_CURVE_WITH_KNOTS('',3,(#52357,#52358,#52359,#52360,#52361,
#52362,#52363,#52364,#52365,#52366),.UNSPECIFIED.,.F.,.F.,(4,1,1,1,1,1,
1,4),(109.955742875644,110.561437850898,111.56089256132,112.560347271742,
113.559801982165,114.559256692587,115.558711403009,116.238928182823),
 .UNSPECIFIED.);
#1327=B_SPLINE_CURVE_WITH_KNOTS('',3,(#52367,#52368,#52369,#52370,#52371,
#52372,#52373,#52374,#52375,#52376,#52377),.UNSPECIFIED.,.F.,.F.,(4,1,1,
1,1,1,1,1,4),(109.955742875644,110.171333024216,111.170983690732,112.170634357249,
113.170285023765,114.169935690282,115.169586356798,116.169237023315,116.238928182824),
 .UNSPECIFIED.);
#1328=B_SPLINE_CURVE_WITH_KNOTS('',3,(#52382,#52383,#52384,#52385,#52386,
#52387,#52388,#52389,#52390,#52391),.UNSPECIFIED.,.F.,.F.,(4,1,1,1,1,1,
1,4),(103.672557568464,104.564709588366,105.564164298788,106.56361900921,
107.563073719632,108.562528430054,109.561983140476,109.955742875644),
 .UNSPECIFIED.);
#1329=B_SPLINE_CURVE_WITH_KNOTS('',3,(#52392,#52393,#52394,#52395,#52396,
#52397,#52398,#52399,#52400,#52401),.UNSPECIFIED.,.F.,.F.,(4,1,1,1,1,1,
1,4),(103.672557568464,104.173429025116,105.173079691633,106.17273035815,
107.172381024666,108.172031691183,109.171682357699,109.955742875644),
 .UNSPECIFIED.);
#1330=B_SPLINE_CURVE_WITH_KNOTS('',3,(#52406,#52407,#52408,#52409,#52410,
#52411,#52412,#52413,#52414,#52415,#52416),.UNSPECIFIED.,.F.,.F.,(4,1,1,
1,1,1,1,1,4),(97.3893722612846,97.5685266154111,98.5679813258332,99.5674360362553,
100.566890746677,101.566345457099,102.565800167522,103.565254877944,103.672557568464),
 .UNSPECIFIED.);
#1331=B_SPLINE_CURVE_WITH_KNOTS('',3,(#52417,#52418,#52419,#52420,#52421,
#52422,#52423,#52424,#52425,#52426),.UNSPECIFIED.,.F.,.F.,(4,1,1,1,1,1,
1,4),(97.3893722612848,98.1755250260171,99.1751756925336,100.17482635905,
101.174477025567,102.174127692083,103.1737783586,103.672557568464),
 .UNSPECIFIED.);
#1332=B_SPLINE_CURVE_WITH_KNOTS('',3,(#52431,#52432,#52433,#52434,#52435,
#52436,#52437,#52438,#52439,#52440),.UNSPECIFIED.,.F.,.F.,(4,1,1,1,1,1,
1,4),(91.106186954105,91.5717983528786,92.5712530633007,93.5707077737228,
94.5701624841449,95.569617194567,96.5690719049891,97.3893722612846),
 .UNSPECIFIED.);
#1333=B_SPLINE_CURVE_WITH_KNOTS('',3,(#52441,#52442,#52443,#52444,#52445,
#52446,#52447,#52448,#52449,#52450,#52451),.UNSPECIFIED.,.F.,.F.,(4,1,1,
1,1,1,1,1,4),(91.1061869541052,91.1779703604012,92.1776210269178,93.1772716934343,
94.1769223599509,95.1765730264674,96.176223692984,97.1758743595006,97.3893722612848),
 .UNSPECIFIED.);
#1334=B_SPLINE_CURVE_WITH_KNOTS('',3,(#52456,#52457,#52458,#52459,#52460,
#52461,#52462,#52463,#52464,#52465),.UNSPECIFIED.,.F.,.F.,(4,1,1,1,1,1,
1,4),(84.8230016469254,85.5750700903461,86.5745248007682,87.5739795111903,
88.5734342216124,89.5728889320345,90.5723436424566,91.106186954105),
 .UNSPECIFIED.);
#1335=B_SPLINE_CURVE_WITH_KNOTS('',3,(#52466,#52467,#52468,#52469,#52470,
#52471,#52472,#52473,#52474,#52475),.UNSPECIFIED.,.F.,.F.,(4,1,1,1,1,1,
1,4),(84.8230016469256,85.1800663613019,86.1797170278185,87.179367694335,
88.1790183608516,89.1786690273681,90.1783196938847,91.1061869541052),
 .UNSPECIFIED.);
#1336=B_SPLINE_CURVE_WITH_KNOTS('',3,(#52480,#52481,#52482,#52483,#52484,
#52485,#52486,#52487,#52488,#52489,#52490),.UNSPECIFIED.,.F.,.F.,(4,1,1,
1,1,1,1,1,4),(78.5398163397458,78.5788871173915,79.5783418278136,80.5777965382357,
81.5772512486578,82.5767059590799,83.5761606695019,84.575615379924,84.8230016469254),
 .UNSPECIFIED.);
#1337=B_SPLINE_CURVE_WITH_KNOTS('',3,(#52491,#52492,#52493,#52494,#52495,
#52496,#52497,#52498,#52499,#52500),.UNSPECIFIED.,.F.,.F.,(4,1,1,1,1,1,
1,4),(78.539816339746,79.1821623622026,80.1818130287192,81.1814636952357,
82.1811143617523,83.1807650282688,84.1804156947854,84.8230016469256),
 .UNSPECIFIED.);
#1338=B_SPLINE_CURVE_WITH_KNOTS('',3,(#52505,#52506,#52507,#52508,#52509,
#52510,#52511,#52512,#52513,#52514),.UNSPECIFIED.,.F.,.F.,(4,1,1,1,1,1,
1,4),(72.2566310325662,72.582158854859,73.5816135652811,74.5810682757032,
75.5805229861253,76.5799776965474,77.5794324069694,78.5398163397458),
 .UNSPECIFIED.);
#1339=B_SPLINE_CURVE_WITH_KNOTS('',3,(#52515,#52516,#52517,#52518,#52519,
#52520,#52521,#52522,#52523,#52524),.UNSPECIFIED.,.F.,.F.,(4,1,1,1,1,1,
1,4),(72.2566310325664,73.1842583631033,74.1839090296199,75.1835596961364,
76.183210362653,77.1828610291695,78.1825116956861,78.539816339746),
 .UNSPECIFIED.);
#1340=B_SPLINE_CURVE_WITH_KNOTS('',3,(#52529,#52530,#52531,#52532,#52533,
#52534,#52535,#52536,#52537,#52538),.UNSPECIFIED.,.F.,.F.,(4,1,1,1,1,1,
1,4),(65.9734457253866,66.5854305923265,67.5848853027486,68.5843400131707,
69.5837947235928,70.5832494340148,71.5827041444369,72.2566310325662),
 .UNSPECIFIED.);
#1341=B_SPLINE_CURVE_WITH_KNOTS('',3,(#52539,#52540,#52541,#52542,#52543,
#52544,#52545,#52546,#52547,#52548,#52549),.UNSPECIFIED.,.F.,.F.,(4,1,1,
1,1,1,1,1,4),(65.9734457253868,66.1867036974875,67.186354364004,68.1860050305206,
69.1856556970371,70.1853063635537,71.1849570300702,72.1846076965868,72.2566310325664),
 .UNSPECIFIED.);
#1342=B_SPLINE_CURVE_WITH_KNOTS('',3,(#52554,#52555,#52556,#52557,#52558,
#52559,#52560,#52561,#52562,#52563),.UNSPECIFIED.,.F.,.F.,(4,1,1,1,1,1,
1,4),(59.690260418207,60.588702329794,61.5881570402161,62.5876117506382,
63.5870664610603,64.5865211714823,65.5859758819044,65.9734457253866),
 .UNSPECIFIED.);
#1343=B_SPLINE_CURVE_WITH_KNOTS('',3,(#52564,#52565,#52566,#52567,#52568,
#52569,#52570,#52571,#52572,#52573),.UNSPECIFIED.,.F.,.F.,(4,1,1,1,1,1,
1,4),(59.6902604182073,60.1887996983882,61.1884503649047,62.1881010314213,
63.1877516979378,64.1874023644544,65.1870530309709,65.9734457253868),
 .UNSPECIFIED.);
#1344=B_SPLINE_CURVE_WITH_KNOTS('',3,(#52578,#52579,#52580,#52581,#52582,
#52583,#52584,#52585,#52586,#52587,#52588),.UNSPECIFIED.,.F.,.F.,(4,1,1,
1,1,1,1,1,4),(53.4070751110274,53.5925193568394,54.5919740672615,55.5914287776836,
56.5908834881057,57.5903381985277,58.5897929089498,59.5892476193719,59.690260418207),
 .UNSPECIFIED.);
#1345=B_SPLINE_CURVE_WITH_KNOTS('',3,(#52589,#52590,#52591,#52592,#52593,
#52594,#52595,#52596,#52597,#52598),.UNSPECIFIED.,.F.,.F.,(4,1,1,1,1,1,
1,4),(53.4070751110277,54.1908956992888,55.1905463658054,56.1901970323219,
57.1898476988385,58.189498365355,59.1891490318716,59.6902604182073),
 .UNSPECIFIED.);
#1346=B_SPLINE_CURVE_WITH_KNOTS('',3,(#52603,#52604,#52605,#52606,#52607,
#52608,#52609,#52610,#52611,#52612),.UNSPECIFIED.,.F.,.F.,(4,1,1,1,1,1,
1,4),(47.1238898038478,47.5957910943069,48.595245804729,49.5947005151511,
50.5941552255731,51.5936099359952,52.5930646464173,53.4070751110274),
 .UNSPECIFIED.);
#1347=B_SPLINE_CURVE_WITH_KNOTS('',3,(#52613,#52614,#52615,#52616,#52617,
#52618,#52619,#52620,#52621,#52622,#52623),.UNSPECIFIED.,.F.,.F.,(4,1,1,
1,1,1,1,1,4),(47.1238898038481,47.193341033673,48.1929917001895,49.1926423667061,
50.1922930332226,51.1919436997392,52.1915943662557,53.1912450327723,53.4070751110277),
 .UNSPECIFIED.);
#1348=B_SPLINE_CURVE_WITH_KNOTS('',3,(#52628,#52629,#52630,#52631,#52632,
#52633,#52634,#52635,#52636,#52637),.UNSPECIFIED.,.F.,.F.,(4,1,1,1,1,1,
1,4),(40.8407044966683,41.5990628317744,42.5985175421965,43.5979722526185,
44.5974269630406,45.5968816734627,46.5963363838848,47.1238898038478),
 .UNSPECIFIED.);
#1349=B_SPLINE_CURVE_WITH_KNOTS('',3,(#52638,#52639,#52640,#52641,#52642,
#52643,#52644,#52645,#52646,#52647),.UNSPECIFIED.,.F.,.F.,(4,1,1,1,1,1,
1,4),(40.8407044966685,41.1954370345737,42.1950877010902,43.1947383676068,
44.1943890341233,45.1940397006399,46.1936903671564,47.1238898038481),
 .UNSPECIFIED.);
#1350=B_SPLINE_CURVE_WITH_KNOTS('',3,(#52652,#52653,#52654,#52655,#52656,
#52657,#52658,#52659,#52660,#52661,#52662),.UNSPECIFIED.,.F.,.F.,(4,1,1,
1,1,1,1,1,4),(34.5575191894887,34.6028798588198,35.6023345692419,36.601789279664,
37.601243990086,38.6006987005081,39.6001534109302,40.5996081213523,40.8407044966683),
 .UNSPECIFIED.);
#1351=B_SPLINE_CURVE_WITH_KNOTS('',3,(#52663,#52664,#52665,#52666,#52667,
#52668,#52669,#52670,#52671,#52672),.UNSPECIFIED.,.F.,.F.,(4,1,1,1,1,1,
1,4),(34.5575191894889,35.1975330354744,36.1971837019909,37.1968343685075,
38.196485035024,39.1961357015406,40.1957863680571,40.8407044966685),
 .UNSPECIFIED.);
#1352=B_SPLINE_CURVE_WITH_KNOTS('',3,(#52677,#52678,#52679,#52680,#52681,
#52682,#52683,#52684,#52685,#52686),.UNSPECIFIED.,.F.,.F.,(4,1,1,1,1,1,
1,4),(28.2743338823091,28.6061515962873,29.6056063067094,30.6050610171314,
31.6045157275535,32.6039704379756,33.6034251483977,34.5575191894887),
 .UNSPECIFIED.);
#1353=B_SPLINE_CURVE_WITH_KNOTS('',3,(#52687,#52688,#52689,#52690,#52691,
#52692,#52693,#52694,#52695,#52696),.UNSPECIFIED.,.F.,.F.,(4,1,1,1,1,1,
1,4),(28.2743338823093,29.1996290363751,30.1992797028916,31.1989303694082,
32.1985810359247,33.1982317024413,34.1978823689578,34.5575191894889),
 .UNSPECIFIED.);
#1354=B_SPLINE_CURVE_WITH_KNOTS('',3,(#52701,#52702,#52703,#52704,#52705,
#52706,#52707,#52708,#52709,#52710),.UNSPECIFIED.,.F.,.F.,(4,1,1,1,1,1,
1,4),(21.9911485751295,22.6094233337548,23.6088780441768,24.6083327545989,
25.607787465021,26.6072421754431,27.6066968858652,28.2743338823091),
 .UNSPECIFIED.);
#1355=B_SPLINE_CURVE_WITH_KNOTS('',3,(#52711,#52712,#52713,#52714,#52715,
#52716,#52717,#52718,#52719,#52720,#52721),.UNSPECIFIED.,.F.,.F.,(4,1,1,
1,1,1,1,1,4),(21.9911485751297,22.2020743707592,23.2017250372758,24.2013757037923,
25.2010263703089,26.2006770368254,27.200327703342,28.1999783698585,28.2743338823093),
 .UNSPECIFIED.);
#1356=B_SPLINE_CURVE_WITH_KNOTS('',3,(#52726,#52727,#52728,#52729,#52730,
#52731,#52732,#52733,#52734,#52735),.UNSPECIFIED.,.F.,.F.,(4,1,1,1,1,1,
1,4),(15.7079632679499,16.6126950712223,17.6121497816443,18.6116044920664,
19.6110592024885,20.6105139129106,21.6099686233327,21.9911485751295),
 .UNSPECIFIED.);
#1357=B_SPLINE_CURVE_WITH_KNOTS('',3,(#52736,#52737,#52738,#52739,#52740,
#52741,#52742,#52743,#52744,#52745),.UNSPECIFIED.,.F.,.F.,(4,1,1,1,1,1,
1,4),(15.7079632679501,16.2041703716599,17.2038210381765,18.203471704693,
19.2031223712096,20.2027730377261,21.2024237042427,21.9911485751297),
 .UNSPECIFIED.);
#1358=B_SPLINE_CURVE_WITH_KNOTS('',3,(#52748,#52749,#52750,#52751,#52752,
#52753,#52754,#52755,#52756,#52757,#52758,#52759,#52760,#52761,#52762,#52763,
#52764,#52765,#52766,#52767,#52768,#52769,#52770,#52771,#52772,#52773,#52774,
#52775,#52776,#52777,#52778,#52779,#52780,#52781,#52782,#52783,#52784,#52785,
#52786,#52787,#52788,#52789,#52790,#52791,#52792,#52793,#52794,#52795,#52796,
#52797,#52798,#52799,#52800,#52801,#52802,#52803,#52804,#52805,#52806,#52807,
#52808,#52809,#52810,#52811,#52812,#52813,#52814,#52815,#52816,#52817,#52818,
#52819,#52820),.UNSPECIFIED.,.F.,.F.,(4,3,3,3,3,3,3,3,3,3,3,3,3,3,3,3,3,
3,3,3,3,3,3,3,4),(-0.833806508238614,-0.784110841134283,-0.735306998950323,
-0.687259726601284,-0.645877709227694,-0.62807402512667,-0.620323068728151,
-0.604495691854104,-0.557043524288525,-0.509117916148162,-0.461617173214432,
-0.427640023675466,-0.414574598236473,-0.406906758156835,-0.401016345434302,
-0.354784550175495,-0.325708575058567,-0.279459204769296,-0.233637516184487,
-0.212276112655899,-0.199827110241752,-0.194271984707397,-0.14972919330764,
-0.105716619472331,-0.0627462879557836),.UNSPECIFIED.);
#1359=B_SPLINE_CURVE_WITH_KNOTS('',3,(#52822,#52823,#52824,#52825,#52826,
#52827,#52828,#52829,#52830,#52831,#52832,#52833,#52834,#52835,#52836,#52837,
#52838,#52839,#52840,#52841,#52842,#52843,#52844,#52845,#52846,#52847,#52848,
#52849,#52850,#52851,#52852,#52853,#52854,#52855,#52856,#52857,#52858,#52859,
#52860,#52861,#52862,#52863,#52864,#52865,#52866,#52867,#52868,#52869,#52870,
#52871,#52872,#52873,#52874,#52875,#52876,#52877,#52878,#52879,#52880,#52881,
#52882,#52883,#52884,#52885,#52886,#52887,#52888,#52889,#52890,#52891,#52892,
#52893,#52894,#52895,#52896,#52897,#52898,#52899,#52900,#52901,#52902,#52903,
#52904,#52905,#52906,#52907,#52908,#52909,#52910,#52911,#52912,#52913,#52914,
#52915,#52916,#52917,#52918,#52919,#52920,#52921,#52922,#52923,#52924,#52925,
#52926,#52927,#52928,#52929,#52930,#52931,#52932,#52933,#52934,#52935,#52936,
#52937,#52938,#52939,#52940,#52941,#52942,#52943,#52944,#52945,#52946,#52947,
#52948,#52949,#52950,#52951,#52952,#52953,#52954,#52955,#52956,#52957,#52958,
#52959,#52960,#52961,#52962,#52963,#52964,#52965,#52966,#52967,#52968,#52969,
#52970,#52971,#52972,#52973,#52974,#52975,#52976,#52977,#52978,#52979,#52980,
#52981,#52982,#52983,#52984,#52985,#52986,#52987,#52988,#52989,#52990,#52991,
#52992,#52993,#52994,#52995,#52996,#52997,#52998,#52999,#53000,#53001,#53002,
#53003,#53004,#53005,#53006,#53007,#53008,#53009,#53010,#53011,#53012,#53013,
#53014,#53015,#53016,#53017,#53018,#53019,#53020,#53021,#53022,#53023,#53024,
#53025,#53026,#53027,#53028,#53029,#53030,#53031,#53032,#53033,#53034,#53035,
#53036,#53037,#53038,#53039,#53040,#53041,#53042,#53043,#53044,#53045,#53046,
#53047,#53048,#53049,#53050,#53051,#53052,#53053,#53054,#53055,#53056,#53057,
#53058,#53059,#53060,#53061,#53062,#53063,#53064,#53065,#53066,#53067,#53068,
#53069,#53070,#53071,#53072,#53073,#53074,#53075,#53076,#53077,#53078,#53079,
#53080,#53081,#53082,#53083,#53084,#53085,#53086,#53087,#53088,#53089,#53090,
#53091,#53092,#53093,#53094,#53095,#53096,#53097,#53098,#53099,#53100,#53101),
 .UNSPECIFIED.,.F.,.F.,(4,3,3,3,3,3,3,3,3,3,3,3,3,3,3,3,3,3,3,3,3,3,3,3,
3,3,3,3,3,3,3,3,3,3,3,3,3,3,3,3,3,3,3,3,3,3,3,3,3,3,3,3,3,3,3,3,3,3,3,3,
3,3,3,3,3,3,3,3,3,3,3,3,3,3,3,3,3,3,3,3,3,3,3,3,3,3,3,3,3,3,3,3,3,4),(-2.8505485327553,
-2.80573427450524,-2.77511892064891,-2.76323501298752,-2.7578271088511,
-2.71268252538819,-2.68327285907993,-2.63807445758683,-2.61160951174613,
-2.59853995865707,-2.5879328823648,-2.5817358151457,-2.5361463925531,-2.49054398414152,
-2.44565509913639,-2.42635489086124,-2.39343442202386,-2.38640148315151,
-2.38063442805171,-2.33614443609276,-2.29063594485493,-2.24440704909113,
-2.20130959163764,-2.18782840844821,-2.1815609373624,-2.17543544873235,
-2.1287835245443,-2.08184078143437,-2.03551021638789,-2.00153950965672,
-1.98594287672261,-1.97665838033466,-1.97074492343949,-1.92364723254399,
-1.89962738946321,-1.8536836277288,-1.80688299109426,-1.77866383131902,
-1.769614968468,-1.76173733059279,-1.71535978925738,-1.66772881631917,-1.61991043415747,
-1.58684368422409,-1.55789442552168,-1.55016980216945,-1.5014714602997,
-1.4534466233461,-1.40441152901827,-1.35822610122742,-1.35537643469044,
-1.34088108273801,-1.33444858249317,-1.28819265226034,-1.24082690028513,
-1.19260099076567,-1.14276637745728,-1.12831574751615,-1.12231458018188,
-1.07369356250354,-1.02459245907517,-0.975558021868307,-0.930149537475869,
-0.913121355828704,-0.904001509154352,-0.898152153874911,-0.84868958328962,
-0.799775975381224,-0.793924084298553,-0.745422579095372,-0.712280661750332,
-0.69384093619032,-0.68376800953834,-0.677703857148311,-0.629392367529373,
-0.577612309285043,-0.527597792884359,-0.488542056470656,-0.471325584677335,
-0.461423807374008,-0.452963847209369,-0.402681212061588,-0.352415085644384,
-0.302711700252363,-0.258931800913549,-0.237041851244141,-0.230232856748154,
-0.224025422271845,-0.215151901574734,-0.167089464755252,-0.117446387488254,
-0.0671034891247927,-0.0162957457720915,0.),.UNSPECIFIED.);
#1360=B_SPLINE_CURVE_WITH_KNOTS('',3,(#53105,#53106,#53107,#53108,#53109,
#53110,#53111),.UNSPECIFIED.,.F.,.F.,(4,3,4),(1.04608885943707,1.08948735834114,
1.13094109509796),.UNSPECIFIED.);
#1361=B_SPLINE_CURVE_WITH_KNOTS('',3,(#53114,#53115,#53116,#53117,#53118,
#53119,#53120),.UNSPECIFIED.,.F.,.F.,(4,3,4),(0.,0.0443247549663995,0.084677685176745),
 .UNSPECIFIED.);
#1362=B_SPLINE_CURVE_WITH_KNOTS('',3,(#53136,#53137,#53138,#53139,#53140,
#53141,#53142,#53143,#53144,#53145,#53146,#53147,#53148,#53149,#53150,#53151,
#53152,#53153,#53154,#53155,#53156,#53157,#53158,#53159,#53160,#53161,#53162,
#53163,#53164,#53165,#53166,#53167,#53168,#53169,#53170,#53171,#53172,#53173,
#53174,#53175,#53176,#53177,#53178,#53179,#53180,#53181,#53182,#53183,#53184,
#53185,#53186,#53187,#53188,#53189,#53190,#53191,#53192,#53193,#53194,#53195,
#53196,#53197,#53198,#53199,#53200,#53201,#53202,#53203,#53204,#53205,#53206,
#53207,#53208,#53209,#53210,#53211,#53212,#53213,#53214,#53215,#53216,#53217,
#53218,#53219,#53220,#53221,#53222,#53223,#53224,#53225,#53226,#53227,#53228,
#53229,#53230,#53231,#53232,#53233,#53234,#53235,#53236,#53237,#53238,#53239,
#53240,#53241,#53242,#53243,#53244,#53245,#53246,#53247,#53248,#53249,#53250),
 .UNSPECIFIED.,.F.,.F.,(4,3,3,3,3,3,3,3,3,3,3,3,3,3,3,3,3,3,3,3,3,3,3,3,
3,3,3,3,3,3,3,3,3,3,3,3,3,3,4),(-1.13094109509824,-1.09563331911551,-1.05277492694931,
-1.02270576365399,-1.00715902947279,-0.999434161139063,-0.992415787646934,
-0.948423021491772,-0.901328683083329,-0.880724910029636,-0.865673266591215,
-0.85985042234436,-0.814096270843057,-0.767722321418939,-0.721190349721597,
-0.683809840847257,-0.669300679648143,-0.659993560535856,-0.654189217743676,
-0.606509202994476,-0.571668314224235,-0.525516476930707,-0.478640819134196,
-0.455267754576504,-0.447581100598068,-0.442041462532518,-0.39477738260878,
-0.346766372069733,-0.298184121586594,-0.291656302672655,-0.255199264838573,
-0.239249310786162,-0.229177328973695,-0.222810242437123,-0.173603985401498,
-0.123778246004826,-0.0739959577271227,-0.0248532857217371,0.),
 .UNSPECIFIED.);
#1363=B_SPLINE_CURVE_WITH_KNOTS('',3,(#53251,#53252,#53253,#53254,#53255,
#53256,#53257,#53258,#53259,#53260,#53261,#53262,#53263,#53264,#53265,#53266,
#53267,#53268,#53269,#53270,#53271,#53272,#53273,#53274,#53275,#53276,#53277,
#53278,#53279,#53280,#53281,#53282,#53283,#53284,#53285,#53286,#53287,#53288,
#53289,#53290,#53291,#53292,#53293,#53294,#53295,#53296,#53297,#53298,#53299,
#53300,#53301,#53302,#53303,#53304,#53305,#53306,#53307,#53308,#53309,#53310,
#53311,#53312,#53313,#53314,#53315,#53316,#53317,#53318,#53319,#53320,#53321,
#53322,#53323,#53324,#53325,#53326,#53327,#53328,#53329,#53330,#53331,#53332,
#53333,#53334,#53335,#53336,#53337,#53338,#53339,#53340,#53341,#53342,#53343,
#53344,#53345,#53346,#53347,#53348,#53349,#53350,#53351,#53352,#53353,#53354,
#53355,#53356,#53357,#53358,#53359),.UNSPECIFIED.,.F.,.F.,(4,3,3,3,3,3,
3,3,3,3,3,3,3,3,3,3,3,3,3,3,3,3,3,3,3,3,3,3,3,3,3,3,3,3,3,3,4),(-1.12653966532762,
-1.08490854816515,-1.03522530378325,-1.00297074027101,-0.98193935568292,
-0.97317885460119,-0.965315969455476,-0.916182132148453,-0.86655340157831,
-0.822266762307489,-0.815588448831975,-0.767271193265127,-0.719185403827295,
-0.671761178654938,-0.633608955888029,-0.616498884302865,-0.606206529965436,
-0.599913578153287,-0.553803068539291,-0.519152287587304,-0.472463419784273,
-0.425808948481975,-0.404285750458287,-0.397320170626258,-0.391056720436118,
-0.345587767561757,-0.299605565927115,-0.253623364292473,-0.221920443755914,
-0.205347277549075,-0.194960257430732,-0.189028113959442,-0.144730321897778,
-0.100642231601604,-0.0569916939973363,-0.014221171191207,0.),
 .UNSPECIFIED.);
#1364=B_SPLINE_CURVE_WITH_KNOTS('',3,(#55392,#55393,#55394,#55395,#55396,
#55397,#55398,#55399,#55400,#55401),.UNSPECIFIED.,.F.,.F.,(4,1,1,1,1,1,
1,4),(10.375727056019,10.7060917058189,11.2059170390771,12.2055677055937,
13.2052183721102,14.2048690386268,15.2045197051434,15.7079632679501),
 .UNSPECIFIED.);
#1365=B_SPLINE_CURVE_WITH_KNOTS('',3,(#55402,#55403,#55404,#55405,#55406,
#55407,#55408,#55409,#55410,#55411,#55412,#55413,#55414,#55415,#55416,#55417,
#55418,#55419,#55420,#55421,#55422,#55423),.UNSPECIFIED.,.F.,.F.,(4,3,3,
3,3,3,3,4),(491.207309053546,491.729170098438,492.728820764955,493.728471431471,
494.728122097988,495.727772764504,496.727423431021,497.490494360725),
 .UNSPECIFIED.);
#1366=B_SPLINE_CURVE_WITH_KNOTS('',3,(#55425,#55426,#55427,#55428,#55429,
#55430,#55431,#55432,#55433),.UNSPECIFIED.,.F.,.F.,(4,1,1,1,1,1,4),(11.6154215191118,
12.1151488743229,12.6148762295339,13.614330939956,14.6137856503781,15.6132403608002,
15.7079632679499),.UNSPECIFIED.);
#1367=B_SPLINE_CURVE_WITH_KNOTS('',3,(#57474,#57475,#57476,#57477,#57478,
#57479,#57480,#57481,#57482,#57483,#57484,#57485,#57486,#57487,#57488,#57489,
#57490,#57491,#57492,#57493,#57494,#57495),.UNSPECIFIED.,.F.,.F.,(4,3,3,
3,3,3,3,4),(-500.464181016024,-499.727355211043,-498.72790050062,-497.728445790198,
-496.728991079776,-495.729536369354,-494.730081658932,-494.180995708845),
 .UNSPECIFIED.);
#1368=B_SPLINE_CURVE_WITH_KNOTS('',3,(#57596,#57597,#57598,#57599,#57600,
#57601,#57602,#57603,#57604,#57605),.UNSPECIFIED.,.F.,.F.,(4,3,3,4),(-4.09293042013067,
-3.97124047255661,-2.97843035441746,-2.06863817490915),.UNSPECIFIED.);
#1369=B_SPLINE_CURVE_WITH_KNOTS('',3,(#57608,#57609,#57610,#57611,#57612,
#57613,#57614),.UNSPECIFIED.,.F.,.F.,(4,3,4),(0.,0.992810118139154,1.11730040836816),
 .UNSPECIFIED.);
#1370=B_SPLINE_CURVE_WITH_KNOTS('',3,(#57619,#57620,#57621,#57622,#57623,
#57624,#57625,#57626,#57627,#57628,#57629,#57630,#57631,#57632,#57633,#57634,
#57635,#57636,#57637,#57638,#57639,#57640),.UNSPECIFIED.,.F.,.F.,(4,3,3,
3,3,3,3,4),(-10.3761157273103,-9.92810118139153,-8.93529106325238,-7.94248094511322,
-6.94967082697407,-5.95686070883492,-4.96405059069577,-4.09293042013067),
 .UNSPECIFIED.);
#1371=B_SPLINE_CURVE_WITH_KNOTS('',3,(#57641,#57642,#57643,#57644,#57645,
#57646,#57647,#57648,#57649,#57650,#57651,#57652,#57653,#57654,#57655,#57656,
#57657,#57658,#57659,#57660,#57661,#57662),.UNSPECIFIED.,.F.,.F.,(4,3,3,
3,3,3,3,4),(1.11730040836816,1.98562023627831,2.97843035441746,3.97124047255661,
4.96405059069576,5.95686070883492,6.94967082697407,7.40048571554774),
 .UNSPECIFIED.);
#1372=B_SPLINE_CURVE_WITH_KNOTS('',3,(#57667,#57668,#57669,#57670,#57671,
#57672,#57673,#57674,#57675,#57676,#57677,#57678,#57679,#57680,#57681,#57682,
#57683,#57684,#57685,#57686,#57687,#57688),.UNSPECIFIED.,.F.,.F.,(4,3,3,
3,3,3,3,4),(-16.6593010344898,-15.8849618902264,-14.8921517720873,-13.8993416539481,
-12.906531535809,-11.9137214176698,-10.9209112995307,-10.3761157273103),
 .UNSPECIFIED.);
#1373=B_SPLINE_CURVE_WITH_KNOTS('',3,(#57689,#57690,#57691,#57692,#57693,
#57694,#57695,#57696,#57697,#57698,#57699,#57700,#57701,#57702,#57703,#57704,
#57705,#57706,#57707,#57708,#57709,#57710),.UNSPECIFIED.,.F.,.F.,(4,3,3,
3,3,3,3,4),(7.40048571554774,7.94248094511322,8.93529106325238,9.92810118139153,
10.9209112995307,11.9137214176698,12.906531535809,13.6836710227273),
 .UNSPECIFIED.);
#1374=B_SPLINE_CURVE_WITH_KNOTS('',3,(#57715,#57716,#57717,#57718,#57719,
#57720,#57721,#57722,#57723,#57724,#57725,#57726,#57727,#57728,#57729,#57730,
#57731,#57732,#57733,#57734,#57735,#57736,#57737,#57738,#57739),
 .UNSPECIFIED.,.F.,.F.,(4,3,3,3,3,3,3,3,4),(-22.9424863416694,-22.8346327172005,
-21.8418225990614,-20.8490124809222,-19.8562023627831,-18.8633922446439,
-17.8705821265048,-16.8777720083656,-16.6593010344898),.UNSPECIFIED.);
#1375=B_SPLINE_CURVE_WITH_KNOTS('',3,(#57740,#57741,#57742,#57743,#57744,
#57745,#57746,#57747,#57748,#57749,#57750,#57751,#57752,#57753,#57754,#57755,
#57756,#57757,#57758,#57759,#57760,#57761,#57762,#57763,#57764),
 .UNSPECIFIED.,.F.,.F.,(4,3,3,3,3,3,3,3,4),(13.6836710227273,13.8993416539481,
14.8921517720873,15.8849618902264,16.8777720083656,17.8705821265047,18.8633922446439,
19.856202362783,19.9668563299069),.UNSPECIFIED.);
#1376=B_SPLINE_CURVE_WITH_KNOTS('',3,(#57769,#57770,#57771,#57772,#57773,
#57774,#57775,#57776,#57777,#57778,#57779,#57780,#57781,#57782,#57783,#57784,
#57785,#57786,#57787,#57788,#57789,#57790),.UNSPECIFIED.,.F.,.F.,(4,3,3,
3,3,3,3,4),(-29.225671648849,-28.7914934260354,-27.7986833078963,-26.8058731897571,
-25.813063071618,-24.8202529534788,-23.8274428353397,-22.9424863416694),
 .UNSPECIFIED.);
#1377=B_SPLINE_CURVE_WITH_KNOTS('',3,(#57791,#57792,#57793,#57794,#57795,
#57796,#57797,#57798,#57799,#57800,#57801,#57802,#57803,#57804,#57805,#57806,
#57807,#57808,#57809,#57810,#57811,#57812),.UNSPECIFIED.,.F.,.F.,(4,3,3,
3,3,3,3,4),(19.9668563299069,20.8490124809222,21.8418225990614,22.8346327172005,
23.8274428353397,24.8202529534788,25.813063071618,26.2500416370865),
 .UNSPECIFIED.);
#1378=B_SPLINE_CURVE_WITH_KNOTS('',3,(#57817,#57818,#57819,#57820,#57821,
#57822,#57823,#57824,#57825,#57826,#57827,#57828,#57829,#57830,#57831,#57832,
#57833,#57834,#57835,#57836,#57837,#57838),.UNSPECIFIED.,.F.,.F.,(4,3,3,
3,3,3,3,4),(-35.5088569560286,-34.7483541348703,-33.7555440167312,-32.762733898592,
-31.7699237804529,-30.7771136623137,-29.7843035441746,-29.225671648849),
 .UNSPECIFIED.);
#1379=B_SPLINE_CURVE_WITH_KNOTS('',3,(#57839,#57840,#57841,#57842,#57843,
#57844,#57845,#57846,#57847,#57848,#57849,#57850,#57851,#57852,#57853,#57854,
#57855,#57856,#57857,#57858,#57859,#57860),.UNSPECIFIED.,.F.,.F.,(4,3,3,
3,3,3,3,4),(26.2500416370865,26.8058731897571,27.7986833078963,28.7914934260354,
29.7843035441746,30.7771136623137,31.7699237804529,32.5332269442661),
 .UNSPECIFIED.);
#1380=B_SPLINE_CURVE_WITH_KNOTS('',3,(#57865,#57866,#57867,#57868,#57869,
#57870,#57871,#57872,#57873,#57874,#57875,#57876,#57877,#57878,#57879,#57880,
#57881,#57882,#57883,#57884,#57885,#57886,#57887,#57888,#57889),
 .UNSPECIFIED.,.F.,.F.,(4,3,3,3,3,3,3,3,4),(-41.7920422632082,-41.6980249618444,
-40.7052148437053,-39.7124047255661,-38.719594607427,-37.7267844892878,
-36.7339743711486,-35.7411642530095,-35.5088569560286),.UNSPECIFIED.);
#1381=B_SPLINE_CURVE_WITH_KNOTS('',3,(#57890,#57891,#57892,#57893,#57894,
#57895,#57896,#57897,#57898,#57899,#57900,#57901,#57902,#57903,#57904,#57905,
#57906,#57907,#57908,#57909,#57910,#57911,#57912,#57913,#57914),
 .UNSPECIFIED.,.F.,.F.,(4,3,3,3,3,3,3,3,4),(32.5332269442661,32.762733898592,
33.7555440167312,34.7483541348703,35.7411642530095,36.7339743711486,37.7267844892878,
38.7195946074269,38.8164122514457),.UNSPECIFIED.);
#1382=B_SPLINE_CURVE_WITH_KNOTS('',3,(#57919,#57920,#57921,#57922,#57923,
#57924,#57925,#57926,#57927,#57928,#57929,#57930,#57931,#57932,#57933,#57934,
#57935,#57936,#57937,#57938,#57939,#57940),.UNSPECIFIED.,.F.,.F.,(4,3,3,
3,3,3,3,4),(-48.0752275703878,-47.6548856706793,-46.6620755525402,-45.669265434401,
-44.6764553162619,-43.6836451981227,-42.6908350799836,-41.7920422632082),
 .UNSPECIFIED.);
#1383=B_SPLINE_CURVE_WITH_KNOTS('',3,(#57941,#57942,#57943,#57944,#57945,
#57946,#57947,#57948,#57949,#57950,#57951,#57952,#57953,#57954,#57955,#57956,
#57957,#57958,#57959,#57960,#57961,#57962),.UNSPECIFIED.,.F.,.F.,(4,3,3,
3,3,3,3,4),(38.8164122514457,39.7124047255661,40.7052148437053,41.6980249618444,
42.6908350799836,43.6836451981227,44.6764553162619,45.0995975586253),
 .UNSPECIFIED.);
#1384=B_SPLINE_CURVE_WITH_KNOTS('',3,(#57967,#57968,#57969,#57970,#57971,
#57972,#57973,#57974,#57975,#57976,#57977,#57978,#57979,#57980,#57981,#57982,
#57983,#57984,#57985,#57986,#57987,#57988),.UNSPECIFIED.,.F.,.F.,(4,3,3,
3,3,3,3,4),(-54.3584128775674,-53.6117463795143,-52.6189362613751,-51.626126143236,
-50.6333160250968,-49.6405059069576,-48.6476957888185,-48.0752275703878),
 .UNSPECIFIED.);
#1385=B_SPLINE_CURVE_WITH_KNOTS('',3,(#57989,#57990,#57991,#57992,#57993,
#57994,#57995,#57996,#57997,#57998,#57999,#58000,#58001,#58002,#58003,#58004,
#58005,#58006,#58007,#58008,#58009,#58010),.UNSPECIFIED.,.F.,.F.,(4,3,3,
3,3,3,3,4),(45.0995975586253,45.669265434401,46.6620755525402,47.6548856706793,
48.6476957888185,49.6405059069576,50.6333160250968,51.3827828658049),
 .UNSPECIFIED.);
#1386=B_SPLINE_CURVE_WITH_KNOTS('',3,(#58015,#58016,#58017,#58018,#58019,
#58020,#58021,#58022,#58023,#58024,#58025,#58026,#58027,#58028,#58029,#58030,
#58031,#58032,#58033,#58034,#58035,#58036,#58037,#58038,#58039),
 .UNSPECIFIED.,.F.,.F.,(4,3,3,3,3,3,3,3,4),(-60.641598184747,-60.5614172064883,
-59.5686070883492,-58.57579697021,-57.5829868520709,-56.5901767339317,-55.5973666157926,
-54.6045564976534,-54.3584128775674),.UNSPECIFIED.);
#1387=B_SPLINE_CURVE_WITH_KNOTS('',3,(#58040,#58041,#58042,#58043,#58044,
#58045,#58046,#58047,#58048,#58049,#58050,#58051,#58052,#58053,#58054,#58055,
#58056,#58057,#58058,#58059,#58060,#58061,#58062,#58063,#58064),
 .UNSPECIFIED.,.F.,.F.,(4,3,3,3,3,3,3,3,4),(51.3827828658049,51.626126143236,
52.6189362613751,53.6117463795143,54.6045564976534,55.5973666157926,56.5901767339317,
57.5829868520709,57.6659681729845),.UNSPECIFIED.);
#1388=B_SPLINE_CURVE_WITH_KNOTS('',3,(#58069,#58070,#58071,#58072,#58073,
#58074,#58075,#58076,#58077,#58078,#58079,#58080,#58081,#58082,#58083,#58084,
#58085,#58086,#58087,#58088,#58089,#58090),.UNSPECIFIED.,.F.,.F.,(4,3,3,
3,3,3,3,4),(-66.9247834919266,-66.5182779153233,-65.5254677971841,-64.5326576790449,
-63.5398475609058,-62.5470374427666,-61.5542273246275,-60.641598184747),
 .UNSPECIFIED.);
#1389=B_SPLINE_CURVE_WITH_KNOTS('',3,(#58091,#58092,#58093,#58094,#58095,
#58096,#58097,#58098,#58099,#58100,#58101,#58102,#58103,#58104,#58105,#58106,
#58107,#58108,#58109,#58110,#58111,#58112),.UNSPECIFIED.,.F.,.F.,(4,3,3,
3,3,3,3,4),(57.6659681729845,58.57579697021,59.5686070883492,60.5614172064883,
61.5542273246275,62.5470374427666,63.5398475609058,63.949153480164),
 .UNSPECIFIED.);
#1390=B_SPLINE_CURVE_WITH_KNOTS('',3,(#58117,#58118,#58119,#58120,#58121,
#58122,#58123,#58124,#58125,#58126,#58127,#58128,#58129,#58130,#58131,#58132,
#58133,#58134,#58135,#58136,#58137,#58138),.UNSPECIFIED.,.F.,.F.,(4,3,3,
3,3,3,3,4),(-73.2079687991062,-72.4751386241581,-71.482328506019,-70.4895183878799,
-69.4967082697407,-68.5038981516016,-67.5110880334624,-66.9247834919266),
 .UNSPECIFIED.);
#1391=B_SPLINE_CURVE_WITH_KNOTS('',3,(#58139,#58140,#58141,#58142,#58143,
#58144,#58145,#58146,#58147,#58148,#58149,#58150,#58151,#58152,#58153,#58154,
#58155,#58156,#58157,#58158,#58159,#58160),.UNSPECIFIED.,.F.,.F.,(4,3,3,
3,3,3,3,4),(63.949153480164,64.5326576790449,65.5254677971841,66.5182779153232,
67.5110880334624,68.5038981516015,69.4967082697407,70.2323387873436),
 .UNSPECIFIED.);
#1392=B_SPLINE_CURVE_WITH_KNOTS('',3,(#58165,#58166,#58167,#58168,#58169,
#58170,#58171,#58172,#58173,#58174,#58175,#58176,#58177,#58178,#58179,#58180,
#58181,#58182,#58183,#58184,#58185,#58186,#58187,#58188,#58189),
 .UNSPECIFIED.,.F.,.F.,(4,3,3,3,3,3,3,3,4),(-79.4911541062858,-79.4248094511322,
-78.4319993329931,-77.4391892148539,-76.4463790967148,-75.4535689785756,
-74.4607588604365,-73.4679487422973,-73.2079687991062),.UNSPECIFIED.);
#1393=B_SPLINE_CURVE_WITH_KNOTS('',3,(#58190,#58191,#58192,#58193,#58194,
#58195,#58196,#58197,#58198,#58199,#58200,#58201,#58202,#58203,#58204,#58205,
#58206,#58207,#58208,#58209,#58210,#58211,#58212,#58213,#58214),
 .UNSPECIFIED.,.F.,.F.,(4,3,3,3,3,3,3,3,4),(70.2323387873436,70.4895183878799,
71.482328506019,72.4751386241582,73.4679487422973,74.4607588604365,75.4535689785756,
76.4463790967148,76.5155240945232),.UNSPECIFIED.);
#1394=B_SPLINE_CURVE_WITH_KNOTS('',3,(#58219,#58220,#58221,#58222,#58223,
#58224,#58225,#58226,#58227,#58228,#58229,#58230,#58231,#58232,#58233,#58234,
#58235,#58236,#58237,#58238,#58239,#58240),.UNSPECIFIED.,.F.,.F.,(4,3,3,
3,3,3,3,4),(-85.7743394134654,-85.3816701599672,-84.388860041828,-83.3960499236888,
-82.4032398055497,-81.4104296874105,-80.4176195692714,-79.4911541062858),
 .UNSPECIFIED.);
#1395=B_SPLINE_CURVE_WITH_KNOTS('',3,(#58241,#58242,#58243,#58244,#58245,
#58246,#58247,#58248,#58249,#58250,#58251,#58252,#58253,#58254,#58255,#58256,
#58257,#58258,#58259,#58260,#58261,#58262),.UNSPECIFIED.,.F.,.F.,(4,3,3,
3,3,3,3,4),(76.5155240945232,77.4391892148539,78.4319993329931,79.4248094511322,
80.4176195692714,81.4104296874105,82.4032398055497,82.7987094017028),
 .UNSPECIFIED.);
#1396=B_SPLINE_CURVE_WITH_KNOTS('',3,(#58267,#58268,#58269,#58270,#58271,
#58272,#58273,#58274,#58275,#58276,#58277,#58278,#58279,#58280,#58281,#58282,
#58283,#58284,#58285,#58286,#58287,#58288),.UNSPECIFIED.,.F.,.F.,(4,3,3,
3,3,3,3,4),(-92.0575247206449,-91.3385308688021,-90.3457207506629,-89.3529106325238,
-88.3601005143846,-87.3672903962455,-86.3744802781063,-85.7743394134654),
 .UNSPECIFIED.);
#1397=B_SPLINE_CURVE_WITH_KNOTS('',3,(#58289,#58290,#58291,#58292,#58293,
#58294,#58295,#58296,#58297,#58298,#58299,#58300,#58301,#58302,#58303,#58304,
#58305,#58306,#58307,#58308,#58309,#58310),.UNSPECIFIED.,.F.,.F.,(4,3,3,
3,3,3,3,4),(82.7987094017028,83.3960499236888,84.388860041828,85.3816701599672,
86.3744802781063,87.3672903962455,88.3601005143846,89.0818947088824),
 .UNSPECIFIED.);
#1398=B_SPLINE_CURVE_WITH_KNOTS('',3,(#58315,#58316,#58317,#58318,#58319,
#58320,#58321,#58322,#58323,#58324,#58325,#58326,#58327,#58328,#58329,#58330,
#58331,#58332,#58333,#58334,#58335,#58336,#58337,#58338,#58339),
 .UNSPECIFIED.,.F.,.F.,(4,3,3,3,3,3,3,3,4),(-98.3407100278245,-98.2882016957761,
-97.295391577637,-96.3025814594978,-95.3097713413587,-94.3169612232195,
-93.3241511050804,-92.3313409869412,-92.0575247206449),.UNSPECIFIED.);
#1399=B_SPLINE_CURVE_WITH_KNOTS('',3,(#58340,#58341,#58342,#58343,#58344,
#58345,#58346,#58347,#58348,#58349,#58350,#58351,#58352,#58353,#58354,#58355,
#58356,#58357,#58358,#58359,#58360,#58361,#58362,#58363,#58364),
 .UNSPECIFIED.,.F.,.F.,(4,3,3,3,3,3,3,3,4),(89.0818947088824,89.3529106325238,
90.3457207506629,91.3385308688021,92.3313409869412,93.3241511050804,94.3169612232195,
95.3097713413587,95.365080016062),.UNSPECIFIED.);
#1400=B_SPLINE_CURVE_WITH_KNOTS('',3,(#58369,#58370,#58371,#58372,#58373,
#58374,#58375,#58376,#58377,#58378,#58379,#58380,#58381,#58382,#58383,#58384,
#58385,#58386,#58387,#58388,#58389,#58390),.UNSPECIFIED.,.F.,.F.,(4,3,3,
3,3,3,3,4),(-104.623895335004,-104.245062404611,-103.252252286472,-102.259442168333,
-101.266632050194,-100.273821932054,-99.2810118139153,-98.3407100278245),
 .UNSPECIFIED.);
#1401=B_SPLINE_CURVE_WITH_KNOTS('',3,(#58391,#58392,#58393,#58394,#58395,
#58396,#58397,#58398,#58399,#58400,#58401,#58402,#58403,#58404,#58405,#58406,
#58407,#58408,#58409,#58410,#58411,#58412),.UNSPECIFIED.,.F.,.F.,(4,3,3,
3,3,3,3,4),(95.365080016062,96.3025814594978,97.295391577637,98.2882016957761,
99.2810118139153,100.273821932054,101.266632050194,101.648265323242),
 .UNSPECIFIED.);
#1402=B_SPLINE_CURVE_WITH_KNOTS('',3,(#58417,#58418,#58419,#58420,#58421,
#58422,#58423,#58424,#58425,#58426,#58427,#58428,#58429,#58430,#58431,#58432,
#58433,#58434,#58435,#58436,#58437,#58438),.UNSPECIFIED.,.F.,.F.,(4,3,3,
3,3,3,3,4),(-110.907080642184,-110.201923113446,-109.209112995307,-108.216302877168,
-107.223492759029,-106.230682640889,-105.23787252275,-104.623895335004),
 .UNSPECIFIED.);
#1403=B_SPLINE_CURVE_WITH_KNOTS('',3,(#58439,#58440,#58441,#58442,#58443,
#58444,#58445,#58446,#58447,#58448,#58449,#58450,#58451,#58452,#58453,#58454,
#58455,#58456,#58457,#58458,#58459,#58460),.UNSPECIFIED.,.F.,.F.,(4,3,3,
3,3,3,3,4),(101.648265323242,102.259442168333,103.252252286472,104.245062404611,
105.23787252275,106.230682640889,107.223492759029,107.931450630421),
 .UNSPECIFIED.);
#1404=B_SPLINE_CURVE_WITH_KNOTS('',3,(#58466,#58467,#58468,#58469,#58470,
#58471),.UNSPECIFIED.,.F.,.F.,(4,1,1,4),(122.522113490002,122.809766079403,
123.802576197542,124.712368377051),.UNSPECIFIED.);
#1405=B_SPLINE_CURVE_WITH_KNOTS('',3,(#58474,#58475,#58476,#58477),
 .UNSPECIFIED.,.F.,.F.,(4,4),(122.522113490002,123.473451256543),
 .UNSPECIFIED.);
#1406=B_SPLINE_CURVE_WITH_KNOTS('',3,(#58482,#58483,#58484,#58485,#58486,
#58487,#58488,#58489,#58490,#58491),.UNSPECIFIED.,.F.,.F.,(4,1,1,1,1,1,
1,4),(116.238928182822,116.852905370568,117.845715488708,118.838525606847,
119.831335724986,120.824145843125,121.816955961264,122.522113490002),
 .UNSPECIFIED.);
#1407=B_SPLINE_CURVE_WITH_KNOTS('',3,(#58492,#58493,#58494,#58495,#58496,
#58497,#58498,#58499,#58500,#58501,#58502),.UNSPECIFIED.,.F.,.F.,(4,1,1,
1,1,1,1,1,4),(116.238928182822,116.523780429569,117.516590547708,118.509400665847,
119.502210783986,120.495020902125,121.487831020264,122.480641138404,122.522113490002),
 .UNSPECIFIED.);
#1408=B_SPLINE_CURVE_WITH_KNOTS('',3,(#58507,#58508,#58509,#58510,#58511,
#58512,#58513,#58514,#58515,#58516),.UNSPECIFIED.,.F.,.F.,(4,1,1,1,1,1,
1,4),(109.955742875643,110.896044661733,111.888854779873,112.881664898012,
113.874475016151,114.86728513429,115.860095252429,116.238928182822),
 .UNSPECIFIED.);
#1409=B_SPLINE_CURVE_WITH_KNOTS('',3,(#58517,#58518,#58519,#58520,#58521,
#58522,#58523,#58524,#58525,#58526),.UNSPECIFIED.,.F.,.F.,(4,1,1,1,1,1,
1,4),(109.955742875643,110.566919720734,111.559729838873,112.552539957012,
113.545350075151,114.53816019329,115.530970311429,116.238928182822),
 .UNSPECIFIED.);
#1410=B_SPLINE_CURVE_WITH_KNOTS('',3,(#58531,#58532,#58533,#58534,#58535,
#58536,#58537,#58538,#58539,#58540,#58541),.UNSPECIFIED.,.F.,.F.,(4,1,1,
1,1,1,1,1,4),(103.672557568463,103.946373834759,104.939183952899,105.931994071038,
106.924804189177,107.917614307316,108.910424425455,109.903234543594,109.955742875643),
 .UNSPECIFIED.);
#1411=B_SPLINE_CURVE_WITH_KNOTS('',3,(#58542,#58543,#58544,#58545,#58546,
#58547,#58548,#58549,#58550,#58551),.UNSPECIFIED.,.F.,.F.,(4,1,1,1,1,1,
1,4),(103.672557568463,104.610059011899,105.602869130038,106.595679248177,
107.588489366316,108.581299484455,109.574109602595,109.955742875643),
 .UNSPECIFIED.);
#1412=B_SPLINE_CURVE_WITH_KNOTS('',3,(#58556,#58557,#58558,#58559,#58560,
#58561,#58562,#58563,#58564,#58565),.UNSPECIFIED.,.F.,.F.,(4,1,1,1,1,1,
1,4),(97.3893722612836,97.9895131259245,98.9823232440636,99.9751333622028,
100.967943480342,101.960753598481,102.95356371662,103.672557568463),
 .UNSPECIFIED.);
#1413=B_SPLINE_CURVE_WITH_KNOTS('',3,(#58566,#58567,#58568,#58569,#58570,
#58571,#58572,#58573,#58574,#58575,#58576),.UNSPECIFIED.,.F.,.F.,(4,1,1,
1,1,1,1,1,4),(97.3893722612835,97.6603881849247,98.6531983030639,99.646008421203,
100.638818539342,101.631628657481,102.624438775621,103.61724889376,103.672557568463),
 .UNSPECIFIED.);
#1414=B_SPLINE_CURVE_WITH_KNOTS('',3,(#58581,#58582,#58583,#58584,#58585,
#58586,#58587,#58588,#58589,#58590),.UNSPECIFIED.,.F.,.F.,(4,1,1,1,1,1,
1,4),(91.106186954104,92.0326524170896,93.0254625352287,94.0182726533679,
95.011082771507,96.0038928896462,96.9967030077853,97.3893722612836),
 .UNSPECIFIED.);
#1415=B_SPLINE_CURVE_WITH_KNOTS('',3,(#58591,#58592,#58593,#58594,#58595,
#58596,#58597,#58598,#58599,#58600),.UNSPECIFIED.,.F.,.F.,(4,1,1,1,1,1,
1,4),(91.106186954104,91.7035274760898,92.696337594229,93.6891477123681,
94.6819578305073,95.6747679486464,96.6675780667856,97.3893722612835),
 .UNSPECIFIED.);
#1416=B_SPLINE_CURVE_WITH_KNOTS('',3,(#58605,#58606,#58607,#58608,#58609,
#58610,#58611,#58612,#58613,#58614,#58615),.UNSPECIFIED.,.F.,.F.,(4,1,1,
1,1,1,1,1,4),(84.8230016469244,85.0829815901155,86.0757917082546,87.0686018263938,
88.0614119445329,89.0542220626721,90.0470321808113,91.0398422989504,91.106186954104),
 .UNSPECIFIED.);
#1417=B_SPLINE_CURVE_WITH_KNOTS('',3,(#58616,#58617,#58618,#58619,#58620,
#58621,#58622,#58623,#58624,#58625),.UNSPECIFIED.,.F.,.F.,(4,1,1,1,1,1,
1,4),(84.8230016469244,85.7466667672549,86.7394768853941,87.7322870035332,
88.7250971216724,89.7179072398115,90.7107173579507,91.106186954104),
 .UNSPECIFIED.);
#1418=B_SPLINE_CURVE_WITH_KNOTS('',3,(#58630,#58631,#58632,#58633,#58634,
#58635,#58636,#58637,#58638,#58639),.UNSPECIFIED.,.F.,.F.,(4,1,1,1,1,1,
1,4),(78.5398163397448,79.1261208812806,80.1189309994197,81.1117411175589,
82.104551235698,83.0973613538372,84.0901714719763,84.8230016469244),
 .UNSPECIFIED.);
#1419=B_SPLINE_CURVE_WITH_KNOTS('',3,(#58640,#58641,#58642,#58643,#58644,
#58645,#58646,#58647,#58648,#58649,#58650),.UNSPECIFIED.,.F.,.F.,(4,1,1,
1,1,1,1,1,4),(78.5398163397448,78.7969959402808,79.78980605842,80.7826161765591,
81.7754262946983,82.7682364128375,83.7610465309766,84.7538566491157,84.8230016469244),
 .UNSPECIFIED.);
#1420=B_SPLINE_CURVE_WITH_KNOTS('',3,(#58655,#58656,#58657,#58658,#58659,
#58660,#58661,#58662,#58663,#58664),.UNSPECIFIED.,.F.,.F.,(4,1,1,1,1,1,
1,4),(72.2566310325652,73.1692601724456,74.1620702905848,75.154880408724,
76.1476905268631,77.1405006450023,78.1333107631414,78.5398163397448),
 .UNSPECIFIED.);
#1421=B_SPLINE_CURVE_WITH_KNOTS('',3,(#58665,#58666,#58667,#58668,#58669,
#58670,#58671,#58672,#58673,#58674),.UNSPECIFIED.,.F.,.F.,(4,1,1,1,1,1,
1,4),(72.2566310325652,72.8401352314459,73.8329453495851,74.8257554677242,
75.8185655858634,76.8113757040025,77.8041858221417,78.5398163397448),
 .UNSPECIFIED.);
#1422=B_SPLINE_CURVE_WITH_KNOTS('',3,(#58679,#58680,#58681,#58682,#58683,
#58684,#58685,#58686,#58687,#58688,#58689),.UNSPECIFIED.,.F.,.F.,(4,1,1,
1,1,1,1,1,4),(65.9734457253856,66.2195893454716,67.2123994636107,68.2052095817499,
69.198019699889,70.1908298180282,71.1836399361674,72.1764500543065,72.2566310325652),
 .UNSPECIFIED.);
#1423=B_SPLINE_CURVE_WITH_KNOTS('',3,(#58690,#58691,#58692,#58693,#58694,
#58695,#58696,#58697,#58698,#58699),.UNSPECIFIED.,.F.,.F.,(4,1,1,1,1,1,
1,4),(65.9734457253856,66.883274522611,67.8760846407502,68.8688947588893,
69.8617048770285,70.8545149951676,71.8473251133068,72.2566310325652),
 .UNSPECIFIED.);
#1424=B_SPLINE_CURVE_WITH_KNOTS('',3,(#58704,#58705,#58706,#58707,#58708,
#58709,#58710,#58711,#58712,#58713),.UNSPECIFIED.,.F.,.F.,(4,1,1,1,1,1,
1,4),(59.690260418206,60.2627286366367,61.2555387547758,62.248348872915,
63.2411589910541,64.2339691091933,65.2267792273324,65.9734457253856),
 .UNSPECIFIED.);
#1425=B_SPLINE_CURVE_WITH_KNOTS('',3,(#58714,#58715,#58716,#58717,#58718,
#58719,#58720,#58721,#58722,#58723,#58724),.UNSPECIFIED.,.F.,.F.,(4,1,1,
1,1,1,1,1,4),(59.690260418206,59.9336036956369,60.9264138137761,61.9192239319152,
62.9120340500544,63.9048441681935,64.8976542863327,65.8904644044719,65.9734457253856),
 .UNSPECIFIED.);
#1426=B_SPLINE_CURVE_WITH_KNOTS('',3,(#58729,#58730,#58731,#58732,#58733,
#58734,#58735,#58736,#58737,#58738),.UNSPECIFIED.,.F.,.F.,(4,1,1,1,1,1,
1,4),(53.4070751110264,54.3058679278017,55.2986780459409,56.2914881640801,
57.2842982822192,58.2771084003584,59.2699185184975,59.690260418206),
 .UNSPECIFIED.);
#1427=B_SPLINE_CURVE_WITH_KNOTS('',3,(#58739,#58740,#58741,#58742,#58743,
#58744,#58745,#58746,#58747,#58748),.UNSPECIFIED.,.F.,.F.,(4,1,1,1,1,1,
1,4),(53.4070751110264,53.976742986802,54.9695531049412,55.9623632230803,
56.9551733412195,57.9479834593586,58.9407935774978,59.690260418206),
 .UNSPECIFIED.);
#1428=B_SPLINE_CURVE_WITH_KNOTS('',3,(#58753,#58754,#58755,#58756,#58757,
#58758,#58759,#58760,#58761,#58762,#58763),.UNSPECIFIED.,.F.,.F.,(4,1,1,
1,1,1,1,1,4),(47.1238898038468,47.3561971008277,48.3490072189668,49.341817337106,
50.3346274552451,51.3274375733843,52.3202476915234,53.3130578096626,53.4070751110264),
 .UNSPECIFIED.);
#1429=B_SPLINE_CURVE_WITH_KNOTS('',3,(#58764,#58765,#58766,#58767,#58768,
#58769,#58770,#58771,#58772,#58773),.UNSPECIFIED.,.F.,.F.,(4,1,1,1,1,1,
1,4),(47.1238898038468,48.0198822779671,49.0126923961063,50.0055025142454,
50.9983126323846,51.9911227505237,52.9839328686629,53.4070751110264),
 .UNSPECIFIED.);
#1430=B_SPLINE_CURVE_WITH_KNOTS('',3,(#58778,#58779,#58780,#58781,#58782,
#58783,#58784,#58785,#58786,#58787),.UNSPECIFIED.,.F.,.F.,(4,1,1,1,1,1,
1,4),(40.8407044966672,41.3993363919928,42.3921465101319,43.3849566282711,
44.3777667464102,45.3705768645494,46.3633869826885,47.1238898038468),
 .UNSPECIFIED.);
#1431=B_SPLINE_CURVE_WITH_KNOTS('',3,(#58788,#58789,#58790,#58791,#58792,
#58793,#58794,#58795,#58796,#58797,#58798),.UNSPECIFIED.,.F.,.F.,(4,1,1,
1,1,1,1,1,4),(40.8407044966672,41.070211450993,42.0630215691322,43.0558316872713,
44.0486418054105,45.0414519235496,46.0342620416888,47.0270721598279,47.1238898038468),
 .UNSPECIFIED.);
#1432=B_SPLINE_CURVE_WITH_KNOTS('',3,(#58803,#58804,#58805,#58806,#58807,
#58808,#58809,#58810,#58811,#58812),.UNSPECIFIED.,.F.,.F.,(4,1,1,1,1,1,
1,4),(34.5575191894876,35.4424756831578,36.435285801297,37.4280959194362,
38.4209060375753,39.4137161557145,40.4065262738536,40.8407044966672),
 .UNSPECIFIED.);
#1433=B_SPLINE_CURVE_WITH_KNOTS('',3,(#58813,#58814,#58815,#58816,#58817,
#58818,#58819,#58820,#58821,#58822),.UNSPECIFIED.,.F.,.F.,(4,1,1,1,1,1,
1,4),(34.5575191894876,35.1133507421581,36.1061608602973,37.0989709784364,
38.0917810965756,39.0845912147147,40.0774013328539,40.8407044966672),
 .UNSPECIFIED.);
#1434=B_SPLINE_CURVE_WITH_KNOTS('',3,(#58827,#58828,#58829,#58830,#58831,
#58832,#58833,#58834,#58835,#58836,#58837),.UNSPECIFIED.,.F.,.F.,(4,1,1,
1,1,1,1,1,4),(28.2743338823081,28.4928048561838,29.4856149743229,30.4784250924621,
31.4712352106012,32.4640453287404,33.4568554468795,34.4496655650187,34.5575191894876),
 .UNSPECIFIED.);
#1435=B_SPLINE_CURVE_WITH_KNOTS('',3,(#58838,#58839,#58840,#58841,#58842,
#58843,#58844,#58845,#58846,#58847),.UNSPECIFIED.,.F.,.F.,(4,1,1,1,1,1,
1,4),(28.274333882308,29.1564900333232,30.1493001514623,31.1421102696015,
32.1349203877406,33.1277305058798,34.120540624019,34.5575191894876),
 .UNSPECIFIED.);
#1436=B_SPLINE_CURVE_WITH_KNOTS('',3,(#58852,#58853,#58854,#58855,#58856,
#58857,#58858,#58859,#58860,#58861),.UNSPECIFIED.,.F.,.F.,(4,1,1,1,1,1,
1,4),(21.9911485751285,22.5359441473489,23.528754265488,24.5215643836272,
25.5143745017663,26.5071846199055,27.4999947380446,28.2743338823081),
 .UNSPECIFIED.);
#1437=B_SPLINE_CURVE_WITH_KNOTS('',3,(#58862,#58863,#58864,#58865,#58866,
#58867,#58868,#58869,#58870,#58871,#58872),.UNSPECIFIED.,.F.,.F.,(4,1,1,
1,1,1,1,1,4),(21.9911485751284,22.2068192063491,23.1996293244883,24.1924394426274,
25.1852495607666,26.1780596789057,27.1708697970449,28.163679915184,28.274333882308),
 .UNSPECIFIED.);
#1438=B_SPLINE_CURVE_WITH_KNOTS('',3,(#58877,#58878,#58879,#58880,#58881,
#58882,#58883,#58884,#58885,#58886),.UNSPECIFIED.,.F.,.F.,(4,1,1,1,1,1,
1,4),(15.7079632679489,16.5790834385139,17.5718935566531,18.5647036747922,
19.5575137929314,20.5503239110706,21.5431340292097,21.9911485751285),
 .UNSPECIFIED.);
#1439=B_SPLINE_CURVE_WITH_KNOTS('',3,(#58887,#58888,#58889,#58890,#58891,
#58892,#58893,#58894,#58895,#58896),.UNSPECIFIED.,.F.,.F.,(4,1,1,1,1,1,
1,4),(15.7079632679489,16.2499584975142,17.2427686156534,18.2355787337925,
19.2283888519317,20.2211989700708,21.21400908821,21.9911485751284),
 .UNSPECIFIED.);
#1440=B_SPLINE_CURVE_WITH_KNOTS('',3,(#59411,#59412,#59413,#59414,#59415,
#59416,#59417,#59418,#59419,#59420,#59421,#59422,#59423,#59424,#59425,#59426,
#59427,#59428,#59429,#59430,#59431,#59432,#59433,#59434,#59435,#59436,#59437,
#59438,#59439,#59440,#59441,#59442,#59443,#59444,#59445,#59446,#59447,#59448,
#59449,#59450,#59451,#59452,#59453,#59454,#59455,#59456,#59457,#59458,#59459,
#59460,#59461,#59462,#59463,#59464,#59465,#59466,#59467,#59468,#59469,#59470,
#59471,#59472,#59473,#59474,#59475,#59476,#59477,#59478,#59479,#59480,#59481,
#59482,#59483,#59484,#59485,#59486,#59487,#59488,#59489,#59490,#59491,#59492,
#59493,#59494,#59495,#59496,#59497,#59498,#59499,#59500,#59501),
 .UNSPECIFIED.,.F.,.F.,(4,3,3,3,3,3,3,3,3,3,3,3,3,3,3,3,3,3,3,3,3,3,3,3,
3,3,3,3,3,3,4),(0.,0.0244828275480345,0.053633229323616,0.0831948315675068,
0.110714477628582,0.11526672716195,0.144013775177923,0.172670364792843,
0.200834260795346,0.213648978202941,0.219194492985043,0.223573650231945,
0.251155465393894,0.277944800071433,0.303352000056106,0.319097049327563,
0.323930180875061,0.328014801185161,0.354666699599173,0.38176869329296,
0.408582656634786,0.419018395384968,0.42428937677764,0.428315007817544,
0.454631255061835,0.479791638396231,0.488289756370224,0.494557171122132,
0.519833104861304,0.544394958619519,0.555272788399418),.UNSPECIFIED.);
#1441=B_SPLINE_CURVE_WITH_KNOTS('',3,(#59502,#59503,#59504,#59505,#59506,
#59507,#59508,#59509,#59510,#59511,#59512,#59513,#59514,#59515,#59516,#59517,
#59518,#59519,#59520),.UNSPECIFIED.,.F.,.F.,(4,3,3,3,3,3,4),(107.931450630421,
108.216302877168,109.209112995307,110.201923113446,111.194733231585,112.187543349724,
113.097335529233),.UNSPECIFIED.);
#1442=B_SPLINE_CURVE_WITH_KNOTS('',3,(#59522,#59523,#59524,#59525,#59526,
#59527,#59528,#59529,#59530,#59531,#59532,#59533,#59534,#59535,#59536,#59537,
#59538,#59539,#59540,#59541,#59542,#59543,#59544,#59545,#59546,#59547,#59548,
#59549,#59550,#59551,#59552,#59553,#59554,#59555,#59556,#59557,#59558,#59559,
#59560,#59561,#59562,#59563,#59564,#59565,#59566,#59567,#59568,#59569,#59570,
#59571,#59572,#59573,#59574,#59575,#59576,#59577,#59578,#59579,#59580,#59581,
#59582,#59583,#59584,#59585,#59586,#59587,#59588,#59589,#59590,#59591,#59592,
#59593,#59594,#59595,#59596,#59597,#59598,#59599,#59600,#59601,#59602,#59603,
#59604,#59605,#59606,#59607,#59608,#59609,#59610,#59611,#59612),
 .UNSPECIFIED.,.F.,.F.,(4,3,3,3,3,3,3,3,3,3,3,3,3,3,3,3,3,3,3,3,3,3,3,3,
3,3,3,3,3,3,4),(0.,0.0199484555424935,0.0444472219322248,0.0695704352965358,
0.0823017670372087,0.0889067669075885,0.0939032261859449,0.0978868073317507,
0.123848521149104,0.150333670415753,0.177012130518808,0.190045367541077,
0.195034003771074,0.222448330986507,0.249798458203261,0.273271743147302,
0.290738845349037,0.295003687011922,0.321757479861748,0.350630967175911,
0.377214736980723,0.389091550177083,0.398269541876197,0.403901739635534,
0.432677759684221,0.462694664356929,0.472448461766916,0.479349706952298,
0.508919877152419,0.538123179131352,0.552745378375053),.UNSPECIFIED.);
#1443=B_SPLINE_CURVE_WITH_KNOTS('',3,(#59613,#59614,#59615,#59616,#59617,
#59618,#59619,#59620,#59621),.UNSPECIFIED.,.F.,.F.,(4,1,1,1,1,1,4),(10.3761157273101,
11.2859079068184,12.2787180249576,13.2715281430967,14.2643382612359,15.2571483793751,
15.7079632679489),.UNSPECIFIED.);
#1444=B_SPLINE_CURVE_WITH_KNOTS('',3,(#59625,#59626,#59627,#59628,#59629,
#59630,#59631,#59632),.UNSPECIFIED.,.F.,.F.,(4,1,1,1,1,4),(11.6150328478182,
12.6078429659573,13.6006530840965,14.5934632022356,15.5862733203748,15.7079632679489),
 .UNSPECIFIED.);
#1445=B_SPLINE_CURVE_WITH_KNOTS('',3,(#60110,#60111,#60112,#60113,#60114,
#60115,#60116,#60117,#60118,#60119,#60120,#60121,#60122,#60123,#60124,#60125,
#60126,#60127,#60128,#60129,#60130,#60131,#60132,#60133,#60134,#60135,#60136,
#60137,#60138,#60139,#60140,#60141,#60142,#60143,#60144,#60145,#60146,#60147,
#60148,#60149,#60150,#60151,#60152,#60153,#60154,#60155,#60156,#60157,#60158,
#60159,#60160,#60161,#60162,#60163,#60164,#60165,#60166,#60167,#60168,#60169,
#60170,#60171,#60172,#60173,#60174,#60175,#60176,#60177,#60178,#60179,#60180,
#60181,#60182,#60183,#60184,#60185,#60186,#60187,#60188,#60189,#60190,#60191,
#60192,#60193,#60194,#60195,#60196,#60197,#60198,#60199,#60200),
 .UNSPECIFIED.,.F.,.F.,(4,3,3,3,3,3,3,3,3,3,3,3,3,3,3,3,3,3,3,3,3,3,3,3,
3,3,3,3,3,3,4),(0.,0.0199484555424956,0.0444472057453558,0.06957040842524,
0.082301741845369,0.0889067201937656,0.0939032092701117,0.0978868025698804,
0.123848506283839,0.150333651753478,0.177012112338214,0.190045334010802,
0.195033995567435,0.222448321497137,0.249798448556615,0.273271743147304,
0.290738845349038,0.295003687474005,0.321757477096169,0.35063096475603,
0.377214805322132,0.389091676062608,0.398269949867563,0.403901905426966,
0.432677921570632,0.462694785771738,0.472448780080044,0.479349722651653,
0.508919892898584,0.538123208459607,0.552745378375058),.UNSPECIFIED.);
#1446=B_SPLINE_CURVE_WITH_KNOTS('',3,(#60201,#60202,#60203,#60204,#60205,
#60206,#60207,#60208,#60209,#60210,#60211,#60212,#60213,#60214,#60215,#60216,
#60217,#60218,#60219,#60220,#60221,#60222,#60223,#60224,#60225,#60226,#60227,
#60228,#60229,#60230,#60231,#60232,#60233,#60234,#60235,#60236,#60237,#60238,
#60239,#60240,#60241,#60242,#60243,#60244,#60245,#60246,#60247,#60248,#60249,
#60250,#60251,#60252,#60253,#60254,#60255,#60256,#60257,#60258,#60259,#60260,
#60261,#60262,#60263,#60264,#60265,#60266,#60267,#60268,#60269,#60270,#60271,
#60272,#60273,#60274,#60275,#60276,#60277,#60278,#60279,#60280,#60281,#60282,
#60283,#60284,#60285,#60286,#60287,#60288,#60289,#60290,#60291),
 .UNSPECIFIED.,.F.,.F.,(4,3,3,3,3,3,3,3,3,3,3,3,3,3,3,3,3,3,3,3,3,3,3,3,
3,3,3,3,3,3,4),(0.,0.0244828275480203,0.0536332274622602,0.0831948298811238,
0.110714476152993,0.115266725820044,0.144013773894134,0.172670359523596,
0.20083424455867,0.213648963995846,0.219194447131387,0.223573639079567,
0.251155446612606,0.277944764436798,0.303352000056074,0.31909704932753,
0.323930181275963,0.328014801994789,0.354666688633115,0.381768683952949,
0.408582659874698,0.419018397971995,0.424289394077547,0.428315034389049,
0.454631289457757,0.479791664193159,0.488289819943521,0.494557177833865,
0.519833128909889,0.544395005481118,0.555272788399364),.UNSPECIFIED.);
#1447=B_SPLINE_CURVE_WITH_KNOTS('',3,(#60292,#60293,#60294,#60295,#60296,
#60297,#60298,#60299,#60300,#60301,#60302,#60303,#60304,#60305,#60306,#60307),
 .UNSPECIFIED.,.F.,.F.,(4,3,3,3,3,4),(-115.165973704142,-114.173163586003,
-113.180353467863,-112.187543349724,-111.194733231585,-110.907080642184),
 .UNSPECIFIED.);
#1448=B_SPLINE_CURVE_WITH_KNOTS('',3,(#60434,#60435,#60436,#60437,#60438,
#60439,#60440,#60441,#60442,#60443,#60444,#60445,#60446,#60447,#60448,#60449,
#60450,#60451,#60452,#60453,#60454,#60455,#60456,#60457,#60458,#60459),
 .UNSPECIFIED.,.F.,.F.,(4,2,2,2,2,2,2,2,2,2,2,2,4),(-1.71701449155744,-1.52195735713249,
-1.32690022270754,-1.23846982832783,-1.15003943394813,-1.00427333986342,
-0.858507245778717,-0.712741151694014,-0.56697505760931,-0.478544663229604,
-0.390114268849898,-0.195057134424949,0.),.UNSPECIFIED.);
#1449=B_SPLINE_CURVE_WITH_KNOTS('',3,(#60463,#60464,#60465,#60466,#60467,
#60468,#60469,#60470,#60471,#60472,#60473,#60474),.UNSPECIFIED.,.F.,.F.,
(4,2,2,2,2,4),(-0.73325034842368,-0.710785333485644,-0.57603622531241,-0.432027168984308,
-0.288018112656205,0.),.UNSPECIFIED.);
#1450=B_SPLINE_CURVE_WITH_KNOTS('',3,(#60478,#60479,#60480,#60481,#60482,
#60483,#60484,#60485,#60486,#60487,#60488,#60489,#60490,#60491),
 .UNSPECIFIED.,.F.,.F.,(4,2,2,2,2,2,4),(-1.69106888331775,-1.40305077066155,
-1.25904171433345,-1.11503265800535,-0.980283549832111,-0.845534441658878,
-0.73325034842368),.UNSPECIFIED.);
#1451=B_SPLINE_CURVE_WITH_KNOTS('',3,(#60499,#60500,#60501,#60502,#60503,
#60504,#60505,#60506,#60507,#60508,#60509,#60510),.UNSPECIFIED.,.F.,.F.,
(4,2,2,2,2,4),(-0.845534441658877,-0.710785333485644,-0.576036225312411,
-0.432027168984308,-0.288018112656205,0.),.UNSPECIFIED.);
#1452=B_SPLINE_CURVE_WITH_KNOTS('',3,(#60514,#60515,#60516,#60517,#60518,
#60519,#60520,#60521,#60522,#60523,#60524,#60525,#60526,#60527,#60528,#60529,
#60530,#60531,#60532,#60533,#60534,#60535),.UNSPECIFIED.,.F.,.F.,(4,2,2,
2,2,2,2,2,2,2,4),(-1.69106888331776,-1.40305077066155,-1.25904171433345,
-1.11503265800535,-0.980283549832111,-0.845534441658878,-0.710785333485644,
-0.57603622531241,-0.432027168984307,-0.288018112656205,0.),
 .UNSPECIFIED.);
#1453=B_SPLINE_CURVE_WITH_KNOTS('',3,(#60539,#60540,#60541,#60542,#60543,
#60544,#60545,#60546,#60547,#60548,#60549,#60550,#60551,#60552,#60553,#60554,
#60555,#60556,#60557,#60558,#60559,#60560),.UNSPECIFIED.,.F.,.F.,(4,2,2,
2,2,2,2,2,2,2,4),(-1.69106888331776,-1.40305077066155,-1.25904171433345,
-1.11503265800535,-0.980283549832111,-0.845534441658878,-0.710785333485644,
-0.57603622531241,-0.432027168984307,-0.288018112656205,0.),
 .UNSPECIFIED.);
#1454=B_SPLINE_CURVE_WITH_KNOTS('',3,(#60564,#60565,#60566,#60567,#60568,
#60569,#60570,#60571,#60572,#60573,#60574,#60575,#60576,#60577,#60578,#60579,
#60580,#60581,#60582,#60583,#60584,#60585),.UNSPECIFIED.,.F.,.F.,(4,2,2,
2,2,2,2,2,2,2,4),(-1.69106888331775,-1.40305077066155,-1.25904171433345,
-1.11503265800534,-0.980283549832111,-0.845534441658877,-0.710785333485644,
-0.57603622531241,-0.432027168984307,-0.288018112656205,0.),
 .UNSPECIFIED.);
#1455=B_SPLINE_CURVE_WITH_KNOTS('',3,(#60589,#60590,#60591,#60592,#60593,
#60594),.UNSPECIFIED.,.F.,.F.,(4,2,4),(-1.69106888331776,-1.40305077066155,
-1.27424252614337),.UNSPECIFIED.);
#1456=B_SPLINE_CURVE_WITH_KNOTS('',3,(#60596,#60597,#60598,#60599,#60600,
#60601,#60602,#60603,#60604,#60605,#60606,#60607,#60608,#60609,#60610,#60611,
#60612,#60613,#60614,#60615),.UNSPECIFIED.,.F.,.F.,(4,2,2,2,2,2,2,2,2,4),
(-1.27424252614337,-1.25904171433345,-1.11503265800534,-0.980283549832111,
-0.845534441658877,-0.710785333485643,-0.576036225312409,-0.432027168984307,
-0.288018112656205,0.),.UNSPECIFIED.);
#1457=B_SPLINE_CURVE_WITH_KNOTS('',3,(#60619,#60620,#60621,#60622,#60623,
#60624,#60625,#60626,#60627,#60628,#60629,#60630),.UNSPECIFIED.,.F.,.F.,
(4,2,2,2,2,4),(-1.69106888331776,-1.40305077066155,-1.25904171433345,-1.11503265800534,
-0.980283549832111,-0.957818534894075),.UNSPECIFIED.);
#1458=B_SPLINE_CURVE_WITH_KNOTS('',3,(#60632,#60633,#60634,#60635,#60636,
#60637,#60638,#60639,#60640,#60641,#60642,#60643,#60644,#60645),
 .UNSPECIFIED.,.F.,.F.,(4,2,2,2,2,2,4),(-0.957818534894075,-0.845534441658877,
-0.710785333485644,-0.57603622531241,-0.432027168984307,-0.288018112656205,
0.),.UNSPECIFIED.);
#1459=B_SPLINE_CURVE_WITH_KNOTS('',3,(#60649,#60650,#60651,#60652,#60653,
#60654,#60655,#60656,#60657,#60658,#60659,#60660),.UNSPECIFIED.,.F.,.F.,
(4,2,2,2,2,4),(-1.69106888331776,-1.40305077066155,-1.25904171433345,-1.11503265800535,
-0.980283549832111,-0.845534441658878),.UNSPECIFIED.);
#1460=B_SPLINE_CURVE_WITH_KNOTS('',3,(#60662,#60663,#60664,#60665,#60666,
#60667,#60668,#60669,#60670,#60671,#60672,#60673),.UNSPECIFIED.,.F.,.F.,
(4,2,2,2,2,4),(-0.845534441658878,-0.710785333485644,-0.57603622531241,
-0.432027168984308,-0.288018112656205,0.),.UNSPECIFIED.);
#1461=B_SPLINE_CURVE_WITH_KNOTS('',3,(#60678,#60679,#60680,#60681,#60682,
#60683,#60684,#60685,#60686,#60687,#60688,#60689,#60690,#60691,#60692,#60693,
#60694,#60695,#60696,#60697),.UNSPECIFIED.,.F.,.F.,(4,2,2,2,2,2,2,2,2,4),
(-1.69106888331775,-1.40305077066155,-1.25904171433345,-1.11503265800535,
-0.980283549832112,-0.845534441658878,-0.710785333485644,-0.57603622531241,
-0.432027168984308,-0.416826357174388),.UNSPECIFIED.);
#1462=B_SPLINE_CURVE_WITH_KNOTS('',3,(#60699,#60700,#60701,#60702,#60703,
#60704),.UNSPECIFIED.,.F.,.F.,(4,2,4),(-0.416826357174388,-0.288018112656205,
0.),.UNSPECIFIED.);
#1463=B_SPLINE_CURVE_WITH_KNOTS('',3,(#60708,#60709,#60710,#60711,#60712,
#60713,#60714,#60715,#60716,#60717,#60718,#60719,#60720,#60721,#60722,#60723,
#60724,#60725,#60726,#60727,#60728,#60729),.UNSPECIFIED.,.F.,.F.,(4,2,2,
2,2,2,2,2,2,2,4),(-1.69106888331776,-1.40305077066155,-1.25904171433345,
-1.11503265800535,-0.980283549832111,-0.845534441658878,-0.710785333485644,
-0.576036225312411,-0.432027168984308,-0.288018112656205,0.),
 .UNSPECIFIED.);
#1464=B_SPLINE_CURVE_WITH_KNOTS('',3,(#60733,#60734,#60735,#60736,#60737,
#60738,#60739,#60740,#60741,#60742,#60743,#60744,#60745,#60746,#60747,#60748,
#60749,#60750,#60751,#60752,#60753,#60754),.UNSPECIFIED.,.F.,.F.,(4,2,2,
2,2,2,2,2,2,2,4),(-1.69106888331776,-1.40305077066155,-1.25904171433345,
-1.11503265800535,-0.980283549832111,-0.845534441658878,-0.710785333485644,
-0.57603622531241,-0.432027168984308,-0.288018112656205,0.),
 .UNSPECIFIED.);
#1465=B_SPLINE_CURVE_WITH_KNOTS('',3,(#60758,#60759,#60760,#60761,#60762,
#60763,#60764,#60765,#60766,#60767,#60768,#60769,#60770,#60771,#60772,#60773,
#60774,#60775,#60776,#60777,#60778,#60779),.UNSPECIFIED.,.F.,.F.,(4,2,2,
2,2,2,2,2,2,2,4),(-1.69106888331776,-1.40305077066155,-1.25904171433345,
-1.11503265800535,-0.980283549832113,-0.845534441658879,-0.710785333485645,
-0.576036225312412,-0.432027168984308,-0.288018112656206,0.),
 .UNSPECIFIED.);
#1466=B_SPLINE_CURVE_WITH_KNOTS('',3,(#60782,#60783,#60784,#60785,#60786,
#60787,#60788,#60789,#60790,#60791,#60792,#60793),.UNSPECIFIED.,.F.,.F.,
(4,2,2,2,2,4),(-1.69106888331776,-1.40305077066155,-1.25904171433345,-1.11503265800535,
-0.980283549832112,-0.845534441658877),.UNSPECIFIED.);
#1467=B_SPLINE_CURVE_WITH_KNOTS('',3,(#60800,#60801,#60802,#60803,#60804,
#60805,#60806,#60807,#60808,#60809,#60810,#60811,#60812,#60813,#60814,#60815,
#60816,#60817,#60818,#60819,#60820,#60821,#60822,#60823,#60824,#60825),
 .UNSPECIFIED.,.F.,.F.,(4,2,2,2,2,2,2,2,2,2,2,2,4),(-1.71701449155743,-1.52195735713249,
-1.32690022270754,-1.23846982832783,-1.15003943394812,-1.00427333986342,
-0.858507245778717,-0.712741151694013,-0.56697505760931,-0.478544663229604,
-0.390114268849898,-0.195057134424949,0.),.UNSPECIFIED.);
#1468=B_SPLINE_CURVE_WITH_KNOTS('',3,(#60835,#60836,#60837,#60838,#60839,
#60840,#60841,#60842,#60843,#60844,#60845,#60846,#60847,#60848,#60849,#60850,
#60851,#60852,#60853,#60854,#60855,#60856,#60857,#60858,#60859,#60860),
 .UNSPECIFIED.,.F.,.F.,(4,2,2,2,2,2,2,2,2,2,2,2,4),(-1.71701449155744,-1.52195735713249,
-1.32690022270754,-1.23846982832783,-1.15003943394812,-1.00427333986342,
-0.858507245778718,-0.712741151694014,-0.56697505760931,-0.478544663229604,
-0.390114268849898,-0.195057134424949,0.),.UNSPECIFIED.);
#1469=B_SPLINE_CURVE_WITH_KNOTS('',3,(#60873,#60874,#60875,#60876,#60877,
#60878,#60879,#60880,#60881,#60882),.UNSPECIFIED.,.F.,.F.,(4,2,2,2,4),(-1.71701449155744,
-1.52195735713249,-1.32690022270754,-1.23846982832783,-1.17815521207059),
 .UNSPECIFIED.);
#1470=B_SPLINE_CURVE_WITH_KNOTS('',3,(#60884,#60885,#60886,#60887,#60888,
#60889,#60890,#60891,#60892,#60893,#60894,#60895,#60896,#60897,#60898,#60899,
#60900,#60901,#60902,#60903),.UNSPECIFIED.,.F.,.F.,(4,2,2,2,2,2,2,2,2,4),
(-1.17815521207059,-1.15003943394812,-1.00427333986342,-0.858507245778718,
-0.712741151694014,-0.56697505760931,-0.478544663229604,-0.390114268849898,
-0.195057134424949,0.),.UNSPECIFIED.);
#1471=B_SPLINE_CURVE_WITH_KNOTS('',3,(#60913,#60914,#60915,#60916,#60917,
#60918,#60919,#60920,#60921,#60922,#60923,#60924,#60925,#60926),
 .UNSPECIFIED.,.F.,.F.,(4,2,2,2,2,2,4),(-1.71701449155744,-1.52195735713249,
-1.32690022270754,-1.23846982832783,-1.15003943394813,-1.00427333986342,
-0.968278936736989),.UNSPECIFIED.);
#1472=B_SPLINE_CURVE_WITH_KNOTS('',3,(#60928,#60929,#60930,#60931,#60932,
#60933,#60934,#60935,#60936,#60937,#60938,#60939,#60940,#60941,#60942,#60943),
 .UNSPECIFIED.,.F.,.F.,(4,2,2,2,2,2,2,4),(-0.968278936736989,-0.858507245778719,
-0.712741151694015,-0.566975057609311,-0.478544663229605,-0.390114268849899,
-0.19505713442495,0.),.UNSPECIFIED.);
#1473=B_SPLINE_CURVE_WITH_KNOTS('',3,(#60953,#60954,#60955,#60956,#60957,
#60958,#60959,#60960,#60961,#60962,#60963,#60964,#60965,#60966),
 .UNSPECIFIED.,.F.,.F.,(4,2,2,2,2,2,4),(-1.71701449155743,-1.52195735713248,
-1.32690022270754,-1.23846982832783,-1.15003943394812,-1.00427333986342,
-0.858507245778716),.UNSPECIFIED.);
#1474=B_SPLINE_CURVE_WITH_KNOTS('',3,(#60968,#60969,#60970,#60971,#60972,
#60973,#60974,#60975,#60976,#60977,#60978,#60979,#60980,#60981),
 .UNSPECIFIED.,.F.,.F.,(4,2,2,2,2,2,4),(-0.858507245778716,-0.712741151694012,
-0.566975057609308,-0.478544663229602,-0.390114268849896,-0.195057134424948,
0.),.UNSPECIFIED.);
#1475=B_SPLINE_CURVE_WITH_KNOTS('',3,(#60991,#60992,#60993,#60994,#60995,
#60996,#60997,#60998,#60999,#61000,#61001,#61002,#61003,#61004,#61005,#61006),
 .UNSPECIFIED.,.F.,.F.,(4,2,2,2,2,2,2,4),(-1.71701449155744,-1.52195735713249,
-1.32690022270754,-1.23846982832783,-1.15003943394812,-1.00427333986342,
-0.858507245778716,-0.748735554820447),.UNSPECIFIED.);
#1476=B_SPLINE_CURVE_WITH_KNOTS('',3,(#61008,#61009,#61010,#61011,#61012,
#61013,#61014,#61015,#61016,#61017,#61018,#61019,#61020,#61021),
 .UNSPECIFIED.,.F.,.F.,(4,2,2,2,2,2,4),(-0.748735554820447,-0.712741151694013,
-0.56697505760931,-0.478544663229603,-0.390114268849895,-0.195057134424948,
0.),.UNSPECIFIED.);
#1477=B_SPLINE_CURVE_WITH_KNOTS('',3,(#61031,#61032,#61033,#61034,#61035,
#61036,#61037,#61038,#61039,#61040,#61041,#61042,#61043,#61044,#61045,#61046,
#61047,#61048,#61049,#61050),.UNSPECIFIED.,.F.,.F.,(4,2,2,2,2,2,2,2,2,4),
(-1.71701449155743,-1.52195735713249,-1.32690022270754,-1.23846982832783,
-1.15003943394812,-1.00427333986342,-0.858507245778717,-0.712741151694014,
-0.566975057609311,-0.538859279486847),.UNSPECIFIED.);
#1478=B_SPLINE_CURVE_WITH_KNOTS('',3,(#61052,#61053,#61054,#61055,#61056,
#61057,#61058,#61059,#61060,#61061),.UNSPECIFIED.,.F.,.F.,(4,2,2,2,4),(-0.538859279486847,
-0.478544663229605,-0.3901142688499,-0.19505713442495,0.),.UNSPECIFIED.);
#1479=B_SPLINE_CURVE_WITH_KNOTS('',3,(#61072,#61073,#61074,#61075,#61076,
#61077,#61078,#61079,#61080,#61081,#61082,#61083,#61084,#61085,#61086,#61087,
#61088,#61089,#61090,#61091,#61092,#61093,#61094,#61095,#61096,#61097),
 .UNSPECIFIED.,.F.,.F.,(4,2,2,2,2,2,2,2,2,2,2,2,4),(-1.71701449155743,-1.52195735713249,
-1.32690022270754,-1.23846982832783,-1.15003943394813,-1.00427333986342,
-0.858507245778717,-0.712741151694013,-0.56697505760931,-0.478544663229603,
-0.390114268849897,-0.195057134424949,0.),.UNSPECIFIED.);
#1480=B_SPLINE_CURVE_WITH_KNOTS('',3,(#61107,#61108,#61109,#61110,#61111,
#61112,#61113,#61114,#61115,#61116,#61117,#61118,#61119,#61120,#61121,#61122,
#61123,#61124,#61125,#61126,#61127,#61128,#61129,#61130,#61131,#61132),
 .UNSPECIFIED.,.F.,.F.,(4,2,2,2,2,2,2,2,2,2,2,2,4),(-1.71701449155743,-1.52195735713249,
-1.32690022270754,-1.23846982832783,-1.15003943394812,-1.00427333986342,
-0.858507245778718,-0.712741151694014,-0.56697505760931,-0.478544663229604,
-0.390114268849898,-0.195057134424949,0.),.UNSPECIFIED.);
#1481=B_SPLINE_CURVE_WITH_KNOTS('',3,(#61142,#61143,#61144,#61145,#61146,
#61147,#61148,#61149,#61150,#61151,#61152,#61153,#61154,#61155,#61156,#61157,
#61158,#61159,#61160,#61161,#61162,#61163,#61164,#61165,#61166,#61167),
 .UNSPECIFIED.,.F.,.F.,(4,2,2,2,2,2,2,2,2,2,2,2,4),(-1.71701449155744,-1.52195735713249,
-1.32690022270754,-1.23846982832783,-1.15003943394813,-1.00427333986342,
-0.858507245778718,-0.712741151694014,-0.56697505760931,-0.478544663229604,
-0.390114268849898,-0.195057134424949,0.),.UNSPECIFIED.);
#1482=B_SPLINE_CURVE_WITH_KNOTS('',3,(#61177,#61178,#61179,#61180,#61181,
#61182,#61183,#61184,#61185,#61186,#61187,#61188,#61189,#61190,#61191,#61192,
#61193,#61194,#61195,#61196,#61197,#61198,#61199,#61200,#61201,#61202),
 .UNSPECIFIED.,.F.,.F.,(4,2,2,2,2,2,2,2,2,2,2,2,4),(-1.71701449155743,-1.52195735713249,
-1.32690022270754,-1.23846982832783,-1.15003943394812,-1.00427333986342,
-0.858507245778717,-0.712741151694014,-0.56697505760931,-0.478544663229604,
-0.390114268849898,-0.195057134424949,0.),.UNSPECIFIED.);
#1483=B_SPLINE_CURVE_WITH_KNOTS('',3,(#61234,#61235,#61236,#61237,#61238,
#61239,#61240,#61241,#61242,#61243),.UNSPECIFIED.,.F.,.F.,(4,3,3,4),(-4.09254174883833,
-3.98934337020898,-2.99200752765673,-2.06514013327813),.UNSPECIFIED.);
#1484=B_SPLINE_CURVE_WITH_KNOTS('',3,(#61246,#61247,#61248,#61249,#61250,
#61251,#61252),.UNSPECIFIED.,.F.,.F.,(4,3,4),(0.,0.998006970630082,1.11419103802948),
 .UNSPECIFIED.);
#1485=B_SPLINE_CURVE_WITH_KNOTS('',3,(#61257,#61258,#61259,#61260,#61261,
#61262,#61263,#61264,#61265,#61266,#61267,#61268,#61269,#61270,#61271,#61272,
#61273,#61274,#61275,#61276,#61277,#61278),.UNSPECIFIED.,.F.,.F.,(4,3,3,
3,3,3,3,4),(-10.3757270560179,-9.97335842552244,-8.9760225829702,-7.97868674041795,
-6.9813508978657,-5.98401505531347,-4.98667921276122,-4.09254174883833),
 .UNSPECIFIED.);
#1486=B_SPLINE_CURVE_WITH_KNOTS('',3,(#61279,#61280,#61281,#61282,#61283,
#61284,#61285,#61286,#61287,#61288,#61289,#61290,#61291,#61292,#61293,#61294,
#61295,#61296,#61297,#61298,#61299,#61300),.UNSPECIFIED.,.F.,.F.,(4,3,3,
3,3,3,3,4),(1.11419103802948,1.99601394126018,2.99402091189026,3.99202788252035,
4.99003485315045,5.98804182378054,6.98604879441062,7.39737634520907),
 .UNSPECIFIED.);
#1487=B_SPLINE_CURVE_WITH_KNOTS('',3,(#61305,#61306,#61307,#61308,#61309,
#61310,#61311,#61312,#61313,#61314,#61315,#61316,#61317,#61318,#61319,#61320,
#61321,#61322,#61323,#61324,#61325,#61326),.UNSPECIFIED.,.F.,.F.,(4,3,3,
3,3,3,3,4),(-16.6589123631975,-15.9573734808359,-14.9600376382837,-13.9627017957314,
-12.9653659531792,-11.9680301106269,-10.9706942680747,-10.3757270560179),
 .UNSPECIFIED.);
#1488=B_SPLINE_CURVE_WITH_KNOTS('',3,(#61327,#61328,#61329,#61330,#61331,
#61332,#61333,#61334,#61335,#61336,#61337,#61338,#61339,#61340,#61341,#61342,
#61343,#61344,#61345,#61346,#61347,#61348),.UNSPECIFIED.,.F.,.F.,(4,3,3,
3,3,3,3,4),(7.39737634520907,7.98405576504071,8.9820627356708,9.98006970630089,
10.978076676931,11.9760836475611,12.9740906181912,13.6805616523887),
 .UNSPECIFIED.);
#1489=B_SPLINE_CURVE_WITH_KNOTS('',3,(#61353,#61354,#61355,#61356,#61357,
#61358,#61359,#61360,#61361,#61362,#61363,#61364,#61365,#61366,#61367,#61368,
#61369,#61370,#61371,#61372,#61373,#61374,#61375,#61376,#61377),
 .UNSPECIFIED.,.F.,.F.,(4,3,3,3,3,3,3,3,4),(-22.9420976703771,-22.9387243787016,
-21.9413885361494,-20.9440526935971,-19.9467168510449,-18.9493810084926,
-17.9520451659404,-16.9547093233881,-16.6589123631975),.UNSPECIFIED.);
#1490=B_SPLINE_CURVE_WITH_KNOTS('',3,(#61378,#61379,#61380,#61381,#61382,
#61383,#61384,#61385,#61386,#61387,#61388,#61389,#61390,#61391,#61392,#61393,
#61394,#61395,#61396,#61397,#61398,#61399,#61400,#61401,#61402),
 .UNSPECIFIED.,.F.,.F.,(4,3,3,3,3,3,3,3,4),(13.6805616523887,13.9720975888212,
14.9701045594513,15.9681115300814,16.9661185007115,17.9641254713416,18.9621324419717,
19.9601394126018,19.9637469595682),.UNSPECIFIED.);
#1491=B_SPLINE_CURVE_WITH_KNOTS('',3,(#61407,#61408,#61409,#61410,#61411,
#61412,#61413,#61414,#61415,#61416,#61417,#61418,#61419,#61420,#61421,#61422,
#61423,#61424,#61425,#61426,#61427,#61428),.UNSPECIFIED.,.F.,.F.,(4,3,3,
3,3,3,3,4),(-29.2252829775567,-28.9227394340151,-27.9254035914628,-26.9280677489106,
-25.9307319063583,-24.9333960638061,-23.9360602212539,-22.9420976703771),
 .UNSPECIFIED.);
#1492=B_SPLINE_CURVE_WITH_KNOTS('',3,(#61429,#61430,#61431,#61432,#61433,
#61434,#61435,#61436,#61437,#61438,#61439,#61440,#61441,#61442,#61443,#61444,
#61445,#61446,#61447,#61448,#61449,#61450),.UNSPECIFIED.,.F.,.F.,(4,3,3,
3,3,3,3,4),(19.9637469595682,20.9581463832319,21.956153353862,22.954160324492,
23.9521672951221,24.9501742657522,25.9481812363823,26.2469322667478),
 .UNSPECIFIED.);
#1493=B_SPLINE_CURVE_WITH_KNOTS('',3,(#61455,#61456,#61457,#61458,#61459,
#61460,#61461,#61462,#61463,#61464,#61465,#61466,#61467,#61468,#61469,#61470,
#61471,#61472,#61473,#61474,#61475,#61476),.UNSPECIFIED.,.F.,.F.,(4,3,3,
3,3,3,3,4),(-35.5084682847363,-34.9067544893285,-33.9094186467763,-32.9120828042241,
-31.9147469616718,-30.9174111191196,-29.9200752765673,-29.2252829775567),
 .UNSPECIFIED.);
#1494=B_SPLINE_CURVE_WITH_KNOTS('',3,(#61477,#61478,#61479,#61480,#61481,
#61482,#61483,#61484,#61485,#61486,#61487,#61488,#61489,#61490,#61491,#61492,
#61493,#61494,#61495,#61496,#61497,#61498),.UNSPECIFIED.,.F.,.F.,(4,3,3,
3,3,3,3,4),(26.2469322667478,26.9461882070124,27.9441951776425,28.9422021482726,
29.9402091189027,30.9382160895327,31.9362230601628,32.5301175739274),
 .UNSPECIFIED.);
#1495=B_SPLINE_CURVE_WITH_KNOTS('',3,(#61503,#61504,#61505,#61506,#61507,
#61508,#61509,#61510,#61511,#61512,#61513,#61514,#61515,#61516,#61517,#61518,
#61519,#61520,#61521,#61522,#61523,#61524),.UNSPECIFIED.,.F.,.F.,(4,3,3,
3,3,3,3,4),(-41.7916535919159,-40.890769544642,-39.8934337020898,-38.8960978595375,
-37.8987620169853,-36.901426174433,-35.9040903318808,-35.5084682847363),
 .UNSPECIFIED.);
#1496=B_SPLINE_CURVE_WITH_KNOTS('',3,(#61525,#61526,#61527,#61528,#61529,
#61530,#61531,#61532,#61533,#61534,#61535,#61536,#61537,#61538,#61539,#61540,
#61541,#61542,#61543,#61544,#61545,#61546),.UNSPECIFIED.,.F.,.F.,(4,3,3,
3,3,3,3,4),(32.5301175739274,32.9342300307929,33.932237001423,34.9302439720531,
35.9282509426832,36.9262579133133,37.9242648839434,38.813302881107),
 .UNSPECIFIED.);
#1497=B_SPLINE_CURVE_WITH_KNOTS('',3,(#61551,#61552,#61553,#61554,#61555,
#61556,#61557,#61558,#61559,#61560,#61561,#61562,#61563,#61564,#61565,#61566,
#61567,#61568,#61569,#61570,#61571,#61572,#61573,#61574,#61575),
 .UNSPECIFIED.,.F.,.F.,(4,3,3,3,3,3,3,3,4),(-48.0748388990955,-47.8721204425077,
-46.8747845999555,-45.8774487574032,-44.880112914851,-43.8827770722987,
-42.8854412297465,-41.8881053871943,-41.7916535919159),.UNSPECIFIED.);
#1498=B_SPLINE_CURVE_WITH_KNOTS('',3,(#61576,#61577,#61578,#61579,#61580,
#61581,#61582,#61583,#61584,#61585,#61586,#61587,#61588,#61589,#61590,#61591,
#61592,#61593,#61594,#61595,#61596,#61597,#61598,#61599,#61600),
 .UNSPECIFIED.,.F.,.F.,(4,3,3,3,3,3,3,3,4),(38.813302881107,38.9222718545735,
39.9202788252036,40.9182857958337,41.9162927664637,42.9142997370938,43.9123067077239,
44.910313678354,45.0964881882866),.UNSPECIFIED.);
#1499=B_SPLINE_CURVE_WITH_KNOTS('',3,(#61605,#61606,#61607,#61608,#61609,
#61610,#61611,#61612,#61613,#61614,#61615,#61616,#61617,#61618,#61619,#61620,
#61621,#61622,#61623,#61624,#61625,#61626),.UNSPECIFIED.,.F.,.F.,(4,3,3,
3,3,3,3,4),(-54.3580242062751,-53.8561354978212,-52.8587996552689,-51.8614638127167,
-50.8641279701645,-49.8667921276122,-48.86945628506,-48.0748388990955),
 .UNSPECIFIED.);
#1500=B_SPLINE_CURVE_WITH_KNOTS('',3,(#61627,#61628,#61629,#61630,#61631,
#61632,#61633,#61634,#61635,#61636,#61637,#61638,#61639,#61640,#61641,#61642,
#61643,#61644,#61645,#61646,#61647,#61648),.UNSPECIFIED.,.F.,.F.,(4,3,3,
3,3,3,3,4),(45.0964881882866,45.9083206489841,46.9063276196142,47.9043345902443,
48.9023415608744,49.9003485315045,50.8983555021345,51.3796734954662),
 .UNSPECIFIED.);
#1501=B_SPLINE_CURVE_WITH_KNOTS('',3,(#61653,#61654,#61655,#61656,#61657,
#61658,#61659,#61660,#61661,#61662,#61663,#61664,#61665,#61666,#61667,#61668,
#61669,#61670,#61671,#61672,#61673,#61674),.UNSPECIFIED.,.F.,.F.,(4,3,3,
3,3,3,3,4),(-60.6412095134546,-59.8401505531347,-58.8428147105824,-57.8454788680302,
-56.8481430254779,-55.8508071829257,-54.8534713403734,-54.3580242062751),
 .UNSPECIFIED.);
#1502=B_SPLINE_CURVE_WITH_KNOTS('',3,(#61675,#61676,#61677,#61678,#61679,
#61680,#61681,#61682,#61683,#61684,#61685,#61686,#61687,#61688,#61689,#61690,
#61691,#61692,#61693,#61694,#61695,#61696),.UNSPECIFIED.,.F.,.F.,(4,3,3,
3,3,3,3,4),(51.3796734954662,51.8963624727646,52.8943694433947,53.8923764140248,
54.8903833846549,55.888390355285,56.8863973259151,57.6628588026458),
 .UNSPECIFIED.);
#1503=B_SPLINE_CURVE_WITH_KNOTS('',3,(#61701,#61702,#61703,#61704,#61705,
#61706,#61707,#61708,#61709,#61710,#61711,#61712,#61713,#61714,#61715,#61716,
#61717,#61718,#61719,#61720,#61721,#61722,#61723,#61724,#61725),
 .UNSPECIFIED.,.F.,.F.,(4,3,3,3,3,3,3,3,4),(-66.9243948206342,-66.8215014510004,
-65.8241656084481,-64.8268297658959,-63.8294939233436,-62.8321580807914,
-61.8348222382391,-60.8374863956869,-60.6412095134546),.UNSPECIFIED.);
#1504=B_SPLINE_CURVE_WITH_KNOTS('',3,(#61726,#61727,#61728,#61729,#61730,
#61731,#61732,#61733,#61734,#61735,#61736,#61737,#61738,#61739,#61740,#61741,
#61742,#61743,#61744,#61745,#61746,#61747,#61748,#61749,#61750),
 .UNSPECIFIED.,.F.,.F.,(4,3,3,3,3,3,3,3,4),(57.6628588026458,57.8844042965452,
58.8824112671752,59.8804182378054,60.8784252084354,61.8764321790655,62.8744391496956,
63.8724461203257,63.9460441098254),.UNSPECIFIED.);
#1505=B_SPLINE_CURVE_WITH_KNOTS('',3,(#61755,#61756,#61757,#61758,#61759,
#61760,#61761,#61762,#61763,#61764,#61765,#61766,#61767,#61768,#61769,#61770,
#61771,#61772,#61773,#61774,#61775,#61776),.UNSPECIFIED.,.F.,.F.,(4,3,3,
3,3,3,3,4),(-73.2075801278138,-72.8055165063138,-71.8081806637616,-70.8108448212093,
-69.8135089786571,-68.8161731361048,-67.8188372935526,-66.9243948206342),
 .UNSPECIFIED.);
#1506=B_SPLINE_CURVE_WITH_KNOTS('',3,(#61777,#61778,#61779,#61780,#61781,
#61782,#61783,#61784,#61785,#61786,#61787,#61788,#61789,#61790,#61791,#61792,
#61793,#61794,#61795,#61796,#61797,#61798),.UNSPECIFIED.,.F.,.F.,(4,3,3,
3,3,3,3,4),(63.9460441098254,64.8704530909558,65.8684600615859,66.866467032216,
67.8644740028461,68.8624809734761,69.8604879441062,70.229229417005),
 .UNSPECIFIED.);
#1507=B_SPLINE_CURVE_WITH_KNOTS('',3,(#61803,#61804,#61805,#61806,#61807,
#61808,#61809,#61810,#61811,#61812,#61813,#61814,#61815,#61816,#61817,#61818,
#61819,#61820,#61821,#61822,#61823,#61824),.UNSPECIFIED.,.F.,.F.,(4,3,3,
3,3,3,3,4),(-79.4907654349934,-78.7895315616273,-77.792195719075,-76.7948598765228,
-75.7975240339705,-74.8001881914183,-73.802852348866,-73.2075801278138),
 .UNSPECIFIED.);
#1508=B_SPLINE_CURVE_WITH_KNOTS('',3,(#61825,#61826,#61827,#61828,#61829,
#61830,#61831,#61832,#61833,#61834,#61835,#61836,#61837,#61838,#61839,#61840,
#61841,#61842,#61843,#61844,#61845,#61846),.UNSPECIFIED.,.F.,.F.,(4,3,3,
3,3,3,3,4),(70.229229417005,70.8584949147363,71.8565018853664,72.8545088559965,
73.8525158266266,74.8505227972567,75.8485297678868,76.5124147241846),
 .UNSPECIFIED.);
#1509=B_SPLINE_CURVE_WITH_KNOTS('',3,(#61851,#61852,#61853,#61854,#61855,
#61856,#61857,#61858,#61859,#61860,#61861,#61862,#61863,#61864,#61865,#61866,
#61867,#61868,#61869,#61870,#61871,#61872,#61873,#61874,#61875),
 .UNSPECIFIED.,.F.,.F.,(4,3,3,3,3,3,3,3,4),(-85.773950742173,-85.770882459493,
-84.7735466169407,-83.7762107743885,-82.7788749318363,-81.781539089284,
-80.7842032467318,-79.7868674041795,-79.4907654349934),.UNSPECIFIED.);
#1510=B_SPLINE_CURVE_WITH_KNOTS('',3,(#61876,#61877,#61878,#61879,#61880,
#61881,#61882,#61883,#61884,#61885,#61886,#61887,#61888,#61889,#61890,#61891,
#61892,#61893,#61894,#61895,#61896,#61897),.UNSPECIFIED.,.F.,.F.,(4,3,3,
3,3,3,3,4),(76.5124147241846,76.8465367385169,77.8445437091469,78.842550679777,
79.8405576504071,80.8385646210372,81.8365715916673,82.7956000313642),
 .UNSPECIFIED.);
#1511=B_SPLINE_CURVE_WITH_KNOTS('',3,(#61902,#61903,#61904,#61905,#61906,
#61907,#61908,#61909,#61910,#61911,#61912,#61913,#61914,#61915,#61916,#61917,
#61918,#61919,#61920,#61921,#61922,#61923),.UNSPECIFIED.,.F.,.F.,(4,3,3,
3,3,3,3,4),(-92.0571360493526,-91.7548975148065,-90.7575616722542,-89.760225829702,
-88.7628899871497,-87.7655541445975,-86.7682183020452,-85.773950742173),
 .UNSPECIFIED.);
#1512=B_SPLINE_CURVE_WITH_KNOTS('',3,(#61924,#61925,#61926,#61927,#61928,
#61929,#61930,#61931,#61932,#61933,#61934,#61935,#61936,#61937,#61938,#61939,
#61940,#61941,#61942,#61943,#61944,#61945,#61946,#61947,#61948),
 .UNSPECIFIED.,.F.,.F.,(4,3,3,3,3,3,3,3,4),(82.7956000313642,82.8345785622974,
83.8325855329275,84.8305925035576,85.8285994741877,86.8266064448178,87.8246134154479,
88.822620386078,89.0787853385438),.UNSPECIFIED.);
#1513=B_SPLINE_CURVE_WITH_KNOTS('',3,(#61953,#61954,#61955,#61956,#61957,
#61958,#61959,#61960,#61961,#61962,#61963,#61964,#61965,#61966,#61967,#61968,
#61969,#61970,#61971,#61972,#61973,#61974),.UNSPECIFIED.,.F.,.F.,(4,3,3,
3,3,3,3,4),(-98.3403213565322,-97.7389125701199,-96.7415767275677,-95.7442408850154,
-94.7469050424632,-93.7495691999109,-92.7522333573587,-92.0571360493526),
 .UNSPECIFIED.);
#1514=B_SPLINE_CURVE_WITH_KNOTS('',3,(#61975,#61976,#61977,#61978,#61979,
#61980,#61981,#61982,#61983,#61984,#61985,#61986,#61987,#61988,#61989,#61990,
#61991,#61992,#61993,#61994,#61995,#61996),.UNSPECIFIED.,.F.,.F.,(4,3,3,
3,3,3,3,4),(89.0787853385438,89.820627356708,90.8186343273381,91.8166412979682,
92.8146482685983,93.8126552392284,94.8106622098585,95.3619706457233),
 .UNSPECIFIED.);
#1515=B_SPLINE_CURVE_WITH_KNOTS('',3,(#62002,#62003,#62004,#62005,#62006,
#62007,#62008,#62009),.UNSPECIFIED.,.F.,.F.,(4,1,1,1,1,4),(109.955742875643,
110.351669931783,111.349005774335,112.346341616887,113.343677459439,114.341013301992),
 .UNSPECIFIED.);
#1516=B_SPLINE_CURVE_WITH_KNOTS('',3,(#62012,#62013,#62014,#62015,#62016,
#62017,#62018),.UNSPECIFIED.,.F.,.F.,(4,1,1,1,4),(109.955742875643,110.107297927009,
111.105304897639,112.103311868269,113.101318838899),.UNSPECIFIED.);
#1517=B_SPLINE_CURVE_WITH_KNOTS('',3,(#62023,#62024,#62025,#62026,#62027,
#62028,#62029,#62030,#62031,#62032),.UNSPECIFIED.,.F.,.F.,(4,1,1,1,1,1,
1,4),(103.672557568463,104.367654876469,105.364990719021,106.362326561574,
107.359662404126,108.356998246678,109.35433408923,109.955742875643),
 .UNSPECIFIED.);
#1518=B_SPLINE_CURVE_WITH_KNOTS('',3,(#62033,#62034,#62035,#62036,#62037,
#62038,#62039,#62040,#62041,#62042),.UNSPECIFIED.,.F.,.F.,(4,1,1,1,1,1,
1,4),(103.672557568463,104.119256103228,105.117263073858,106.115270044488,
107.113277015118,108.111283985749,109.109290956379,109.955742875643),
 .UNSPECIFIED.);
#1519=B_SPLINE_CURVE_WITH_KNOTS('',3,(#62047,#62048,#62049,#62050,#62051,
#62052,#62053,#62054,#62055,#62056),.UNSPECIFIED.,.F.,.F.,(4,1,1,1,1,1,
1,4),(97.3893722612836,98.3836398211558,99.380975663708,100.37831150626,
101.375647348812,102.372983191365,103.370319033917,103.672557568463),
 .UNSPECIFIED.);
#1520=B_SPLINE_CURVE_WITH_KNOTS('',3,(#62057,#62058,#62059,#62060,#62061,
#62062,#62063,#62064,#62065,#62066),.UNSPECIFIED.,.F.,.F.,(4,1,1,1,1,1,
1,4),(97.3893722612836,98.1312142794477,99.1292212500778,100.127228220708,
101.125235191338,102.123242161968,103.121249132598,103.672557568463),
 .UNSPECIFIED.);
#1521=B_SPLINE_CURVE_WITH_KNOTS('',3,(#62071,#62072,#62073,#62074,#62075,
#62076,#62077,#62078,#62079,#62080,#62081),.UNSPECIFIED.,.F.,.F.,(4,1,1,
1,1,1,1,1,4),(91.106186954104,91.4022889232901,92.3996247658423,93.3969606083945,
94.3942964509468,95.391632293499,96.3889681360513,97.3863039786035,97.3893722612836),
 .UNSPECIFIED.);
#1522=B_SPLINE_CURVE_WITH_KNOTS('',3,(#62082,#62083,#62084,#62085,#62086,
#62087,#62088,#62089,#62090,#62091,#62092),.UNSPECIFIED.,.F.,.F.,(4,1,1,
1,1,1,1,1,4),(91.106186954104,91.1451654850371,92.1431724556672,93.1411794262973,
94.1391863969273,95.1371933675574,96.1352003381875,97.1332073088176,97.3893722612836),
 .UNSPECIFIED.);
#1523=B_SPLINE_CURVE_WITH_KNOTS('',3,(#62097,#62098,#62099,#62100,#62101,
#62102,#62103,#62104,#62105,#62106),.UNSPECIFIED.,.F.,.F.,(4,1,1,1,1,1,
1,4),(84.8230016469244,85.4182738679766,86.4156097105288,87.4129455530811,
88.4102813956333,89.4076172381856,90.4049530807378,91.106186954104),
 .UNSPECIFIED.);
#1524=B_SPLINE_CURVE_WITH_KNOTS('',3,(#62107,#62108,#62109,#62110,#62111,
#62112,#62113,#62114,#62115,#62116),.UNSPECIFIED.,.F.,.F.,(4,1,1,1,1,1,
1,4),(84.8230016469244,85.1571236612565,86.1551306318866,87.1531376025167,
88.1511445731468,89.1491515437769,90.147158514407,91.106186954104),
 .UNSPECIFIED.);
#1525=B_SPLINE_CURVE_WITH_KNOTS('',3,(#62121,#62122,#62123,#62124,#62125,
#62126,#62127,#62128,#62129,#62130),.UNSPECIFIED.,.F.,.F.,(4,1,1,1,1,1,
1,4),(78.5398163397448,79.4342588126631,80.4315946552154,81.4289304977676,
82.4262663403199,83.4236021828721,84.4209380254243,84.8230016469244),
 .UNSPECIFIED.);
#1526=B_SPLINE_CURVE_WITH_KNOTS('',3,(#62131,#62132,#62133,#62134,#62135,
#62136,#62137,#62138,#62139,#62140),.UNSPECIFIED.,.F.,.F.,(4,1,1,1,1,1,
1,4),(78.5398163397448,79.169081837476,80.1670888081061,81.1650957787362,
82.1631027493663,83.1611097199964,84.1591166906264,84.8230016469244),
 .UNSPECIFIED.);
#1527=B_SPLINE_CURVE_WITH_KNOTS('',3,(#62145,#62146,#62147,#62148,#62149,
#62150,#62151,#62152,#62153,#62154,#62155),.UNSPECIFIED.,.F.,.F.,(4,1,1,
1,1,1,1,1,4),(72.2566310325652,72.4529079147974,73.4502437573497,74.4475795999019,
75.4449154424541,76.4422512850064,77.4395871275586,78.4369229701109,78.5398163397448),
 .UNSPECIFIED.);
#1528=B_SPLINE_CURVE_WITH_KNOTS('',3,(#62156,#62157,#62158,#62159,#62160,
#62161,#62162,#62163,#62164,#62165),.UNSPECIFIED.,.F.,.F.,(4,1,1,1,1,1,
1,4),(72.2566310325652,73.1810400136955,74.1790469843256,75.1770539549557,
76.1750609255857,77.1730678962158,78.1710748668459,78.5398163397448),
 .UNSPECIFIED.);
#1529=B_SPLINE_CURVE_WITH_KNOTS('',3,(#62170,#62171,#62172,#62173,#62174,
#62175,#62176,#62177,#62178,#62179),.UNSPECIFIED.,.F.,.F.,(4,1,1,1,1,1,
1,4),(65.9734457253856,66.468892859484,67.4662287020362,68.4635645445884,
69.4609003871407,70.4582362296929,71.4555720722452,72.2566310325652),
 .UNSPECIFIED.);
#1530=B_SPLINE_CURVE_WITH_KNOTS('',3,(#62180,#62181,#62182,#62183,#62184,
#62185,#62186,#62187,#62188,#62189,#62190),.UNSPECIFIED.,.F.,.F.,(4,1,1,
1,1,1,1,1,4),(65.9734457253856,66.1949912192848,67.1929981899149,68.191005160545,
69.1890121311751,70.1870191018052,71.1850260724353,72.1830330430654,72.2566310325652),
 .UNSPECIFIED.);
#1531=B_SPLINE_CURVE_WITH_KNOTS('',3,(#62195,#62196,#62197,#62198,#62199,
#62200,#62201,#62202,#62203,#62204),.UNSPECIFIED.,.F.,.F.,(4,1,1,1,1,1,
1,4),(59.690260418206,60.4848778041705,61.4822136467227,62.479549489275,
63.4768853318272,64.4742211743795,65.4715570169317,65.9734457253856),
 .UNSPECIFIED.);
#1532=B_SPLINE_CURVE_WITH_KNOTS('',3,(#62205,#62206,#62207,#62208,#62209,
#62210,#62211,#62212,#62213,#62214),.UNSPECIFIED.,.F.,.F.,(4,1,1,1,1,1,
1,4),(59.690260418206,60.2069493955043,61.2049563661344,62.2029633367645,
63.2009703073946,64.1989772780247,65.1969842486548,65.9734457253856),
 .UNSPECIFIED.);
#1533=B_SPLINE_CURVE_WITH_KNOTS('',3,(#62219,#62220,#62221,#62222,#62223,
#62224,#62225,#62226,#62227,#62228,#62229),.UNSPECIFIED.,.F.,.F.,(4,1,1,
1,1,1,1,1,4),(53.4070751110265,53.5035269063048,54.500862748857,55.4981985914093,
56.4955344339615,57.4928702765138,58.490206119066,59.4875419616182,59.690260418206),
 .UNSPECIFIED.);
#1534=B_SPLINE_CURVE_WITH_KNOTS('',3,(#62230,#62231,#62232,#62233,#62234,
#62235,#62236,#62237,#62238,#62239),.UNSPECIFIED.,.F.,.F.,(4,1,1,1,1,1,
1,4),(53.4070751110264,54.2189075717238,55.2169145423539,56.214921512984,
57.212928483614,58.2109354542441,59.2089424248742,59.690260418206),
 .UNSPECIFIED.);
#1535=B_SPLINE_CURVE_WITH_KNOTS('',3,(#62244,#62245,#62246,#62247,#62248,
#62249,#62250,#62251,#62252,#62253),.UNSPECIFIED.,.F.,.F.,(4,1,1,1,1,1,
1,4),(47.1238898038469,47.5195118509913,48.5168476935436,49.5141835360958,
50.5115193786481,51.5088552212003,52.5061910637525,53.4070751110265),
 .UNSPECIFIED.);
#1536=B_SPLINE_CURVE_WITH_KNOTS('',3,(#62254,#62255,#62256,#62257,#62258,
#62259,#62260,#62261,#62262,#62263,#62264),.UNSPECIFIED.,.F.,.F.,(4,1,1,
1,1,1,1,1,4),(47.1238898038468,47.2328587773132,48.2308657479432,49.2288727185733,
50.2268796892034,51.2248866598335,52.2228936304636,53.2209006010937,53.4070751110264),
 .UNSPECIFIED.);
#1537=B_SPLINE_CURVE_WITH_KNOTS('',3,(#62269,#62270,#62271,#62272,#62273,
#62274,#62275,#62276,#62277,#62278),.UNSPECIFIED.,.F.,.F.,(4,1,1,1,1,1,
1,4),(40.8407044966673,41.5354967956779,42.5328326382301,43.5301684807823,
44.5275043233346,45.5248401658868,46.5221760084391,47.1238898038469),
 .UNSPECIFIED.);
#1538=B_SPLINE_CURVE_WITH_KNOTS('',3,(#62279,#62280,#62281,#62282,#62283,
#62284,#62285,#62286,#62287,#62288),.UNSPECIFIED.,.F.,.F.,(4,1,1,1,1,1,
1,4),(40.8407044966672,41.2448169535326,42.2428239241627,43.2408308947928,
44.2388378654229,45.236844836053,46.2348518066831,47.1238898038468),
 .UNSPECIFIED.);
#1539=B_SPLINE_CURVE_WITH_KNOTS('',3,(#62293,#62294,#62295,#62296,#62297,
#62298,#62299,#62300,#62301,#62302),.UNSPECIFIED.,.F.,.F.,(4,1,1,1,1,1,
1,4),(34.5575191894877,35.5514817403644,36.5488175829166,37.5461534254689,
38.5434892680211,39.5408251105734,40.5381609531256,40.8407044966673),
 .UNSPECIFIED.);
#1540=B_SPLINE_CURVE_WITH_KNOTS('',3,(#62303,#62304,#62305,#62306,#62307,
#62308,#62309,#62310,#62311,#62312),.UNSPECIFIED.,.F.,.F.,(4,1,1,1,1,1,
1,4),(34.5575191894876,35.2567751297521,36.2547821003822,37.2527890710123,
38.2507960416424,39.2488030122724,40.2468099829025,40.8407044966672),
 .UNSPECIFIED.);
#1541=B_SPLINE_CURVE_WITH_KNOTS('',3,(#62317,#62318,#62319,#62320,#62321,
#62322,#62323,#62324,#62325,#62326,#62327),.UNSPECIFIED.,.F.,.F.,(4,1,1,
1,1,1,1,1,4),(28.2743338823081,28.5701308424987,29.5674666850509,30.5648025276032,
31.5621383701554,32.5594742127077,33.5568100552599,34.5541458978121,34.5575191894877),
 .UNSPECIFIED.);
#1542=B_SPLINE_CURVE_WITH_KNOTS('',3,(#62328,#62329,#62330,#62331,#62332,
#62333,#62334,#62335,#62336,#62337),.UNSPECIFIED.,.F.,.F.,(4,1,1,1,1,1,
1,4),(28.274333882308,29.2687333059716,30.2667402766016,31.2647472472317,
32.2627542178618,33.2607611884919,34.258768159122,34.5575191894876),
 .UNSPECIFIED.);
#1543=B_SPLINE_CURVE_WITH_KNOTS('',3,(#62342,#62343,#62344,#62345,#62346,
#62347,#62348,#62349,#62350,#62351),.UNSPECIFIED.,.F.,.F.,(4,1,1,1,1,1,
1,4),(21.9911485751285,22.5861157871852,23.5834516297375,24.5807874722897,
25.5781233148419,26.5754591573942,27.5727949999464,28.2743338823081),
 .UNSPECIFIED.);
#1544=B_SPLINE_CURVE_WITH_KNOTS('',3,(#62352,#62353,#62354,#62355,#62356,
#62357,#62358,#62359,#62360,#62361,#62362),.UNSPECIFIED.,.F.,.F.,(4,1,1,
1,1,1,1,1,4),(21.9911485751285,22.2826845115609,23.280691482191,24.2786984528211,
25.2767054234512,26.2747123940813,27.2727193647114,28.2707263353415,28.274333882308),
 .UNSPECIFIED.);
#1545=B_SPLINE_CURVE_WITH_KNOTS('',3,(#62367,#62368,#62369,#62370,#62371,
#62372,#62373,#62374,#62375,#62376),.UNSPECIFIED.,.F.,.F.,(4,1,1,1,1,1,
1,4),(15.7079632679489,16.6021007318718,17.599436574424,18.5967724169762,
19.5941082595285,20.5914441020807,21.588779944633,21.9911485751285),
 .UNSPECIFIED.);
#1546=B_SPLINE_CURVE_WITH_KNOTS('',3,(#62377,#62378,#62379,#62380,#62381,
#62382,#62383,#62384,#62385,#62386),.UNSPECIFIED.,.F.,.F.,(4,1,1,1,1,1,
1,4),(15.7079632679489,16.2946426877804,17.2926496584105,18.2906566290406,
19.2886635996707,20.2866705703008,21.2846775409308,21.9911485751285),
 .UNSPECIFIED.);
#1547=B_SPLINE_CURVE_WITH_KNOTS('',3,(#62389,#62390,#62391,#62392,#62393,
#62394,#62395,#62396,#62397,#62398,#62399,#62400,#62401,#62402,#62403,#62404,
#62405,#62406,#62407,#62408,#62409,#62410,#62411,#62412,#62413,#62414,#62415,
#62416,#62417,#62418,#62419,#62420,#62421,#62422,#62423,#62424,#62425,#62426,
#62427,#62428,#62429,#62430,#62431,#62432,#62433,#62434,#62435,#62436,#62437,
#62438,#62439,#62440,#62441,#62442,#62443,#62444,#62445,#62446,#62447,#62448,
#62449,#62450,#62451,#62452,#62453,#62454,#62455,#62456,#62457,#62458,#62459,
#62460,#62461,#62462,#62463,#62464,#62465,#62466,#62467,#62468,#62469,#62470,
#62471,#62472,#62473,#62474,#62475,#62476,#62477,#62478,#62479,#62480,#62481,
#62482,#62483,#62484,#62485,#62486,#62487,#62488,#62489,#62490,#62491,#62492,
#62493,#62494,#62495,#62496,#62497,#62498,#62499,#62500,#62501,#62502,#62503,
#62504,#62505,#62506,#62507,#62508,#62509,#62510,#62511,#62512,#62513,#62514,
#62515),.UNSPECIFIED.,.F.,.F.,(4,3,3,3,3,3,3,3,3,3,3,3,3,3,3,3,3,3,3,3,
3,3,3,3,3,3,3,3,3,3,3,3,3,3,3,3,3,3,3,3,3,3,4),(-0.996917990983956,-0.978871588953361,
-0.96111138213616,-0.951572166884024,-0.94788730271085,-0.928958746515757,
-0.909876465942473,-0.904936500084987,-0.901848009849201,-0.882541837721487,
-0.863353532865677,-0.850071733640713,-0.842096384739765,-0.838733342910066,
-0.836789934415749,-0.818254783653573,-0.798902591036692,-0.782735584954257,
-0.778204258927876,-0.774298497031817,-0.75473106557298,-0.734923369072796,
-0.7185841623989,-0.712646708603056,-0.709110058221935,-0.689189804001172,
-0.669566542377212,-0.649891129487148,-0.644972000047888,-0.641670824784499,
-0.621885476350888,-0.601705353300825,-0.588427767916722,-0.579820295317846,
-0.575107459303169,-0.554609906499435,-0.53420632583291,-0.514845498030454,
-0.510394870356688,-0.506773348856668,-0.495484670227998,-0.475532816008266,
-0.468408511919796),.UNSPECIFIED.);
#1548=B_SPLINE_CURVE_WITH_KNOTS('',3,(#62517,#62518,#62519,#62520,#62521,
#62522,#62523,#62524,#62525,#62526,#62527,#62528,#62529,#62530,#62531,#62532,
#62533,#62534,#62535,#62536,#62537,#62538,#62539,#62540,#62541,#62542,#62543,
#62544,#62545,#62546,#62547,#62548,#62549,#62550,#62551,#62552,#62553,#62554,
#62555,#62556,#62557,#62558,#62559,#62560,#62561,#62562,#62563,#62564,#62565,
#62566,#62567,#62568,#62569,#62570,#62571,#62572,#62573,#62574),
 .UNSPECIFIED.,.F.,.F.,(4,3,3,3,3,3,3,3,3,3,3,3,3,3,3,3,3,3,3,4),(-0.271362855059921,
-0.249815156703991,-0.228817954605844,-0.214757059032555,-0.202695986178297,
-0.199258382274391,-0.179079040584676,-0.172574372312687,-0.151002575773601,
-0.132127253801901,-0.128545223737615,-0.108660382312346,-0.0889046320299183,
-0.0695673553379917,-0.0643976613730527,-0.0611873083345303,-0.0424332578302701,
-0.0240014673407122,-0.00610701619818059,0.),.UNSPECIFIED.);
#1549=B_SPLINE_CURVE_WITH_KNOTS('',3,(#62577,#62578,#62579,#62580,#62581,
#62582,#62583,#62584,#62585,#62586,#62587,#62588,#62589,#62590,#62591,#62592,
#62593,#62594,#62595,#62596,#62597,#62598,#62599,#62600,#62601,#62602,#62603,
#62604,#62605,#62606,#62607,#62608,#62609,#62610,#62611,#62612,#62613,#62614,
#62615,#62616,#62617,#62618,#62619,#62620,#62621,#62622,#62623,#62624,#62625,
#62626,#62627,#62628,#62629,#62630,#62631,#62632,#62633,#62634,#62635,#62636,
#62637,#62638,#62639,#62640,#62641,#62642,#62643,#62644,#62645,#62646,#62647,
#62648,#62649,#62650,#62651,#62652,#62653,#62654,#62655,#62656,#62657,#62658,
#62659,#62660,#62661,#62662,#62663,#62664,#62665,#62666,#62667,#62668,#62669,
#62670,#62671,#62672,#62673,#62674,#62675,#62676,#62677,#62678,#62679),
 .UNSPECIFIED.,.F.,.F.,(4,3,3,3,3,3,3,3,3,3,3,3,3,3,3,3,3,3,3,3,3,3,3,3,
3,3,3,3,3,3,3,3,3,3,4),(-0.468408511919796,-0.449159592277506,-0.442679572366002,
-0.439139523917826,-0.418501747794262,-0.397540534942074,-0.376759689901926,
-0.369408338867191,-0.366188435771172,-0.344993296658329,-0.324164935680159,
-0.314417154781481,-0.302674036643168,-0.298303152413865,-0.294792657786698,
-0.273759483634418,-0.252453791079512,-0.23671297526563,-0.228622459040654,
-0.22484613779528,-0.221071692886511,-0.199520974492535,-0.177947952659577,
-0.156760757052952,-0.151824997028116,-0.148277425274246,-0.12652726456846,
-0.105236270462937,-0.0835127492652271,-0.0784406535722348,-0.0733870619889256,
-0.0516031153801045,-0.029512914496819,-0.0074997402847098,0.),
 .UNSPECIFIED.);
#1550=B_SPLINE_CURVE_WITH_KNOTS('',3,(#63108,#63109,#63110,#63111,#63112,
#63113,#63114,#63115),.UNSPECIFIED.,.F.,.F.,(4,1,1,1,1,4),(11.6154215191105,
12.6127573616628,13.610093204215,14.6074290467673,15.6047648893195,15.7079632679489),
 .UNSPECIFIED.);
#1551=B_SPLINE_CURVE_WITH_KNOTS('',3,(#63116,#63117,#63118,#63119,#63120,
#63121,#63122,#63123,#63124,#63125,#63126,#63127,#63128,#63129,#63130,#63131,
#63132,#63133,#63134,#63135,#63136,#63137,#63138,#63139,#63140,#63141,#63142,
#63143,#63144,#63145,#63146,#63147,#63148,#63149,#63150,#63151,#63152,#63153,
#63154,#63155,#63156,#63157,#63158,#63159,#63160,#63161,#63162,#63163,#63164,
#63165,#63166,#63167,#63168,#63169,#63170,#63171,#63172,#63173,#63174,#63175,
#63176,#63177,#63178,#63179,#63180,#63181,#63182,#63183,#63184,#63185,#63186,
#63187,#63188,#63189,#63190,#63191,#63192,#63193,#63194,#63195,#63196,#63197,
#63198,#63199,#63200),.UNSPECIFIED.,.F.,.F.,(4,3,3,3,3,3,3,3,3,3,3,3,3,
3,3,3,3,3,3,3,3,3,3,3,3,3,3,3,4),(-0.364629307890661,-0.350885759085945,
-0.329296488089375,-0.318978386270927,-0.313741431878983,-0.309365163672801,
-0.288042901568511,-0.272809238661881,-0.264006177467146,-0.26029818106468,
-0.239567096461013,-0.219346880276472,-0.206053559786221,-0.194876880502573,
-0.191399047668888,-0.171813366976952,-0.166173598315468,-0.145401898526034,
-0.126706873608775,-0.123379860192083,-0.103925496661725,-0.0845481894111439,
-0.065567586070534,-0.0621782887363481,-0.05894467115978,-0.0403543924373443,
-0.0220984153978596,-0.00442511140790438,0.),.UNSPECIFIED.);
#1552=B_SPLINE_CURVE_WITH_KNOTS('',3,(#63201,#63202,#63203,#63204,#63205,
#63206,#63207,#63208,#63209,#63210,#63211,#63212,#63213),.UNSPECIFIED.,
 .F.,.F.,(4,3,3,3,4),(-101.213804280572,-100.730920097777,-99.7335842552244,
-98.7362484126722,-98.3403213565322),.UNSPECIFIED.);
#1553=B_SPLINE_CURVE_WITH_KNOTS('',3,(#63216,#63217,#63218,#63219,#63220,
#63221,#63222,#63223,#63224),.UNSPECIFIED.,.F.,.F.,(4,1,1,1,1,1,4),(10.3757270560178,
11.30460783463,12.30261480526,13.3006217758901,14.2986287465202,15.2966357171503,
15.7079632679489),.UNSPECIFIED.);
#1554=B_SPLINE_CURVE_WITH_KNOTS('',3,(#63658,#63659,#63660,#63661,#63662,
#63663,#63664,#63665,#63666,#63667,#63668,#63669,#63670,#63671,#63672,#63673),
 .UNSPECIFIED.,.F.,.F.,(4,3,3,3,3,4),(95.3619706457233,95.8086691804886,
96.8066761511186,97.8046831217487,98.8026900923788,99.1486641472938),
 .UNSPECIFIED.);
#1555=B_SPLINE_CURVE_WITH_KNOTS('',3,(#63674,#63675,#63676,#63677,#63678,
#63679,#63680,#63681,#63682,#63683,#63684,#63685,#63686,#63687,#63688,#63689,
#63690,#63691,#63692,#63693,#63694,#63695,#63696,#63697,#63698,#63699,#63700,
#63701,#63702,#63703,#63704,#63705,#63706,#63707,#63708,#63709,#63710,#63711,
#63712,#63713,#63714,#63715,#63716,#63717,#63718,#63719,#63720,#63721,#63722,
#63723,#63724,#63725,#63726,#63727,#63728,#63729,#63730,#63731,#63732,#63733,
#63734,#63735,#63736,#63737,#63738,#63739,#63740,#63741,#63742,#63743,#63744,
#63745,#63746,#63747,#63748,#63749,#63750,#63751,#63752,#63753,#63754,#63755,
#63756,#63757,#63758),.UNSPECIFIED.,.F.,.F.,(4,3,3,3,3,3,3,3,3,3,3,3,3,
3,3,3,3,3,3,3,3,3,3,3,3,3,3,3,4),(-0.366397579005845,-0.355461226466819,
-0.337490969642209,-0.327214164040339,-0.321649482146298,-0.302840833811487,
-0.288386907394637,-0.281257238921911,-0.277593927902022,-0.258153123971634,
-0.238335729520815,-0.225554152759783,-0.218411056976172,-0.214856426708649,
-0.194426531587897,-0.187209422476688,-0.167504451243421,-0.156894426252658,
-0.149523127563347,-0.145921626399787,-0.125494957624892,-0.104619107174947,
-0.0835512936559854,-0.0752831225832569,-0.0721648689176682,-0.0505208253811386,
-0.028827309118007,-0.00759789023731293,0.),.UNSPECIFIED.);
#1556=SHAPE_REPRESENTATION_RELATIONSHIP('SRR','None',#63995,#1574);
#1557=SHAPE_REPRESENTATION_RELATIONSHIP('SRR','None',#63996,#1575);
#1558=SHAPE_REPRESENTATION_RELATIONSHIP('SRR','None',#63997,#1576);
#1559=SHAPE_REPRESENTATION_RELATIONSHIP('SRR','None',#63998,#1577);
#1560=SHAPE_REPRESENTATION_RELATIONSHIP('SRR','None',#63999,#1578);
#1561=SHAPE_REPRESENTATION_RELATIONSHIP('SRR','None',#64000,#1579);
#1562=SHAPE_REPRESENTATION_RELATIONSHIP('SRR','None',#64001,#1580);
#1563=SHAPE_REPRESENTATION_RELATIONSHIP('SRR','None',#64002,#1581);
#1564=SHAPE_REPRESENTATION_RELATIONSHIP('SRR','None',#64003,#1582);
#1565=SHAPE_REPRESENTATION_RELATIONSHIP('SRR','None',#64004,#1583);
#1566=SHAPE_REPRESENTATION_RELATIONSHIP('SRR','None',#64005,#1584);
#1567=SHAPE_REPRESENTATION_RELATIONSHIP('SRR','None',#64006,#1585);
#1568=SHAPE_REPRESENTATION_RELATIONSHIP('SRR','None',#64007,#1586);
#1569=SHAPE_REPRESENTATION_RELATIONSHIP('SRR','None',#64008,#1587);
#1570=SHAPE_REPRESENTATION_RELATIONSHIP('SRR','None',#64009,#1588);
#1571=SHAPE_REPRESENTATION_RELATIONSHIP('SRR','None',#64010,#1589);
#1572=SHAPE_REPRESENTATION_RELATIONSHIP('SRR','None',#64011,#1590);
#1573=SHAPE_REPRESENTATION_RELATIONSHIP('SRR','None',#64012,#1591);
#1574=ADVANCED_BREP_SHAPE_REPRESENTATION('',(#1610),#63880);
#1575=ADVANCED_BREP_SHAPE_REPRESENTATION('',(#1611),#63881);
#1576=ADVANCED_BREP_SHAPE_REPRESENTATION('',(#1612),#63882);
#1577=ADVANCED_BREP_SHAPE_REPRESENTATION('',(#1613),#63883);
#1578=ADVANCED_BREP_SHAPE_REPRESENTATION('',(#1614),#63884);
#1579=ADVANCED_BREP_SHAPE_REPRESENTATION('',(#1615),#63885);
#1580=ADVANCED_BREP_SHAPE_REPRESENTATION('',(#1616),#63886);
#1581=ADVANCED_BREP_SHAPE_REPRESENTATION('',(#1617),#63887);
#1582=ADVANCED_BREP_SHAPE_REPRESENTATION('',(#1618),#63888);
#1583=ADVANCED_BREP_SHAPE_REPRESENTATION('',(#1619),#63889);
#1584=ADVANCED_BREP_SHAPE_REPRESENTATION('',(#1620),#63890);
#1585=ADVANCED_BREP_SHAPE_REPRESENTATION('',(#1621),#63891);
#1586=ADVANCED_BREP_SHAPE_REPRESENTATION('',(#1622),#63892);
#1587=ADVANCED_BREP_SHAPE_REPRESENTATION('',(#1623),#63893);
#1588=ADVANCED_BREP_SHAPE_REPRESENTATION('',(#1624),#63894);
#1589=ADVANCED_BREP_SHAPE_REPRESENTATION('',(#1625),#63895);
#1590=ADVANCED_BREP_SHAPE_REPRESENTATION('',(#1626),#63896);
#1591=ADVANCED_BREP_SHAPE_REPRESENTATION('',(#1627),#63897);
#1592=STYLED_ITEM('',(#64094),#1610);
#1593=STYLED_ITEM('',(#64095),#1611);
#1594=STYLED_ITEM('',(#64096),#1612);
#1595=STYLED_ITEM('',(#64097),#1613);
#1596=STYLED_ITEM('',(#64098),#1614);
#1597=STYLED_ITEM('',(#64099),#1615);
#1598=STYLED_ITEM('',(#64098),#1616);
#1599=STYLED_ITEM('',(#64098),#1617);
#1600=STYLED_ITEM('',(#64097),#1618);
#1601=STYLED_ITEM('',(#64099),#1619);
#1602=STYLED_ITEM('',(#64100),#1620);
#1603=STYLED_ITEM('',(#64101),#1621);
#1604=STYLED_ITEM('',(#64102),#1622);
#1605=STYLED_ITEM('',(#64103),#1623);
#1606=STYLED_ITEM('',(#64104),#1624);
#1607=STYLED_ITEM('',(#64105),#1625);
#1608=STYLED_ITEM('',(#64097),#1626);
#1609=STYLED_ITEM('',(#64099),#1627);
#1610=MANIFOLD_SOLID_BREP('Body1',#15478);
#1611=MANIFOLD_SOLID_BREP('Body1',#15479);
#1612=MANIFOLD_SOLID_BREP('Body1',#15480);
#1613=MANIFOLD_SOLID_BREP('Body1',#15481);
#1614=MANIFOLD_SOLID_BREP('Body1',#15482);
#1615=MANIFOLD_SOLID_BREP('Body1',#15483);
#1616=MANIFOLD_SOLID_BREP('Body1',#15484);
#1617=MANIFOLD_SOLID_BREP('Body1',#15485);
#1618=MANIFOLD_SOLID_BREP('Body1',#15486);
#1619=MANIFOLD_SOLID_BREP('Body1',#15487);
#1620=MANIFOLD_SOLID_BREP('Body1',#15488);
#1621=MANIFOLD_SOLID_BREP('Body1',#15489);
#1622=MANIFOLD_SOLID_BREP('Body1',#15490);
#1623=MANIFOLD_SOLID_BREP('Body1',#15491);
#1624=MANIFOLD_SOLID_BREP('Body1',#15492);
#1625=MANIFOLD_SOLID_BREP('Body1',#15493);
#1626=MANIFOLD_SOLID_BREP('Body1',#15494);
#1627=MANIFOLD_SOLID_BREP('Body1',#15495);
#1628=FACE_BOUND('',#3516,.T.);
#1629=FACE_BOUND('',#3518,.T.);
#1630=FACE_BOUND('',#3519,.T.);
#1631=FACE_BOUND('',#3520,.T.);
#1632=FACE_BOUND('',#3521,.T.);
#1633=FACE_BOUND('',#3522,.T.);
#1634=FACE_BOUND('',#3523,.T.);
#1635=FACE_BOUND('',#3525,.T.);
#1636=FACE_BOUND('',#3526,.T.);
#1637=FACE_BOUND('',#3527,.T.);
#1638=FACE_BOUND('',#3528,.T.);
#1639=FACE_BOUND('',#3529,.T.);
#1640=FACE_BOUND('',#3530,.T.);
#1641=FACE_BOUND('',#3535,.T.);
#1642=FACE_BOUND('',#3536,.T.);
#1643=FACE_BOUND('',#3538,.T.);
#1644=FACE_BOUND('',#3901,.T.);
#1645=FACE_BOUND('',#3902,.T.);
#1646=FACE_BOUND('',#3903,.T.);
#1647=FACE_BOUND('',#3904,.T.);
#1648=FACE_BOUND('',#3905,.T.);
#1649=FACE_BOUND('',#3910,.T.);
#1650=FACE_BOUND('',#3916,.T.);
#1651=FACE_BOUND('',#3918,.T.);
#1652=FACE_BOUND('',#3920,.T.);
#1653=FACE_BOUND('',#3924,.T.);
#1654=FACE_BOUND('',#3926,.T.);
#1655=FACE_BOUND('',#3931,.T.);
#1656=FACE_BOUND('',#3933,.T.);
#1657=FACE_BOUND('',#3934,.T.);
#1658=FACE_BOUND('',#3935,.T.);
#1659=FACE_BOUND('',#3936,.T.);
#1660=FACE_BOUND('',#3937,.T.);
#1661=FACE_BOUND('',#3976,.T.);
#1662=FACE_BOUND('',#3978,.T.);
#1663=FACE_BOUND('',#3985,.T.);
#1664=FACE_BOUND('',#3997,.T.);
#1665=FACE_BOUND('',#3999,.T.);
#1666=FACE_BOUND('',#4003,.T.);
#1667=FACE_BOUND('',#4005,.T.);
#1668=FACE_BOUND('',#4007,.T.);
#1669=FACE_BOUND('',#4012,.T.);
#1670=FACE_BOUND('',#4014,.T.);
#1671=FACE_BOUND('',#4018,.T.);
#1672=FACE_BOUND('',#4020,.T.);
#1673=FACE_BOUND('',#4196,.T.);
#1674=FACE_BOUND('',#4198,.T.);
#1675=FACE_BOUND('',#4212,.T.);
#1676=FACE_BOUND('',#4213,.T.);
#1677=FACE_BOUND('',#4214,.T.);
#1678=FACE_BOUND('',#4215,.T.);
#1679=FACE_BOUND('',#4216,.T.);
#1680=FACE_BOUND('',#4217,.T.);
#1681=FACE_BOUND('',#4218,.T.);
#1682=FACE_BOUND('',#4221,.T.);
#1683=FACE_BOUND('',#4222,.T.);
#1684=FACE_BOUND('',#4223,.T.);
#1685=FACE_BOUND('',#4224,.T.);
#1686=FACE_BOUND('',#4225,.T.);
#1687=FACE_BOUND('',#4226,.T.);
#1688=FACE_BOUND('',#4228,.T.);
#1689=FACE_BOUND('',#4233,.T.);
#1690=FACE_BOUND('',#4235,.T.);
#1691=FACE_BOUND('',#4291,.T.);
#1692=FACE_BOUND('',#4293,.T.);
#1693=FACE_BOUND('',#4297,.T.);
#1694=FACE_BOUND('',#4301,.T.);
#1695=FACE_BOUND('',#4305,.T.);
#1696=FACE_BOUND('',#4311,.T.);
#1697=FACE_BOUND('',#4312,.T.);
#1698=FACE_BOUND('',#4313,.T.);
#1699=FACE_BOUND('',#4314,.T.);
#1700=FACE_BOUND('',#4315,.T.);
#1701=FACE_BOUND('',#4317,.T.);
#1702=FACE_BOUND('',#4318,.T.);
#1703=FACE_BOUND('',#4319,.T.);
#1704=FACE_BOUND('',#4320,.T.);
#1705=FACE_BOUND('',#4321,.T.);
#1706=FACE_BOUND('',#4327,.T.);
#1707=FACE_BOUND('',#4329,.T.);
#1708=FACE_BOUND('',#4335,.T.);
#1709=FACE_BOUND('',#4337,.T.);
#1710=FACE_BOUND('',#4365,.T.);
#1711=FACE_BOUND('',#4370,.T.);
#1712=FACE_BOUND('',#4372,.T.);
#1713=FACE_BOUND('',#4418,.T.);
#1714=FACE_BOUND('',#4421,.T.);
#1715=CYLINDRICAL_SURFACE('',#15709,12.);
#1716=CYLINDRICAL_SURFACE('',#15711,70.);
#1717=CYLINDRICAL_SURFACE('',#15717,8.);
#1718=CYLINDRICAL_SURFACE('',#15720,8.);
#1719=CYLINDRICAL_SURFACE('',#15723,5.5);
#1720=CYLINDRICAL_SURFACE('',#15726,5.5);
#1721=CYLINDRICAL_SURFACE('',#15729,5.5);
#1722=CYLINDRICAL_SURFACE('',#15732,5.5);
#1723=CYLINDRICAL_SURFACE('',#15744,100.);
#1724=CYLINDRICAL_SURFACE('',#15745,70.);
#1725=CYLINDRICAL_SURFACE('',#15747,50.);
#1726=CYLINDRICAL_SURFACE('',#15753,5.13675);
#1727=CYLINDRICAL_SURFACE('',#15755,5.13675);
#1728=CYLINDRICAL_SURFACE('',#15757,5.13675);
#1729=CYLINDRICAL_SURFACE('',#15758,5.13675);
#1730=CYLINDRICAL_SURFACE('',#15759,5.13675);
#1731=CYLINDRICAL_SURFACE('',#15760,5.13675);
#1732=CYLINDRICAL_SURFACE('',#15761,5.13675);
#1733=CYLINDRICAL_SURFACE('',#15763,6.11325000000001);
#1734=CYLINDRICAL_SURFACE('',#15765,6.11325000000001);
#1735=CYLINDRICAL_SURFACE('',#15766,6.11325000000001);
#1736=CYLINDRICAL_SURFACE('',#15767,6.11325000000001);
#1737=CYLINDRICAL_SURFACE('',#15768,6.11325000000001);
#1738=CYLINDRICAL_SURFACE('',#15769,6.11325000000001);
#1739=CYLINDRICAL_SURFACE('',#15770,6.11325000000001);
#1740=CYLINDRICAL_SURFACE('',#15772,1.666);
#1741=CYLINDRICAL_SURFACE('',#15776,1.666);
#1742=CYLINDRICAL_SURFACE('',#15777,1.666);
#1743=CYLINDRICAL_SURFACE('',#15778,1.666);
#1744=CYLINDRICAL_SURFACE('',#15779,1.666);
#1745=CYLINDRICAL_SURFACE('',#15780,1.666);
#1746=CYLINDRICAL_SURFACE('',#15781,1.666);
#1747=CYLINDRICAL_SURFACE('',#15782,1.666);
#1748=CYLINDRICAL_SURFACE('',#15783,1.666);
#1749=CYLINDRICAL_SURFACE('',#15784,1.666);
#1750=CYLINDRICAL_SURFACE('',#15785,1.666);
#1751=CYLINDRICAL_SURFACE('',#15786,1.666);
#1752=CYLINDRICAL_SURFACE('',#15787,1.666);
#1753=CYLINDRICAL_SURFACE('',#15788,1.666);
#1754=CYLINDRICAL_SURFACE('',#15789,1.666);
#1755=CYLINDRICAL_SURFACE('',#15790,1.666);
#1756=CYLINDRICAL_SURFACE('',#15791,1.666);
#1757=CYLINDRICAL_SURFACE('',#15792,1.666);
#1758=CYLINDRICAL_SURFACE('',#15794,2.05475);
#1759=CYLINDRICAL_SURFACE('',#15796,2.05475);
#1760=CYLINDRICAL_SURFACE('',#15797,2.05475);
#1761=CYLINDRICAL_SURFACE('',#15798,2.05475);
#1762=CYLINDRICAL_SURFACE('',#15799,2.05475);
#1763=CYLINDRICAL_SURFACE('',#15800,2.05475);
#1764=CYLINDRICAL_SURFACE('',#15801,2.05475);
#1765=CYLINDRICAL_SURFACE('',#15802,2.05475);
#1766=CYLINDRICAL_SURFACE('',#15803,2.05475);
#1767=CYLINDRICAL_SURFACE('',#15804,2.05475);
#1768=CYLINDRICAL_SURFACE('',#15805,2.05475);
#1769=CYLINDRICAL_SURFACE('',#15806,2.05475);
#1770=CYLINDRICAL_SURFACE('',#15807,2.05475);
#1771=CYLINDRICAL_SURFACE('',#15808,2.05475);
#1772=CYLINDRICAL_SURFACE('',#15809,2.05475);
#1773=CYLINDRICAL_SURFACE('',#15810,2.05475);
#1774=CYLINDRICAL_SURFACE('',#15811,2.05475);
#1775=CYLINDRICAL_SURFACE('',#15812,2.05475);
#1776=CYLINDRICAL_SURFACE('',#15813,2.05475);
#1777=CYLINDRICAL_SURFACE('',#15815,1.666);
#1778=CYLINDRICAL_SURFACE('',#15819,1.666);
#1779=CYLINDRICAL_SURFACE('',#15820,1.666);
#1780=CYLINDRICAL_SURFACE('',#15821,1.666);
#1781=CYLINDRICAL_SURFACE('',#15822,1.666);
#1782=CYLINDRICAL_SURFACE('',#15823,1.666);
#1783=CYLINDRICAL_SURFACE('',#15824,1.666);
#1784=CYLINDRICAL_SURFACE('',#15825,1.666);
#1785=CYLINDRICAL_SURFACE('',#15826,1.666);
#1786=CYLINDRICAL_SURFACE('',#15827,1.666);
#1787=CYLINDRICAL_SURFACE('',#15828,1.666);
#1788=CYLINDRICAL_SURFACE('',#15829,1.666);
#1789=CYLINDRICAL_SURFACE('',#15830,1.666);
#1790=CYLINDRICAL_SURFACE('',#15831,1.666);
#1791=CYLINDRICAL_SURFACE('',#15832,1.666);
#1792=CYLINDRICAL_SURFACE('',#15833,1.666);
#1793=CYLINDRICAL_SURFACE('',#15834,1.666);
#1794=CYLINDRICAL_SURFACE('',#15835,1.666);
#1795=CYLINDRICAL_SURFACE('',#15837,2.05475);
#1796=CYLINDRICAL_SURFACE('',#15839,2.05475);
#1797=CYLINDRICAL_SURFACE('',#15840,2.05475);
#1798=CYLINDRICAL_SURFACE('',#15841,2.05475);
#1799=CYLINDRICAL_SURFACE('',#15842,2.05475);
#1800=CYLINDRICAL_SURFACE('',#15843,2.05475);
#1801=CYLINDRICAL_SURFACE('',#15844,2.05475);
#1802=CYLINDRICAL_SURFACE('',#15845,2.05475);
#1803=CYLINDRICAL_SURFACE('',#15846,2.05475);
#1804=CYLINDRICAL_SURFACE('',#15847,2.05475);
#1805=CYLINDRICAL_SURFACE('',#15848,2.05475);
#1806=CYLINDRICAL_SURFACE('',#15849,2.05475);
#1807=CYLINDRICAL_SURFACE('',#15850,2.05475);
#1808=CYLINDRICAL_SURFACE('',#15851,2.05475);
#1809=CYLINDRICAL_SURFACE('',#15852,2.05475);
#1810=CYLINDRICAL_SURFACE('',#15853,2.05475);
#1811=CYLINDRICAL_SURFACE('',#15854,2.05475);
#1812=CYLINDRICAL_SURFACE('',#15855,2.05475);
#1813=CYLINDRICAL_SURFACE('',#15856,2.05475);
#1814=CYLINDRICAL_SURFACE('',#15858,1.666);
#1815=CYLINDRICAL_SURFACE('',#15862,1.666);
#1816=CYLINDRICAL_SURFACE('',#15863,1.666);
#1817=CYLINDRICAL_SURFACE('',#15864,1.666);
#1818=CYLINDRICAL_SURFACE('',#15865,1.666);
#1819=CYLINDRICAL_SURFACE('',#15866,1.666);
#1820=CYLINDRICAL_SURFACE('',#15867,1.666);
#1821=CYLINDRICAL_SURFACE('',#15868,1.666);
#1822=CYLINDRICAL_SURFACE('',#15869,1.666);
#1823=CYLINDRICAL_SURFACE('',#15870,1.666);
#1824=CYLINDRICAL_SURFACE('',#15871,1.666);
#1825=CYLINDRICAL_SURFACE('',#15872,1.666);
#1826=CYLINDRICAL_SURFACE('',#15873,1.666);
#1827=CYLINDRICAL_SURFACE('',#15874,1.666);
#1828=CYLINDRICAL_SURFACE('',#15875,1.666);
#1829=CYLINDRICAL_SURFACE('',#15876,1.666);
#1830=CYLINDRICAL_SURFACE('',#15877,1.666);
#1831=CYLINDRICAL_SURFACE('',#15878,1.666);
#1832=CYLINDRICAL_SURFACE('',#15880,2.05475);
#1833=CYLINDRICAL_SURFACE('',#15882,2.05475);
#1834=CYLINDRICAL_SURFACE('',#15883,2.05475);
#1835=CYLINDRICAL_SURFACE('',#15884,2.05475);
#1836=CYLINDRICAL_SURFACE('',#15885,2.05475);
#1837=CYLINDRICAL_SURFACE('',#15886,2.05475);
#1838=CYLINDRICAL_SURFACE('',#15887,2.05475);
#1839=CYLINDRICAL_SURFACE('',#15888,2.05475);
#1840=CYLINDRICAL_SURFACE('',#15889,2.05475);
#1841=CYLINDRICAL_SURFACE('',#15890,2.05475);
#1842=CYLINDRICAL_SURFACE('',#15891,2.05475);
#1843=CYLINDRICAL_SURFACE('',#15892,2.05475);
#1844=CYLINDRICAL_SURFACE('',#15893,2.05475);
#1845=CYLINDRICAL_SURFACE('',#15894,2.05475);
#1846=CYLINDRICAL_SURFACE('',#15895,2.05475);
#1847=CYLINDRICAL_SURFACE('',#15896,2.05475);
#1848=CYLINDRICAL_SURFACE('',#15897,2.05475);
#1849=CYLINDRICAL_SURFACE('',#15898,2.05475);
#1850=CYLINDRICAL_SURFACE('',#15899,2.05475);
#1851=CYLINDRICAL_SURFACE('',#15901,1.666);
#1852=CYLINDRICAL_SURFACE('',#15905,1.666);
#1853=CYLINDRICAL_SURFACE('',#15906,1.666);
#1854=CYLINDRICAL_SURFACE('',#15907,1.666);
#1855=CYLINDRICAL_SURFACE('',#15908,1.666);
#1856=CYLINDRICAL_SURFACE('',#15909,1.666);
#1857=CYLINDRICAL_SURFACE('',#15910,1.666);
#1858=CYLINDRICAL_SURFACE('',#15911,1.666);
#1859=CYLINDRICAL_SURFACE('',#15912,1.666);
#1860=CYLINDRICAL_SURFACE('',#15913,1.666);
#1861=CYLINDRICAL_SURFACE('',#15914,1.666);
#1862=CYLINDRICAL_SURFACE('',#15915,1.666);
#1863=CYLINDRICAL_SURFACE('',#15916,1.666);
#1864=CYLINDRICAL_SURFACE('',#15917,1.666);
#1865=CYLINDRICAL_SURFACE('',#15918,1.666);
#1866=CYLINDRICAL_SURFACE('',#15919,1.666);
#1867=CYLINDRICAL_SURFACE('',#15920,1.666);
#1868=CYLINDRICAL_SURFACE('',#15921,1.666);
#1869=CYLINDRICAL_SURFACE('',#15923,2.05475);
#1870=CYLINDRICAL_SURFACE('',#15925,2.05475);
#1871=CYLINDRICAL_SURFACE('',#15926,2.05475);
#1872=CYLINDRICAL_SURFACE('',#15927,2.05475);
#1873=CYLINDRICAL_SURFACE('',#15928,2.05475);
#1874=CYLINDRICAL_SURFACE('',#15929,2.05475);
#1875=CYLINDRICAL_SURFACE('',#15930,2.05475);
#1876=CYLINDRICAL_SURFACE('',#15931,2.05475);
#1877=CYLINDRICAL_SURFACE('',#15932,2.05475);
#1878=CYLINDRICAL_SURFACE('',#15933,2.05475);
#1879=CYLINDRICAL_SURFACE('',#15934,2.05475);
#1880=CYLINDRICAL_SURFACE('',#15935,2.05475);
#1881=CYLINDRICAL_SURFACE('',#15936,2.05475);
#1882=CYLINDRICAL_SURFACE('',#15937,2.05475);
#1883=CYLINDRICAL_SURFACE('',#15938,2.05475);
#1884=CYLINDRICAL_SURFACE('',#15939,2.05475);
#1885=CYLINDRICAL_SURFACE('',#15940,2.05475);
#1886=CYLINDRICAL_SURFACE('',#15941,2.05475);
#1887=CYLINDRICAL_SURFACE('',#15942,2.05475);
#1888=CYLINDRICAL_SURFACE('',#15944,1.666);
#1889=CYLINDRICAL_SURFACE('',#15948,1.666);
#1890=CYLINDRICAL_SURFACE('',#15949,1.666);
#1891=CYLINDRICAL_SURFACE('',#15950,1.666);
#1892=CYLINDRICAL_SURFACE('',#15951,1.666);
#1893=CYLINDRICAL_SURFACE('',#15952,1.666);
#1894=CYLINDRICAL_SURFACE('',#15953,1.666);
#1895=CYLINDRICAL_SURFACE('',#15954,1.666);
#1896=CYLINDRICAL_SURFACE('',#15955,1.666);
#1897=CYLINDRICAL_SURFACE('',#15956,1.666);
#1898=CYLINDRICAL_SURFACE('',#15957,1.666);
#1899=CYLINDRICAL_SURFACE('',#15958,1.666);
#1900=CYLINDRICAL_SURFACE('',#15959,1.666);
#1901=CYLINDRICAL_SURFACE('',#15960,1.666);
#1902=CYLINDRICAL_SURFACE('',#15961,1.666);
#1903=CYLINDRICAL_SURFACE('',#15962,1.666);
#1904=CYLINDRICAL_SURFACE('',#15963,1.666);
#1905=CYLINDRICAL_SURFACE('',#15964,1.666);
#1906=CYLINDRICAL_SURFACE('',#15966,2.05475);
#1907=CYLINDRICAL_SURFACE('',#15968,2.05475);
#1908=CYLINDRICAL_SURFACE('',#15969,2.05475);
#1909=CYLINDRICAL_SURFACE('',#15970,2.05475);
#1910=CYLINDRICAL_SURFACE('',#15971,2.05475);
#1911=CYLINDRICAL_SURFACE('',#15972,2.05475);
#1912=CYLINDRICAL_SURFACE('',#15973,2.05475);
#1913=CYLINDRICAL_SURFACE('',#15974,2.05475);
#1914=CYLINDRICAL_SURFACE('',#15975,2.05475);
#1915=CYLINDRICAL_SURFACE('',#15976,2.05475);
#1916=CYLINDRICAL_SURFACE('',#15977,2.05475);
#1917=CYLINDRICAL_SURFACE('',#15978,2.05475);
#1918=CYLINDRICAL_SURFACE('',#15979,2.05475);
#1919=CYLINDRICAL_SURFACE('',#15980,2.05475);
#1920=CYLINDRICAL_SURFACE('',#15981,2.05475);
#1921=CYLINDRICAL_SURFACE('',#15982,2.05475);
#1922=CYLINDRICAL_SURFACE('',#15983,2.05475);
#1923=CYLINDRICAL_SURFACE('',#15984,2.05475);
#1924=CYLINDRICAL_SURFACE('',#15985,2.05475);
#1925=CYLINDRICAL_SURFACE('',#15987,1.666);
#1926=CYLINDRICAL_SURFACE('',#15991,1.666);
#1927=CYLINDRICAL_SURFACE('',#15992,1.666);
#1928=CYLINDRICAL_SURFACE('',#15993,1.666);
#1929=CYLINDRICAL_SURFACE('',#15994,1.666);
#1930=CYLINDRICAL_SURFACE('',#15995,1.666);
#1931=CYLINDRICAL_SURFACE('',#15996,1.666);
#1932=CYLINDRICAL_SURFACE('',#15997,1.666);
#1933=CYLINDRICAL_SURFACE('',#15998,1.666);
#1934=CYLINDRICAL_SURFACE('',#15999,1.666);
#1935=CYLINDRICAL_SURFACE('',#16000,1.666);
#1936=CYLINDRICAL_SURFACE('',#16001,1.666);
#1937=CYLINDRICAL_SURFACE('',#16002,1.666);
#1938=CYLINDRICAL_SURFACE('',#16003,1.666);
#1939=CYLINDRICAL_SURFACE('',#16004,1.666);
#1940=CYLINDRICAL_SURFACE('',#16005,1.666);
#1941=CYLINDRICAL_SURFACE('',#16006,1.666);
#1942=CYLINDRICAL_SURFACE('',#16007,1.666);
#1943=CYLINDRICAL_SURFACE('',#16009,2.05475000000001);
#1944=CYLINDRICAL_SURFACE('',#16011,2.05475000000001);
#1945=CYLINDRICAL_SURFACE('',#16012,2.05475000000001);
#1946=CYLINDRICAL_SURFACE('',#16013,2.05475000000001);
#1947=CYLINDRICAL_SURFACE('',#16014,2.05475000000001);
#1948=CYLINDRICAL_SURFACE('',#16015,2.05475000000001);
#1949=CYLINDRICAL_SURFACE('',#16016,2.05475000000001);
#1950=CYLINDRICAL_SURFACE('',#16017,2.05475000000001);
#1951=CYLINDRICAL_SURFACE('',#16018,2.05475000000001);
#1952=CYLINDRICAL_SURFACE('',#16019,2.05475000000001);
#1953=CYLINDRICAL_SURFACE('',#16020,2.05475000000001);
#1954=CYLINDRICAL_SURFACE('',#16021,2.05475000000001);
#1955=CYLINDRICAL_SURFACE('',#16022,2.05475000000001);
#1956=CYLINDRICAL_SURFACE('',#16023,2.05475000000001);
#1957=CYLINDRICAL_SURFACE('',#16024,2.05475000000001);
#1958=CYLINDRICAL_SURFACE('',#16025,2.05475000000001);
#1959=CYLINDRICAL_SURFACE('',#16026,2.05475000000001);
#1960=CYLINDRICAL_SURFACE('',#16027,2.05475000000001);
#1961=CYLINDRICAL_SURFACE('',#16028,2.05475000000001);
#1962=CYLINDRICAL_SURFACE('',#16030,1.666);
#1963=CYLINDRICAL_SURFACE('',#16034,1.666);
#1964=CYLINDRICAL_SURFACE('',#16035,1.666);
#1965=CYLINDRICAL_SURFACE('',#16036,1.666);
#1966=CYLINDRICAL_SURFACE('',#16037,1.666);
#1967=CYLINDRICAL_SURFACE('',#16038,1.666);
#1968=CYLINDRICAL_SURFACE('',#16039,1.666);
#1969=CYLINDRICAL_SURFACE('',#16040,1.666);
#1970=CYLINDRICAL_SURFACE('',#16041,1.666);
#1971=CYLINDRICAL_SURFACE('',#16042,1.666);
#1972=CYLINDRICAL_SURFACE('',#16043,1.666);
#1973=CYLINDRICAL_SURFACE('',#16044,1.666);
#1974=CYLINDRICAL_SURFACE('',#16045,1.666);
#1975=CYLINDRICAL_SURFACE('',#16046,1.666);
#1976=CYLINDRICAL_SURFACE('',#16047,1.666);
#1977=CYLINDRICAL_SURFACE('',#16048,1.666);
#1978=CYLINDRICAL_SURFACE('',#16049,1.666);
#1979=CYLINDRICAL_SURFACE('',#16050,1.666);
#1980=CYLINDRICAL_SURFACE('',#16052,2.05475);
#1981=CYLINDRICAL_SURFACE('',#16054,2.05475);
#1982=CYLINDRICAL_SURFACE('',#16055,2.05475);
#1983=CYLINDRICAL_SURFACE('',#16056,2.05475);
#1984=CYLINDRICAL_SURFACE('',#16057,2.05475);
#1985=CYLINDRICAL_SURFACE('',#16058,2.05475);
#1986=CYLINDRICAL_SURFACE('',#16059,2.05475);
#1987=CYLINDRICAL_SURFACE('',#16060,2.05475);
#1988=CYLINDRICAL_SURFACE('',#16061,2.05475);
#1989=CYLINDRICAL_SURFACE('',#16062,2.05475);
#1990=CYLINDRICAL_SURFACE('',#16063,2.05475);
#1991=CYLINDRICAL_SURFACE('',#16064,2.05475);
#1992=CYLINDRICAL_SURFACE('',#16065,2.05475);
#1993=CYLINDRICAL_SURFACE('',#16066,2.05475);
#1994=CYLINDRICAL_SURFACE('',#16067,2.05475);
#1995=CYLINDRICAL_SURFACE('',#16068,2.05475);
#1996=CYLINDRICAL_SURFACE('',#16069,2.05475);
#1997=CYLINDRICAL_SURFACE('',#16070,2.05475);
#1998=CYLINDRICAL_SURFACE('',#16071,2.05475);
#1999=CYLINDRICAL_SURFACE('',#16073,1.666);
#2000=CYLINDRICAL_SURFACE('',#16077,1.666);
#2001=CYLINDRICAL_SURFACE('',#16078,1.666);
#2002=CYLINDRICAL_SURFACE('',#16079,1.666);
#2003=CYLINDRICAL_SURFACE('',#16080,1.666);
#2004=CYLINDRICAL_SURFACE('',#16081,1.666);
#2005=CYLINDRICAL_SURFACE('',#16082,1.666);
#2006=CYLINDRICAL_SURFACE('',#16083,1.666);
#2007=CYLINDRICAL_SURFACE('',#16084,1.666);
#2008=CYLINDRICAL_SURFACE('',#16085,1.666);
#2009=CYLINDRICAL_SURFACE('',#16086,1.666);
#2010=CYLINDRICAL_SURFACE('',#16087,1.666);
#2011=CYLINDRICAL_SURFACE('',#16088,1.666);
#2012=CYLINDRICAL_SURFACE('',#16089,1.666);
#2013=CYLINDRICAL_SURFACE('',#16090,1.666);
#2014=CYLINDRICAL_SURFACE('',#16091,1.666);
#2015=CYLINDRICAL_SURFACE('',#16092,1.666);
#2016=CYLINDRICAL_SURFACE('',#16093,1.666);
#2017=CYLINDRICAL_SURFACE('',#16095,2.05475000000001);
#2018=CYLINDRICAL_SURFACE('',#16097,2.05475000000001);
#2019=CYLINDRICAL_SURFACE('',#16098,2.05475000000001);
#2020=CYLINDRICAL_SURFACE('',#16099,2.05475000000001);
#2021=CYLINDRICAL_SURFACE('',#16100,2.05475000000001);
#2022=CYLINDRICAL_SURFACE('',#16101,2.05475000000001);
#2023=CYLINDRICAL_SURFACE('',#16102,2.05475000000001);
#2024=CYLINDRICAL_SURFACE('',#16103,2.05475000000001);
#2025=CYLINDRICAL_SURFACE('',#16104,2.05475000000001);
#2026=CYLINDRICAL_SURFACE('',#16105,2.05475000000001);
#2027=CYLINDRICAL_SURFACE('',#16106,2.05475000000001);
#2028=CYLINDRICAL_SURFACE('',#16107,2.05475000000001);
#2029=CYLINDRICAL_SURFACE('',#16108,2.05475000000001);
#2030=CYLINDRICAL_SURFACE('',#16109,2.05475000000001);
#2031=CYLINDRICAL_SURFACE('',#16110,2.05475000000001);
#2032=CYLINDRICAL_SURFACE('',#16111,2.05475000000001);
#2033=CYLINDRICAL_SURFACE('',#16112,2.05475000000001);
#2034=CYLINDRICAL_SURFACE('',#16113,2.05475000000001);
#2035=CYLINDRICAL_SURFACE('',#16114,2.05475000000001);
#2036=CYLINDRICAL_SURFACE('',#16117,2.05475000000001);
#2037=CYLINDRICAL_SURFACE('',#16118,1.666);
#2038=CYLINDRICAL_SURFACE('',#16120,2.05475);
#2039=CYLINDRICAL_SURFACE('',#16121,1.666);
#2040=CYLINDRICAL_SURFACE('',#16123,2.05475000000001);
#2041=CYLINDRICAL_SURFACE('',#16124,1.666);
#2042=CYLINDRICAL_SURFACE('',#16126,2.05475);
#2043=CYLINDRICAL_SURFACE('',#16127,1.666);
#2044=CYLINDRICAL_SURFACE('',#16133,2.05475);
#2045=CYLINDRICAL_SURFACE('',#16134,1.666);
#2046=CYLINDRICAL_SURFACE('',#16136,2.05475);
#2047=CYLINDRICAL_SURFACE('',#16137,1.666);
#2048=CYLINDRICAL_SURFACE('',#16139,2.05475);
#2049=CYLINDRICAL_SURFACE('',#16140,1.666);
#2050=CYLINDRICAL_SURFACE('',#16142,2.05475);
#2051=CYLINDRICAL_SURFACE('',#16143,1.666);
#2052=CYLINDRICAL_SURFACE('',#16154,6.11325000000001);
#2053=CYLINDRICAL_SURFACE('',#16157,5.13675);
#2054=CYLINDRICAL_SURFACE('',#16169,35.);
#2055=CYLINDRICAL_SURFACE('',#16170,40.);
#2056=CYLINDRICAL_SURFACE('',#16177,35.);
#2057=CYLINDRICAL_SURFACE('',#16178,40.);
#2058=CYLINDRICAL_SURFACE('',#16179,40.);
#2059=CYLINDRICAL_SURFACE('',#16181,50.);
#2060=CYLINDRICAL_SURFACE('',#16185,2.5175);
#2061=CYLINDRICAL_SURFACE('',#16188,2.5175);
#2062=CYLINDRICAL_SURFACE('',#16189,2.5175);
#2063=CYLINDRICAL_SURFACE('',#16190,2.5175);
#2064=CYLINDRICAL_SURFACE('',#16191,2.5175);
#2065=CYLINDRICAL_SURFACE('',#16192,2.5175);
#2066=CYLINDRICAL_SURFACE('',#16193,2.5175);
#2067=CYLINDRICAL_SURFACE('',#16194,2.5175);
#2068=CYLINDRICAL_SURFACE('',#16195,2.5175);
#2069=CYLINDRICAL_SURFACE('',#16196,2.5175);
#2070=CYLINDRICAL_SURFACE('',#16197,2.5175);
#2071=CYLINDRICAL_SURFACE('',#16198,2.5175);
#2072=CYLINDRICAL_SURFACE('',#16199,2.5175);
#2073=CYLINDRICAL_SURFACE('',#16200,2.5175);
#2074=CYLINDRICAL_SURFACE('',#16201,2.5175);
#2075=CYLINDRICAL_SURFACE('',#16202,2.5175);
#2076=CYLINDRICAL_SURFACE('',#16203,2.5175);
#2077=CYLINDRICAL_SURFACE('',#16204,2.5175);
#2078=CYLINDRICAL_SURFACE('',#16205,3.0735);
#2079=CYLINDRICAL_SURFACE('',#16208,3.0735);
#2080=CYLINDRICAL_SURFACE('',#16209,3.0735);
#2081=CYLINDRICAL_SURFACE('',#16210,3.0735);
#2082=CYLINDRICAL_SURFACE('',#16211,3.0735);
#2083=CYLINDRICAL_SURFACE('',#16212,3.0735);
#2084=CYLINDRICAL_SURFACE('',#16213,3.0735);
#2085=CYLINDRICAL_SURFACE('',#16214,3.0735);
#2086=CYLINDRICAL_SURFACE('',#16215,3.0735);
#2087=CYLINDRICAL_SURFACE('',#16216,3.0735);
#2088=CYLINDRICAL_SURFACE('',#16217,3.0735);
#2089=CYLINDRICAL_SURFACE('',#16218,3.0735);
#2090=CYLINDRICAL_SURFACE('',#16219,3.0735);
#2091=CYLINDRICAL_SURFACE('',#16220,3.0735);
#2092=CYLINDRICAL_SURFACE('',#16221,3.0735);
#2093=CYLINDRICAL_SURFACE('',#16222,3.0735);
#2094=CYLINDRICAL_SURFACE('',#16223,3.0735);
#2095=CYLINDRICAL_SURFACE('',#16224,3.0735);
#2096=CYLINDRICAL_SURFACE('',#16225,19.);
#2097=CYLINDRICAL_SURFACE('',#16232,20.);
#2098=CYLINDRICAL_SURFACE('',#16242,3.0735);
#2099=CYLINDRICAL_SURFACE('',#16244,2.5175);
#2100=CYLINDRICAL_SURFACE('',#16246,8.);
#2101=CYLINDRICAL_SURFACE('',#16250,12.);
#2102=CYLINDRICAL_SURFACE('',#16259,26.);
#2103=CYLINDRICAL_SURFACE('',#16260,20.);
#2104=CYLINDRICAL_SURFACE('',#16264,26.);
#2105=CYLINDRICAL_SURFACE('',#16267,20.);
#2106=CYLINDRICAL_SURFACE('',#16269,20.);
#2107=CYLINDRICAL_SURFACE('',#16272,27.);
#2108=CYLINDRICAL_SURFACE('',#16278,20.);
#2109=CYLINDRICAL_SURFACE('',#16281,27.5);
#2110=CYLINDRICAL_SURFACE('',#16292,19.);
#2111=CYLINDRICAL_SURFACE('',#16294,27.);
#2112=CYLINDRICAL_SURFACE('',#16305,5.91675);
#2113=CYLINDRICAL_SURFACE('',#16307,5.91675);
#2114=CYLINDRICAL_SURFACE('',#16308,5.91675);
#2115=CYLINDRICAL_SURFACE('',#16309,5.91675);
#2116=CYLINDRICAL_SURFACE('',#16310,5.91675);
#2117=CYLINDRICAL_SURFACE('',#16311,5.91675);
#2118=CYLINDRICAL_SURFACE('',#16312,5.91675);
#2119=CYLINDRICAL_SURFACE('',#16313,5.91675);
#2120=CYLINDRICAL_SURFACE('',#16314,5.91675);
#2121=CYLINDRICAL_SURFACE('',#16315,5.91675);
#2122=CYLINDRICAL_SURFACE('',#16316,5.91675);
#2123=CYLINDRICAL_SURFACE('',#16317,5.91675);
#2124=CYLINDRICAL_SURFACE('',#16318,5.91675);
#2125=CYLINDRICAL_SURFACE('',#16319,5.91675);
#2126=CYLINDRICAL_SURFACE('',#16320,5.91675);
#2127=CYLINDRICAL_SURFACE('',#16321,5.91675);
#2128=CYLINDRICAL_SURFACE('',#16322,5.91675);
#2129=CYLINDRICAL_SURFACE('',#16323,5.91675);
#2130=CYLINDRICAL_SURFACE('',#16324,5.91675);
#2131=CYLINDRICAL_SURFACE('',#16325,5.91675);
#2132=CYLINDRICAL_SURFACE('',#16326,5.91675);
#2133=CYLINDRICAL_SURFACE('',#16327,5.91675);
#2134=CYLINDRICAL_SURFACE('',#16328,5.91675);
#2135=CYLINDRICAL_SURFACE('',#16329,5.91675);
#2136=CYLINDRICAL_SURFACE('',#16330,5.91675);
#2137=CYLINDRICAL_SURFACE('',#16331,5.91675);
#2138=CYLINDRICAL_SURFACE('',#16332,5.91675);
#2139=CYLINDRICAL_SURFACE('',#16333,5.91675);
#2140=CYLINDRICAL_SURFACE('',#16334,5.91675);
#2141=CYLINDRICAL_SURFACE('',#16335,5.91675);
#2142=CYLINDRICAL_SURFACE('',#16336,5.91675);
#2143=CYLINDRICAL_SURFACE('',#16337,5.91675);
#2144=CYLINDRICAL_SURFACE('',#16338,5.91675);
#2145=CYLINDRICAL_SURFACE('',#16339,5.91675);
#2146=CYLINDRICAL_SURFACE('',#16340,5.91675);
#2147=CYLINDRICAL_SURFACE('',#16341,5.91675);
#2148=CYLINDRICAL_SURFACE('',#16342,5.91675);
#2149=CYLINDRICAL_SURFACE('',#16343,5.91675);
#2150=CYLINDRICAL_SURFACE('',#16344,5.91675);
#2151=CYLINDRICAL_SURFACE('',#16345,5.91675);
#2152=CYLINDRICAL_SURFACE('',#16346,5.91675);
#2153=CYLINDRICAL_SURFACE('',#16347,5.91675);
#2154=CYLINDRICAL_SURFACE('',#16348,5.91675);
#2155=CYLINDRICAL_SURFACE('',#16349,5.91675);
#2156=CYLINDRICAL_SURFACE('',#16350,5.91675);
#2157=CYLINDRICAL_SURFACE('',#16351,5.91675);
#2158=CYLINDRICAL_SURFACE('',#16352,5.91675);
#2159=CYLINDRICAL_SURFACE('',#16353,5.91675);
#2160=CYLINDRICAL_SURFACE('',#16354,5.91675);
#2161=CYLINDRICAL_SURFACE('',#16355,5.91675);
#2162=CYLINDRICAL_SURFACE('',#16356,5.91675);
#2163=CYLINDRICAL_SURFACE('',#16357,5.91675);
#2164=CYLINDRICAL_SURFACE('',#16358,5.91675);
#2165=CYLINDRICAL_SURFACE('',#16359,5.91675);
#2166=CYLINDRICAL_SURFACE('',#16360,5.91675);
#2167=CYLINDRICAL_SURFACE('',#16361,5.91675);
#2168=CYLINDRICAL_SURFACE('',#16362,5.91675);
#2169=CYLINDRICAL_SURFACE('',#16363,5.91675);
#2170=CYLINDRICAL_SURFACE('',#16364,5.91675);
#2171=CYLINDRICAL_SURFACE('',#16365,5.91675);
#2172=CYLINDRICAL_SURFACE('',#16366,5.91675);
#2173=CYLINDRICAL_SURFACE('',#16367,5.91675);
#2174=CYLINDRICAL_SURFACE('',#16368,5.91675);
#2175=CYLINDRICAL_SURFACE('',#16369,5.91675);
#2176=CYLINDRICAL_SURFACE('',#16370,5.91675);
#2177=CYLINDRICAL_SURFACE('',#16371,5.91675);
#2178=CYLINDRICAL_SURFACE('',#16372,5.91675);
#2179=CYLINDRICAL_SURFACE('',#16373,5.91675);
#2180=CYLINDRICAL_SURFACE('',#16374,5.91675);
#2181=CYLINDRICAL_SURFACE('',#16375,5.91675);
#2182=CYLINDRICAL_SURFACE('',#16376,5.91675);
#2183=CYLINDRICAL_SURFACE('',#16377,5.91675);
#2184=CYLINDRICAL_SURFACE('',#16378,5.91675);
#2185=CYLINDRICAL_SURFACE('',#16379,5.91675);
#2186=CYLINDRICAL_SURFACE('',#16380,5.91675);
#2187=CYLINDRICAL_SURFACE('',#16381,5.91675);
#2188=CYLINDRICAL_SURFACE('',#16382,5.91675);
#2189=CYLINDRICAL_SURFACE('',#16383,5.91675);
#2190=CYLINDRICAL_SURFACE('',#16384,5.91675);
#2191=CYLINDRICAL_SURFACE('',#16388,4.91825);
#2192=CYLINDRICAL_SURFACE('',#16390,4.91825);
#2193=CYLINDRICAL_SURFACE('',#16391,4.91825);
#2194=CYLINDRICAL_SURFACE('',#16392,4.91825);
#2195=CYLINDRICAL_SURFACE('',#16393,4.91825);
#2196=CYLINDRICAL_SURFACE('',#16394,4.91825);
#2197=CYLINDRICAL_SURFACE('',#16395,4.91825);
#2198=CYLINDRICAL_SURFACE('',#16396,4.91825);
#2199=CYLINDRICAL_SURFACE('',#16397,4.91825);
#2200=CYLINDRICAL_SURFACE('',#16398,4.91825);
#2201=CYLINDRICAL_SURFACE('',#16399,4.91825);
#2202=CYLINDRICAL_SURFACE('',#16400,4.91825);
#2203=CYLINDRICAL_SURFACE('',#16401,4.91825);
#2204=CYLINDRICAL_SURFACE('',#16402,4.91825);
#2205=CYLINDRICAL_SURFACE('',#16403,4.91825);
#2206=CYLINDRICAL_SURFACE('',#16404,4.91825);
#2207=CYLINDRICAL_SURFACE('',#16405,4.91825);
#2208=CYLINDRICAL_SURFACE('',#16406,4.91825);
#2209=CYLINDRICAL_SURFACE('',#16407,4.91825);
#2210=CYLINDRICAL_SURFACE('',#16408,4.91825);
#2211=CYLINDRICAL_SURFACE('',#16409,4.91825);
#2212=CYLINDRICAL_SURFACE('',#16410,4.91825);
#2213=CYLINDRICAL_SURFACE('',#16411,4.91825);
#2214=CYLINDRICAL_SURFACE('',#16412,4.91825);
#2215=CYLINDRICAL_SURFACE('',#16413,4.91825);
#2216=CYLINDRICAL_SURFACE('',#16414,4.91825);
#2217=CYLINDRICAL_SURFACE('',#16415,4.91825);
#2218=CYLINDRICAL_SURFACE('',#16416,4.91825);
#2219=CYLINDRICAL_SURFACE('',#16417,4.91825);
#2220=CYLINDRICAL_SURFACE('',#16418,4.91825);
#2221=CYLINDRICAL_SURFACE('',#16419,4.91825);
#2222=CYLINDRICAL_SURFACE('',#16420,4.91825);
#2223=CYLINDRICAL_SURFACE('',#16421,4.91825);
#2224=CYLINDRICAL_SURFACE('',#16422,4.91825);
#2225=CYLINDRICAL_SURFACE('',#16423,4.91825);
#2226=CYLINDRICAL_SURFACE('',#16424,4.91825);
#2227=CYLINDRICAL_SURFACE('',#16425,4.91825);
#2228=CYLINDRICAL_SURFACE('',#16426,4.91825);
#2229=CYLINDRICAL_SURFACE('',#16427,4.91825);
#2230=CYLINDRICAL_SURFACE('',#16428,4.91825);
#2231=CYLINDRICAL_SURFACE('',#16429,4.91825);
#2232=CYLINDRICAL_SURFACE('',#16430,4.91825);
#2233=CYLINDRICAL_SURFACE('',#16431,4.91825);
#2234=CYLINDRICAL_SURFACE('',#16432,4.91825);
#2235=CYLINDRICAL_SURFACE('',#16433,4.91825);
#2236=CYLINDRICAL_SURFACE('',#16434,4.91825);
#2237=CYLINDRICAL_SURFACE('',#16435,4.91825);
#2238=CYLINDRICAL_SURFACE('',#16436,4.91825);
#2239=CYLINDRICAL_SURFACE('',#16437,4.91825);
#2240=CYLINDRICAL_SURFACE('',#16438,4.91825);
#2241=CYLINDRICAL_SURFACE('',#16439,4.91825);
#2242=CYLINDRICAL_SURFACE('',#16440,4.91825);
#2243=CYLINDRICAL_SURFACE('',#16441,4.91825);
#2244=CYLINDRICAL_SURFACE('',#16442,4.91825);
#2245=CYLINDRICAL_SURFACE('',#16443,4.91825);
#2246=CYLINDRICAL_SURFACE('',#16444,4.91825);
#2247=CYLINDRICAL_SURFACE('',#16445,4.91825);
#2248=CYLINDRICAL_SURFACE('',#16446,4.91825);
#2249=CYLINDRICAL_SURFACE('',#16447,4.91825);
#2250=CYLINDRICAL_SURFACE('',#16448,4.91825);
#2251=CYLINDRICAL_SURFACE('',#16449,4.91825);
#2252=CYLINDRICAL_SURFACE('',#16450,4.91825);
#2253=CYLINDRICAL_SURFACE('',#16451,4.91825);
#2254=CYLINDRICAL_SURFACE('',#16452,4.91825);
#2255=CYLINDRICAL_SURFACE('',#16453,4.91825);
#2256=CYLINDRICAL_SURFACE('',#16454,4.91825);
#2257=CYLINDRICAL_SURFACE('',#16455,4.91825);
#2258=CYLINDRICAL_SURFACE('',#16456,4.91825);
#2259=CYLINDRICAL_SURFACE('',#16457,4.91825);
#2260=CYLINDRICAL_SURFACE('',#16458,4.91825);
#2261=CYLINDRICAL_SURFACE('',#16459,4.91825);
#2262=CYLINDRICAL_SURFACE('',#16460,4.91825);
#2263=CYLINDRICAL_SURFACE('',#16461,4.91825);
#2264=CYLINDRICAL_SURFACE('',#16462,4.91825);
#2265=CYLINDRICAL_SURFACE('',#16463,4.91825);
#2266=CYLINDRICAL_SURFACE('',#16464,4.91825);
#2267=CYLINDRICAL_SURFACE('',#16465,4.91825);
#2268=CYLINDRICAL_SURFACE('',#16466,4.91825);
#2269=CYLINDRICAL_SURFACE('',#16467,4.91825);
#2270=CYLINDRICAL_SURFACE('',#16468,4.91825);
#2271=CYLINDRICAL_SURFACE('',#16473,5.);
#2272=CYLINDRICAL_SURFACE('',#16479,5.91675);
#2273=CYLINDRICAL_SURFACE('',#16482,4.91825);
#2274=CYLINDRICAL_SURFACE('',#16483,5.91675);
#2275=CYLINDRICAL_SURFACE('',#16484,3.);
#2276=CYLINDRICAL_SURFACE('',#16487,3.);
#2277=CYLINDRICAL_SURFACE('',#16490,3.);
#2278=CYLINDRICAL_SURFACE('',#16493,3.);
#2279=CYLINDRICAL_SURFACE('',#16496,3.);
#2280=CYLINDRICAL_SURFACE('',#16499,3.);
#2281=CYLINDRICAL_SURFACE('',#16505,25.);
#2282=CYLINDRICAL_SURFACE('',#16510,12.);
#2283=CYLINDRICAL_SURFACE('',#16512,6.);
#2284=CYLINDRICAL_SURFACE('',#16515,8.);
#2285=CYLINDRICAL_SURFACE('',#16526,5.);
#2286=CYLINDRICAL_SURFACE('',#16528,11.);
#2287=CYLINDRICAL_SURFACE('',#16532,2.942);
#2288=CYLINDRICAL_SURFACE('',#16534,2.942);
#2289=CYLINDRICAL_SURFACE('',#16535,2.942);
#2290=CYLINDRICAL_SURFACE('',#16536,2.942);
#2291=CYLINDRICAL_SURFACE('',#16537,2.942);
#2292=CYLINDRICAL_SURFACE('',#16538,2.942);
#2293=CYLINDRICAL_SURFACE('',#16539,2.942);
#2294=CYLINDRICAL_SURFACE('',#16540,2.942);
#2295=CYLINDRICAL_SURFACE('',#16541,2.942);
#2296=CYLINDRICAL_SURFACE('',#16542,2.942);
#2297=CYLINDRICAL_SURFACE('',#16543,2.942);
#2298=CYLINDRICAL_SURFACE('',#16544,2.942);
#2299=CYLINDRICAL_SURFACE('',#16545,2.942);
#2300=CYLINDRICAL_SURFACE('',#16546,2.942);
#2301=CYLINDRICAL_SURFACE('',#16547,2.942);
#2302=CYLINDRICAL_SURFACE('',#16548,2.942);
#2303=CYLINDRICAL_SURFACE('',#16549,2.942);
#2304=CYLINDRICAL_SURFACE('',#16550,2.942);
#2305=CYLINDRICAL_SURFACE('',#16551,2.37175);
#2306=CYLINDRICAL_SURFACE('',#16553,2.37175);
#2307=CYLINDRICAL_SURFACE('',#16554,2.37175);
#2308=CYLINDRICAL_SURFACE('',#16555,2.37175);
#2309=CYLINDRICAL_SURFACE('',#16556,2.37175);
#2310=CYLINDRICAL_SURFACE('',#16557,2.37175);
#2311=CYLINDRICAL_SURFACE('',#16558,2.37175);
#2312=CYLINDRICAL_SURFACE('',#16559,2.37175);
#2313=CYLINDRICAL_SURFACE('',#16560,2.37175);
#2314=CYLINDRICAL_SURFACE('',#16561,2.37175);
#2315=CYLINDRICAL_SURFACE('',#16562,2.37175);
#2316=CYLINDRICAL_SURFACE('',#16563,2.37175);
#2317=CYLINDRICAL_SURFACE('',#16564,2.37175);
#2318=CYLINDRICAL_SURFACE('',#16565,2.37175);
#2319=CYLINDRICAL_SURFACE('',#16566,2.37175);
#2320=CYLINDRICAL_SURFACE('',#16567,2.37175);
#2321=CYLINDRICAL_SURFACE('',#16568,2.37175);
#2322=CYLINDRICAL_SURFACE('',#16569,2.37175);
#2323=CYLINDRICAL_SURFACE('',#16577,2.37175);
#2324=CYLINDRICAL_SURFACE('',#16581,2.942);
#2325=CYLINDRICAL_SURFACE('',#16587,4.);
#2326=CYLINDRICAL_SURFACE('',#16589,2.5);
#2327=CYLINDRICAL_SURFACE('',#16594,4.);
#2328=CYLINDRICAL_SURFACE('',#16596,2.5);
#2329=CYLINDRICAL_SURFACE('',#16601,4.);
#2330=CYLINDRICAL_SURFACE('',#16603,2.5);
#2331=CYLINDRICAL_SURFACE('',#16608,4.);
#2332=CYLINDRICAL_SURFACE('',#16610,2.5);
#2333=CYLINDRICAL_SURFACE('',#16612,28.);
#2334=CYLINDRICAL_SURFACE('',#16615,50.);
#2335=CYLINDRICAL_SURFACE('',#16625,27.5);
#2336=CYLINDRICAL_SURFACE('',#16627,20.);
#2337=CYLINDRICAL_SURFACE('',#16630,27.5);
#2338=CYLINDRICAL_SURFACE('',#16639,32.5);
#2339=CYLINDRICAL_SURFACE('',#16641,32.5);
#2340=CYLINDRICAL_SURFACE('',#16643,40.);
#2341=CYLINDRICAL_SURFACE('',#16656,28.);
#2342=CYLINDRICAL_SURFACE('',#16738,32.);
#2343=CYLINDRICAL_SURFACE('',#16744,6.);
#2344=CYLINDRICAL_SURFACE('',#16747,12.);
#2345=CYLINDRICAL_SURFACE('',#16753,1.954);
#2346=CYLINDRICAL_SURFACE('',#16755,1.954);
#2347=CYLINDRICAL_SURFACE('',#16756,1.954);
#2348=CYLINDRICAL_SURFACE('',#16757,1.954);
#2349=CYLINDRICAL_SURFACE('',#16758,1.954);
#2350=CYLINDRICAL_SURFACE('',#16759,1.954);
#2351=CYLINDRICAL_SURFACE('',#16760,1.954);
#2352=CYLINDRICAL_SURFACE('',#16761,1.954);
#2353=CYLINDRICAL_SURFACE('',#16762,1.954);
#2354=CYLINDRICAL_SURFACE('',#16763,1.954);
#2355=CYLINDRICAL_SURFACE('',#16764,1.954);
#2356=CYLINDRICAL_SURFACE('',#16765,1.954);
#2357=CYLINDRICAL_SURFACE('',#16766,1.954);
#2358=CYLINDRICAL_SURFACE('',#16767,1.954);
#2359=CYLINDRICAL_SURFACE('',#16768,1.954);
#2360=CYLINDRICAL_SURFACE('',#16769,1.954);
#2361=CYLINDRICAL_SURFACE('',#16770,1.5555);
#2362=CYLINDRICAL_SURFACE('',#16772,1.5555);
#2363=CYLINDRICAL_SURFACE('',#16773,1.5555);
#2364=CYLINDRICAL_SURFACE('',#16774,1.5555);
#2365=CYLINDRICAL_SURFACE('',#16775,1.5555);
#2366=CYLINDRICAL_SURFACE('',#16776,1.5555);
#2367=CYLINDRICAL_SURFACE('',#16777,1.5555);
#2368=CYLINDRICAL_SURFACE('',#16778,1.5555);
#2369=CYLINDRICAL_SURFACE('',#16779,1.5555);
#2370=CYLINDRICAL_SURFACE('',#16780,1.5555);
#2371=CYLINDRICAL_SURFACE('',#16781,1.5555);
#2372=CYLINDRICAL_SURFACE('',#16782,1.5555);
#2373=CYLINDRICAL_SURFACE('',#16783,1.5555);
#2374=CYLINDRICAL_SURFACE('',#16784,1.5555);
#2375=CYLINDRICAL_SURFACE('',#16785,1.5555);
#2376=CYLINDRICAL_SURFACE('',#16786,1.5555);
#2377=CYLINDRICAL_SURFACE('',#16790,1.5555);
#2378=CYLINDRICAL_SURFACE('',#16792,1.954);
#2379=CYLINDRICAL_SURFACE('',#16802,3.5);
#2380=CIRCLE('',#15699,50.);
#2381=CIRCLE('',#15700,50.);
#2382=CIRCLE('',#15704,50.);
#2383=CIRCLE('',#15705,50.);
#2384=CIRCLE('',#15707,70.);
#2385=CIRCLE('',#15708,12.);
#2386=CIRCLE('',#15710,12.);
#2387=CIRCLE('',#15712,70.);
#2388=CIRCLE('',#15713,70.);
#2389=CIRCLE('',#15714,70.);
#2390=CIRCLE('',#15715,70.);
#2391=CIRCLE('',#15716,70.);
#2392=CIRCLE('',#15718,8.);
#2393=CIRCLE('',#15719,8.);
#2394=CIRCLE('',#15721,8.);
#2395=CIRCLE('',#15722,8.);
#2396=CIRCLE('',#15724,5.5);
#2397=CIRCLE('',#15725,5.5);
#2398=CIRCLE('',#15727,5.5);
#2399=CIRCLE('',#15728,5.5);
#2400=CIRCLE('',#15730,5.5);
#2401=CIRCLE('',#15731,5.5);
#2402=CIRCLE('',#15733,5.5);
#2403=CIRCLE('',#15734,5.5);
#2404=CIRCLE('',#15740,100.);
#2405=CIRCLE('',#15742,100.);
#2406=CIRCLE('',#15743,70.);
#2407=CIRCLE('',#15746,70.);
#2408=CIRCLE('',#15748,50.);
#2409=CIRCLE('',#15749,50.);
#2410=CIRCLE('',#15754,5.13675);
#2411=CIRCLE('',#15756,5.13675);
#2412=CIRCLE('',#15762,5.13675);
#2413=CIRCLE('',#15764,6.11325000000001);
#2414=CIRCLE('',#15771,6.11325000000001);
#2415=CIRCLE('',#15773,1.666);
#2416=CIRCLE('',#15774,1.666);
#2417=CIRCLE('',#15775,1.666);
#2418=CIRCLE('',#15793,1.666);
#2419=CIRCLE('',#15795,2.05475);
#2420=CIRCLE('',#15814,2.05475);
#2421=CIRCLE('',#15816,1.666);
#2422=CIRCLE('',#15817,1.666);
#2423=CIRCLE('',#15818,1.666);
#2424=CIRCLE('',#15836,1.666);
#2425=CIRCLE('',#15838,2.05475);
#2426=CIRCLE('',#15857,2.05475);
#2427=CIRCLE('',#15859,1.666);
#2428=CIRCLE('',#15860,1.666);
#2429=CIRCLE('',#15861,1.666);
#2430=CIRCLE('',#15879,1.666);
#2431=CIRCLE('',#15881,2.05475);
#2432=CIRCLE('',#15900,2.05475);
#2433=CIRCLE('',#15902,1.666);
#2434=CIRCLE('',#15903,1.666);
#2435=CIRCLE('',#15904,1.666);
#2436=CIRCLE('',#15922,1.666);
#2437=CIRCLE('',#15924,2.05475);
#2438=CIRCLE('',#15943,2.05475);
#2439=CIRCLE('',#15945,1.666);
#2440=CIRCLE('',#15946,1.666);
#2441=CIRCLE('',#15947,1.666);
#2442=CIRCLE('',#15965,1.666);
#2443=CIRCLE('',#15967,2.05475);
#2444=CIRCLE('',#15986,2.05475);
#2445=CIRCLE('',#15988,1.666);
#2446=CIRCLE('',#15989,1.666);
#2447=CIRCLE('',#15990,1.666);
#2448=CIRCLE('',#16008,1.666);
#2449=CIRCLE('',#16010,2.05475000000001);
#2450=CIRCLE('',#16029,2.05475000000001);
#2451=CIRCLE('',#16031,1.666);
#2452=CIRCLE('',#16032,1.666);
#2453=CIRCLE('',#16033,1.666);
#2454=CIRCLE('',#16051,1.666);
#2455=CIRCLE('',#16053,2.05475);
#2456=CIRCLE('',#16072,2.05475);
#2457=CIRCLE('',#16074,1.666);
#2458=CIRCLE('',#16075,1.666);
#2459=CIRCLE('',#16076,1.666);
#2460=CIRCLE('',#16094,1.666);
#2461=CIRCLE('',#16096,2.05475000000001);
#2462=CIRCLE('',#16115,2.05475000000001);
#2463=CIRCLE('',#16152,50.);
#2464=CIRCLE('',#16153,40.);
#2465=CIRCLE('',#16156,50.);
#2466=CIRCLE('',#16162,50.);
#2467=CIRCLE('',#16164,40.);
#2468=CIRCLE('',#16165,35.);
#2469=CIRCLE('',#16167,40.);
#2470=CIRCLE('',#16168,35.);
#2471=CIRCLE('',#16171,40.);
#2472=CIRCLE('',#16173,35.);
#2473=CIRCLE('',#16175,40.);
#2474=CIRCLE('',#16176,35.);
#2475=CIRCLE('',#16180,40.);
#2476=CIRCLE('',#16182,50.);
#2477=CIRCLE('',#16186,2.5175);
#2478=CIRCLE('',#16187,2.5175);
#2479=CIRCLE('',#16206,3.0735);
#2480=CIRCLE('',#16207,3.0735);
#2481=CIRCLE('',#16226,19.);
#2482=CIRCLE('',#16227,19.);
#2483=CIRCLE('',#16229,20.);
#2484=CIRCLE('',#16231,20.);
#2485=CIRCLE('',#16233,20.);
#2486=CIRCLE('',#16237,12.);
#2487=CIRCLE('',#16240,12.);
#2488=CIRCLE('',#16241,12.);
#2489=CIRCLE('',#16247,8.);
#2490=CIRCLE('',#16248,8.);
#2491=CIRCLE('',#16251,12.);
#2492=CIRCLE('',#16254,26.);
#2493=CIRCLE('',#16255,20.);
#2494=CIRCLE('',#16257,26.);
#2495=CIRCLE('',#16258,20.);
#2496=CIRCLE('',#16261,20.);
#2497=CIRCLE('',#16263,26.);
#2498=CIRCLE('',#16265,26.);
#2499=CIRCLE('',#16270,20.);
#2500=CIRCLE('',#16271,20.);
#2501=CIRCLE('',#16273,27.);
#2502=CIRCLE('',#16274,27.);
#2503=CIRCLE('',#16279,20.);
#2504=CIRCLE('',#16280,20.);
#2505=CIRCLE('',#16282,27.5);
#2506=CIRCLE('',#16283,27.5);
#2507=CIRCLE('',#16290,27.);
#2508=CIRCLE('',#16291,19.);
#2509=CIRCLE('',#16293,19.);
#2510=CIRCLE('',#16295,27.);
#2511=CIRCLE('',#16306,5.91675);
#2512=CIRCLE('',#16385,5.91675);
#2513=CIRCLE('',#16386,5.91675);
#2514=CIRCLE('',#16387,5.91675);
#2515=CIRCLE('',#16389,4.91825);
#2516=CIRCLE('',#16470,5.);
#2517=CIRCLE('',#16472,4.91825);
#2518=CIRCLE('',#16474,5.);
#2519=CIRCLE('',#16475,5.);
#2520=CIRCLE('',#16478,5.91675);
#2521=CIRCLE('',#16480,5.91675);
#2522=CIRCLE('',#16485,3.);
#2523=CIRCLE('',#16486,3.);
#2524=CIRCLE('',#16488,3.);
#2525=CIRCLE('',#16489,3.);
#2526=CIRCLE('',#16491,3.);
#2527=CIRCLE('',#16492,3.);
#2528=CIRCLE('',#16494,3.);
#2529=CIRCLE('',#16495,3.);
#2530=CIRCLE('',#16497,3.);
#2531=CIRCLE('',#16498,3.);
#2532=CIRCLE('',#16500,3.);
#2533=CIRCLE('',#16501,3.);
#2534=CIRCLE('',#16503,25.);
#2535=CIRCLE('',#16504,12.);
#2536=CIRCLE('',#16506,25.);
#2537=CIRCLE('',#16509,12.);
#2538=CIRCLE('',#16513,6.);
#2539=CIRCLE('',#16514,6.);
#2540=CIRCLE('',#16516,8.);
#2541=CIRCLE('',#16517,8.);
#2542=CIRCLE('',#16524,11.);
#2543=CIRCLE('',#16525,5.);
#2544=CIRCLE('',#16527,5.);
#2545=CIRCLE('',#16529,11.);
#2546=CIRCLE('',#16533,2.942);
#2547=CIRCLE('',#16552,2.37175);
#2548=CIRCLE('',#16578,2.37175);
#2549=CIRCLE('',#16580,2.942);
#2550=CIRCLE('',#16585,4.);
#2551=CIRCLE('',#16586,2.5);
#2552=CIRCLE('',#16588,4.);
#2553=CIRCLE('',#16590,2.5);
#2554=CIRCLE('',#16592,4.);
#2555=CIRCLE('',#16593,2.5);
#2556=CIRCLE('',#16595,4.);
#2557=CIRCLE('',#16597,2.5);
#2558=CIRCLE('',#16599,4.);
#2559=CIRCLE('',#16600,2.5);
#2560=CIRCLE('',#16602,4.);
#2561=CIRCLE('',#16604,2.5);
#2562=CIRCLE('',#16606,4.);
#2563=CIRCLE('',#16607,2.5);
#2564=CIRCLE('',#16609,4.);
#2565=CIRCLE('',#16611,2.5);
#2566=CIRCLE('',#16613,28.);
#2567=CIRCLE('',#16614,28.);
#2568=CIRCLE('',#16616,50.);
#2569=CIRCLE('',#16617,50.);
#2570=CIRCLE('',#16622,27.5);
#2571=CIRCLE('',#16623,6.);
#2572=CIRCLE('',#16624,27.5);
#2573=CIRCLE('',#16626,27.5);
#2574=CIRCLE('',#16628,20.);
#2575=CIRCLE('',#16629,20.);
#2576=CIRCLE('',#16631,27.5);
#2577=CIRCLE('',#16636,32.5);
#2578=CIRCLE('',#16637,6.);
#2579=CIRCLE('',#16638,32.5);
#2580=CIRCLE('',#16640,32.5);
#2581=CIRCLE('',#16642,32.5);
#2582=CIRCLE('',#16644,40.);
#2583=CIRCLE('',#16645,40.);
#2584=CIRCLE('',#16650,5.);
#2585=CIRCLE('',#16653,6.);
#2586=CIRCLE('',#16654,6.);
#2587=CIRCLE('',#16655,6.);
#2588=CIRCLE('',#16657,28.);
#2589=CIRCLE('',#16658,28.);
#2590=CIRCLE('',#16659,28.);
#2591=CIRCLE('',#16660,28.);
#2592=CIRCLE('',#16661,28.);
#2593=CIRCLE('',#16662,28.);
#2594=CIRCLE('',#16663,28.);
#2595=CIRCLE('',#16664,28.);
#2596=CIRCLE('',#16665,28.);
#2597=CIRCLE('',#16666,28.);
#2598=CIRCLE('',#16667,28.);
#2599=CIRCLE('',#16668,28.);
#2600=CIRCLE('',#16669,28.);
#2601=CIRCLE('',#16671,32.);
#2602=CIRCLE('',#16672,6.);
#2603=CIRCLE('',#16674,6.);
#2604=CIRCLE('',#16675,6.);
#2605=CIRCLE('',#16677,32.);
#2606=CIRCLE('',#16678,6.);
#2607=CIRCLE('',#16680,6.);
#2608=CIRCLE('',#16681,6.);
#2609=CIRCLE('',#16682,6.);
#2610=CIRCLE('',#16684,32.);
#2611=CIRCLE('',#16685,6.);
#2612=CIRCLE('',#16687,6.);
#2613=CIRCLE('',#16688,6.);
#2614=CIRCLE('',#16690,32.);
#2615=CIRCLE('',#16691,6.);
#2616=CIRCLE('',#16693,6.);
#2617=CIRCLE('',#16694,6.00000000000001);
#2618=CIRCLE('',#16696,32.);
#2619=CIRCLE('',#16697,6.);
#2620=CIRCLE('',#16699,6.);
#2621=CIRCLE('',#16700,6.);
#2622=CIRCLE('',#16702,32.);
#2623=CIRCLE('',#16703,6.);
#2624=CIRCLE('',#16705,6.);
#2625=CIRCLE('',#16706,6.);
#2626=CIRCLE('',#16708,32.);
#2627=CIRCLE('',#16709,6.);
#2628=CIRCLE('',#16711,6.);
#2629=CIRCLE('',#16712,6.);
#2630=CIRCLE('',#16714,32.);
#2631=CIRCLE('',#16715,6.);
#2632=CIRCLE('',#16716,6.);
#2633=CIRCLE('',#16718,6.);
#2634=CIRCLE('',#16719,6.);
#2635=CIRCLE('',#16721,32.);
#2636=CIRCLE('',#16722,6.);
#2637=CIRCLE('',#16724,6.);
#2638=CIRCLE('',#16725,6.);
#2639=CIRCLE('',#16727,32.);
#2640=CIRCLE('',#16728,6.);
#2641=CIRCLE('',#16730,6.);
#2642=CIRCLE('',#16731,6.);
#2643=CIRCLE('',#16733,32.);
#2644=CIRCLE('',#16734,6.);
#2645=CIRCLE('',#16736,6.);
#2646=CIRCLE('',#16737,6.);
#2647=CIRCLE('',#16739,32.);
#2648=CIRCLE('',#16740,32.);
#2649=CIRCLE('',#16745,6.);
#2650=CIRCLE('',#16746,6.);
#2651=CIRCLE('',#16748,12.);
#2652=CIRCLE('',#16749,12.);
#2653=CIRCLE('',#16754,1.954);
#2654=CIRCLE('',#16771,1.5555);
#2655=CIRCLE('',#16788,1.954);
#2656=CIRCLE('',#16789,1.);
#2657=CIRCLE('',#16791,1.5555);
#2658=CIRCLE('',#16801,3.5);
#2659=CIRCLE('',#16803,3.5);
#2660=FACE_OUTER_BOUND('',#3498,.T.);
#2661=FACE_OUTER_BOUND('',#3499,.T.);
#2662=FACE_OUTER_BOUND('',#3500,.T.);
#2663=FACE_OUTER_BOUND('',#3501,.T.);
#2664=FACE_OUTER_BOUND('',#3502,.T.);
#2665=FACE_OUTER_BOUND('',#3503,.T.);
#2666=FACE_OUTER_BOUND('',#3504,.T.);
#2667=FACE_OUTER_BOUND('',#3505,.T.);
#2668=FACE_OUTER_BOUND('',#3506,.T.);
#2669=FACE_OUTER_BOUND('',#3507,.T.);
#2670=FACE_OUTER_BOUND('',#3508,.T.);
#2671=FACE_OUTER_BOUND('',#3509,.T.);
#2672=FACE_OUTER_BOUND('',#3510,.T.);
#2673=FACE_OUTER_BOUND('',#3511,.T.);
#2674=FACE_OUTER_BOUND('',#3512,.T.);
#2675=FACE_OUTER_BOUND('',#3513,.T.);
#2676=FACE_OUTER_BOUND('',#3514,.T.);
#2677=FACE_OUTER_BOUND('',#3515,.T.);
#2678=FACE_OUTER_BOUND('',#3517,.T.);
#2679=FACE_OUTER_BOUND('',#3524,.T.);
#2680=FACE_OUTER_BOUND('',#3531,.T.);
#2681=FACE_OUTER_BOUND('',#3532,.T.);
#2682=FACE_OUTER_BOUND('',#3533,.T.);
#2683=FACE_OUTER_BOUND('',#3534,.T.);
#2684=FACE_OUTER_BOUND('',#3537,.T.);
#2685=FACE_OUTER_BOUND('',#3539,.T.);
#2686=FACE_OUTER_BOUND('',#3540,.T.);
#2687=FACE_OUTER_BOUND('',#3541,.T.);
#2688=FACE_OUTER_BOUND('',#3542,.T.);
#2689=FACE_OUTER_BOUND('',#3543,.T.);
#2690=FACE_OUTER_BOUND('',#3544,.T.);
#2691=FACE_OUTER_BOUND('',#3545,.T.);
#2692=FACE_OUTER_BOUND('',#3546,.T.);
#2693=FACE_OUTER_BOUND('',#3547,.T.);
#2694=FACE_OUTER_BOUND('',#3548,.T.);
#2695=FACE_OUTER_BOUND('',#3549,.T.);
#2696=FACE_OUTER_BOUND('',#3550,.T.);
#2697=FACE_OUTER_BOUND('',#3551,.T.);
#2698=FACE_OUTER_BOUND('',#3552,.T.);
#2699=FACE_OUTER_BOUND('',#3553,.T.);
#2700=FACE_OUTER_BOUND('',#3554,.T.);
#2701=FACE_OUTER_BOUND('',#3555,.T.);
#2702=FACE_OUTER_BOUND('',#3556,.T.);
#2703=FACE_OUTER_BOUND('',#3557,.T.);
#2704=FACE_OUTER_BOUND('',#3558,.T.);
#2705=FACE_OUTER_BOUND('',#3559,.T.);
#2706=FACE_OUTER_BOUND('',#3560,.T.);
#2707=FACE_OUTER_BOUND('',#3561,.T.);
#2708=FACE_OUTER_BOUND('',#3562,.T.);
#2709=FACE_OUTER_BOUND('',#3563,.T.);
#2710=FACE_OUTER_BOUND('',#3564,.T.);
#2711=FACE_OUTER_BOUND('',#3565,.T.);
#2712=FACE_OUTER_BOUND('',#3566,.T.);
#2713=FACE_OUTER_BOUND('',#3567,.T.);
#2714=FACE_OUTER_BOUND('',#3568,.T.);
#2715=FACE_OUTER_BOUND('',#3569,.T.);
#2716=FACE_OUTER_BOUND('',#3570,.T.);
#2717=FACE_OUTER_BOUND('',#3571,.T.);
#2718=FACE_OUTER_BOUND('',#3572,.T.);
#2719=FACE_OUTER_BOUND('',#3573,.T.);
#2720=FACE_OUTER_BOUND('',#3574,.T.);
#2721=FACE_OUTER_BOUND('',#3575,.T.);
#2722=FACE_OUTER_BOUND('',#3576,.T.);
#2723=FACE_OUTER_BOUND('',#3577,.T.);
#2724=FACE_OUTER_BOUND('',#3578,.T.);
#2725=FACE_OUTER_BOUND('',#3579,.T.);
#2726=FACE_OUTER_BOUND('',#3580,.T.);
#2727=FACE_OUTER_BOUND('',#3581,.T.);
#2728=FACE_OUTER_BOUND('',#3582,.T.);
#2729=FACE_OUTER_BOUND('',#3583,.T.);
#2730=FACE_OUTER_BOUND('',#3584,.T.);
#2731=FACE_OUTER_BOUND('',#3585,.T.);
#2732=FACE_OUTER_BOUND('',#3586,.T.);
#2733=FACE_OUTER_BOUND('',#3587,.T.);
#2734=FACE_OUTER_BOUND('',#3588,.T.);
#2735=FACE_OUTER_BOUND('',#3589,.T.);
#2736=FACE_OUTER_BOUND('',#3590,.T.);
#2737=FACE_OUTER_BOUND('',#3591,.T.);
#2738=FACE_OUTER_BOUND('',#3592,.T.);
#2739=FACE_OUTER_BOUND('',#3593,.T.);
#2740=FACE_OUTER_BOUND('',#3594,.T.);
#2741=FACE_OUTER_BOUND('',#3595,.T.);
#2742=FACE_OUTER_BOUND('',#3596,.T.);
#2743=FACE_OUTER_BOUND('',#3597,.T.);
#2744=FACE_OUTER_BOUND('',#3598,.T.);
#2745=FACE_OUTER_BOUND('',#3599,.T.);
#2746=FACE_OUTER_BOUND('',#3600,.T.);
#2747=FACE_OUTER_BOUND('',#3601,.T.);
#2748=FACE_OUTER_BOUND('',#3602,.T.);
#2749=FACE_OUTER_BOUND('',#3603,.T.);
#2750=FACE_OUTER_BOUND('',#3604,.T.);
#2751=FACE_OUTER_BOUND('',#3605,.T.);
#2752=FACE_OUTER_BOUND('',#3606,.T.);
#2753=FACE_OUTER_BOUND('',#3607,.T.);
#2754=FACE_OUTER_BOUND('',#3608,.T.);
#2755=FACE_OUTER_BOUND('',#3609,.T.);
#2756=FACE_OUTER_BOUND('',#3610,.T.);
#2757=FACE_OUTER_BOUND('',#3611,.T.);
#2758=FACE_OUTER_BOUND('',#3612,.T.);
#2759=FACE_OUTER_BOUND('',#3613,.T.);
#2760=FACE_OUTER_BOUND('',#3614,.T.);
#2761=FACE_OUTER_BOUND('',#3615,.T.);
#2762=FACE_OUTER_BOUND('',#3616,.T.);
#2763=FACE_OUTER_BOUND('',#3617,.T.);
#2764=FACE_OUTER_BOUND('',#3618,.T.);
#2765=FACE_OUTER_BOUND('',#3619,.T.);
#2766=FACE_OUTER_BOUND('',#3620,.T.);
#2767=FACE_OUTER_BOUND('',#3621,.T.);
#2768=FACE_OUTER_BOUND('',#3622,.T.);
#2769=FACE_OUTER_BOUND('',#3623,.T.);
#2770=FACE_OUTER_BOUND('',#3624,.T.);
#2771=FACE_OUTER_BOUND('',#3625,.T.);
#2772=FACE_OUTER_BOUND('',#3626,.T.);
#2773=FACE_OUTER_BOUND('',#3627,.T.);
#2774=FACE_OUTER_BOUND('',#3628,.T.);
#2775=FACE_OUTER_BOUND('',#3629,.T.);
#2776=FACE_OUTER_BOUND('',#3630,.T.);
#2777=FACE_OUTER_BOUND('',#3631,.T.);
#2778=FACE_OUTER_BOUND('',#3632,.T.);
#2779=FACE_OUTER_BOUND('',#3633,.T.);
#2780=FACE_OUTER_BOUND('',#3634,.T.);
#2781=FACE_OUTER_BOUND('',#3635,.T.);
#2782=FACE_OUTER_BOUND('',#3636,.T.);
#2783=FACE_OUTER_BOUND('',#3637,.T.);
#2784=FACE_OUTER_BOUND('',#3638,.T.);
#2785=FACE_OUTER_BOUND('',#3639,.T.);
#2786=FACE_OUTER_BOUND('',#3640,.T.);
#2787=FACE_OUTER_BOUND('',#3641,.T.);
#2788=FACE_OUTER_BOUND('',#3642,.T.);
#2789=FACE_OUTER_BOUND('',#3643,.T.);
#2790=FACE_OUTER_BOUND('',#3644,.T.);
#2791=FACE_OUTER_BOUND('',#3645,.T.);
#2792=FACE_OUTER_BOUND('',#3646,.T.);
#2793=FACE_OUTER_BOUND('',#3647,.T.);
#2794=FACE_OUTER_BOUND('',#3648,.T.);
#2795=FACE_OUTER_BOUND('',#3649,.T.);
#2796=FACE_OUTER_BOUND('',#3650,.T.);
#2797=FACE_OUTER_BOUND('',#3651,.T.);
#2798=FACE_OUTER_BOUND('',#3652,.T.);
#2799=FACE_OUTER_BOUND('',#3653,.T.);
#2800=FACE_OUTER_BOUND('',#3654,.T.);
#2801=FACE_OUTER_BOUND('',#3655,.T.);
#2802=FACE_OUTER_BOUND('',#3656,.T.);
#2803=FACE_OUTER_BOUND('',#3657,.T.);
#2804=FACE_OUTER_BOUND('',#3658,.T.);
#2805=FACE_OUTER_BOUND('',#3659,.T.);
#2806=FACE_OUTER_BOUND('',#3660,.T.);
#2807=FACE_OUTER_BOUND('',#3661,.T.);
#2808=FACE_OUTER_BOUND('',#3662,.T.);
#2809=FACE_OUTER_BOUND('',#3663,.T.);
#2810=FACE_OUTER_BOUND('',#3664,.T.);
#2811=FACE_OUTER_BOUND('',#3665,.T.);
#2812=FACE_OUTER_BOUND('',#3666,.T.);
#2813=FACE_OUTER_BOUND('',#3667,.T.);
#2814=FACE_OUTER_BOUND('',#3668,.T.);
#2815=FACE_OUTER_BOUND('',#3669,.T.);
#2816=FACE_OUTER_BOUND('',#3670,.T.);
#2817=FACE_OUTER_BOUND('',#3671,.T.);
#2818=FACE_OUTER_BOUND('',#3672,.T.);
#2819=FACE_OUTER_BOUND('',#3673,.T.);
#2820=FACE_OUTER_BOUND('',#3674,.T.);
#2821=FACE_OUTER_BOUND('',#3675,.T.);
#2822=FACE_OUTER_BOUND('',#3676,.T.);
#2823=FACE_OUTER_BOUND('',#3677,.T.);
#2824=FACE_OUTER_BOUND('',#3678,.T.);
#2825=FACE_OUTER_BOUND('',#3679,.T.);
#2826=FACE_OUTER_BOUND('',#3680,.T.);
#2827=FACE_OUTER_BOUND('',#3681,.T.);
#2828=FACE_OUTER_BOUND('',#3682,.T.);
#2829=FACE_OUTER_BOUND('',#3683,.T.);
#2830=FACE_OUTER_BOUND('',#3684,.T.);
#2831=FACE_OUTER_BOUND('',#3685,.T.);
#2832=FACE_OUTER_BOUND('',#3686,.T.);
#2833=FACE_OUTER_BOUND('',#3687,.T.);
#2834=FACE_OUTER_BOUND('',#3688,.T.);
#2835=FACE_OUTER_BOUND('',#3689,.T.);
#2836=FACE_OUTER_BOUND('',#3690,.T.);
#2837=FACE_OUTER_BOUND('',#3691,.T.);
#2838=FACE_OUTER_BOUND('',#3692,.T.);
#2839=FACE_OUTER_BOUND('',#3693,.T.);
#2840=FACE_OUTER_BOUND('',#3694,.T.);
#2841=FACE_OUTER_BOUND('',#3695,.T.);
#2842=FACE_OUTER_BOUND('',#3696,.T.);
#2843=FACE_OUTER_BOUND('',#3697,.T.);
#2844=FACE_OUTER_BOUND('',#3698,.T.);
#2845=FACE_OUTER_BOUND('',#3699,.T.);
#2846=FACE_OUTER_BOUND('',#3700,.T.);
#2847=FACE_OUTER_BOUND('',#3701,.T.);
#2848=FACE_OUTER_BOUND('',#3702,.T.);
#2849=FACE_OUTER_BOUND('',#3703,.T.);
#2850=FACE_OUTER_BOUND('',#3704,.T.);
#2851=FACE_OUTER_BOUND('',#3705,.T.);
#2852=FACE_OUTER_BOUND('',#3706,.T.);
#2853=FACE_OUTER_BOUND('',#3707,.T.);
#2854=FACE_OUTER_BOUND('',#3708,.T.);
#2855=FACE_OUTER_BOUND('',#3709,.T.);
#2856=FACE_OUTER_BOUND('',#3710,.T.);
#2857=FACE_OUTER_BOUND('',#3711,.T.);
#2858=FACE_OUTER_BOUND('',#3712,.T.);
#2859=FACE_OUTER_BOUND('',#3713,.T.);
#2860=FACE_OUTER_BOUND('',#3714,.T.);
#2861=FACE_OUTER_BOUND('',#3715,.T.);
#2862=FACE_OUTER_BOUND('',#3716,.T.);
#2863=FACE_OUTER_BOUND('',#3717,.T.);
#2864=FACE_OUTER_BOUND('',#3718,.T.);
#2865=FACE_OUTER_BOUND('',#3719,.T.);
#2866=FACE_OUTER_BOUND('',#3720,.T.);
#2867=FACE_OUTER_BOUND('',#3721,.T.);
#2868=FACE_OUTER_BOUND('',#3722,.T.);
#2869=FACE_OUTER_BOUND('',#3723,.T.);
#2870=FACE_OUTER_BOUND('',#3724,.T.);
#2871=FACE_OUTER_BOUND('',#3725,.T.);
#2872=FACE_OUTER_BOUND('',#3726,.T.);
#2873=FACE_OUTER_BOUND('',#3727,.T.);
#2874=FACE_OUTER_BOUND('',#3728,.T.);
#2875=FACE_OUTER_BOUND('',#3729,.T.);
#2876=FACE_OUTER_BOUND('',#3730,.T.);
#2877=FACE_OUTER_BOUND('',#3731,.T.);
#2878=FACE_OUTER_BOUND('',#3732,.T.);
#2879=FACE_OUTER_BOUND('',#3733,.T.);
#2880=FACE_OUTER_BOUND('',#3734,.T.);
#2881=FACE_OUTER_BOUND('',#3735,.T.);
#2882=FACE_OUTER_BOUND('',#3736,.T.);
#2883=FACE_OUTER_BOUND('',#3737,.T.);
#2884=FACE_OUTER_BOUND('',#3738,.T.);
#2885=FACE_OUTER_BOUND('',#3739,.T.);
#2886=FACE_OUTER_BOUND('',#3740,.T.);
#2887=FACE_OUTER_BOUND('',#3741,.T.);
#2888=FACE_OUTER_BOUND('',#3742,.T.);
#2889=FACE_OUTER_BOUND('',#3743,.T.);
#2890=FACE_OUTER_BOUND('',#3744,.T.);
#2891=FACE_OUTER_BOUND('',#3745,.T.);
#2892=FACE_OUTER_BOUND('',#3746,.T.);
#2893=FACE_OUTER_BOUND('',#3747,.T.);
#2894=FACE_OUTER_BOUND('',#3748,.T.);
#2895=FACE_OUTER_BOUND('',#3749,.T.);
#2896=FACE_OUTER_BOUND('',#3750,.T.);
#2897=FACE_OUTER_BOUND('',#3751,.T.);
#2898=FACE_OUTER_BOUND('',#3752,.T.);
#2899=FACE_OUTER_BOUND('',#3753,.T.);
#2900=FACE_OUTER_BOUND('',#3754,.T.);
#2901=FACE_OUTER_BOUND('',#3755,.T.);
#2902=FACE_OUTER_BOUND('',#3756,.T.);
#2903=FACE_OUTER_BOUND('',#3757,.T.);
#2904=FACE_OUTER_BOUND('',#3758,.T.);
#2905=FACE_OUTER_BOUND('',#3759,.T.);
#2906=FACE_OUTER_BOUND('',#3760,.T.);
#2907=FACE_OUTER_BOUND('',#3761,.T.);
#2908=FACE_OUTER_BOUND('',#3762,.T.);
#2909=FACE_OUTER_BOUND('',#3763,.T.);
#2910=FACE_OUTER_BOUND('',#3764,.T.);
#2911=FACE_OUTER_BOUND('',#3765,.T.);
#2912=FACE_OUTER_BOUND('',#3766,.T.);
#2913=FACE_OUTER_BOUND('',#3767,.T.);
#2914=FACE_OUTER_BOUND('',#3768,.T.);
#2915=FACE_OUTER_BOUND('',#3769,.T.);
#2916=FACE_OUTER_BOUND('',#3770,.T.);
#2917=FACE_OUTER_BOUND('',#3771,.T.);
#2918=FACE_OUTER_BOUND('',#3772,.T.);
#2919=FACE_OUTER_BOUND('',#3773,.T.);
#2920=FACE_OUTER_BOUND('',#3774,.T.);
#2921=FACE_OUTER_BOUND('',#3775,.T.);
#2922=FACE_OUTER_BOUND('',#3776,.T.);
#2923=FACE_OUTER_BOUND('',#3777,.T.);
#2924=FACE_OUTER_BOUND('',#3778,.T.);
#2925=FACE_OUTER_BOUND('',#3779,.T.);
#2926=FACE_OUTER_BOUND('',#3780,.T.);
#2927=FACE_OUTER_BOUND('',#3781,.T.);
#2928=FACE_OUTER_BOUND('',#3782,.T.);
#2929=FACE_OUTER_BOUND('',#3783,.T.);
#2930=FACE_OUTER_BOUND('',#3784,.T.);
#2931=FACE_OUTER_BOUND('',#3785,.T.);
#2932=FACE_OUTER_BOUND('',#3786,.T.);
#2933=FACE_OUTER_BOUND('',#3787,.T.);
#2934=FACE_OUTER_BOUND('',#3788,.T.);
#2935=FACE_OUTER_BOUND('',#3789,.T.);
#2936=FACE_OUTER_BOUND('',#3790,.T.);
#2937=FACE_OUTER_BOUND('',#3791,.T.);
#2938=FACE_OUTER_BOUND('',#3792,.T.);
#2939=FACE_OUTER_BOUND('',#3793,.T.);
#2940=FACE_OUTER_BOUND('',#3794,.T.);
#2941=FACE_OUTER_BOUND('',#3795,.T.);
#2942=FACE_OUTER_BOUND('',#3796,.T.);
#2943=FACE_OUTER_BOUND('',#3797,.T.);
#2944=FACE_OUTER_BOUND('',#3798,.T.);
#2945=FACE_OUTER_BOUND('',#3799,.T.);
#2946=FACE_OUTER_BOUND('',#3800,.T.);
#2947=FACE_OUTER_BOUND('',#3801,.T.);
#2948=FACE_OUTER_BOUND('',#3802,.T.);
#2949=FACE_OUTER_BOUND('',#3803,.T.);
#2950=FACE_OUTER_BOUND('',#3804,.T.);
#2951=FACE_OUTER_BOUND('',#3805,.T.);
#2952=FACE_OUTER_BOUND('',#3806,.T.);
#2953=FACE_OUTER_BOUND('',#3807,.T.);
#2954=FACE_OUTER_BOUND('',#3808,.T.);
#2955=FACE_OUTER_BOUND('',#3809,.T.);
#2956=FACE_OUTER_BOUND('',#3810,.T.);
#2957=FACE_OUTER_BOUND('',#3811,.T.);
#2958=FACE_OUTER_BOUND('',#3812,.T.);
#2959=FACE_OUTER_BOUND('',#3813,.T.);
#2960=FACE_OUTER_BOUND('',#3814,.T.);
#2961=FACE_OUTER_BOUND('',#3815,.T.);
#2962=FACE_OUTER_BOUND('',#3816,.T.);
#2963=FACE_OUTER_BOUND('',#3817,.T.);
#2964=FACE_OUTER_BOUND('',#3818,.T.);
#2965=FACE_OUTER_BOUND('',#3819,.T.);
#2966=FACE_OUTER_BOUND('',#3820,.T.);
#2967=FACE_OUTER_BOUND('',#3821,.T.);
#2968=FACE_OUTER_BOUND('',#3822,.T.);
#2969=FACE_OUTER_BOUND('',#3823,.T.);
#2970=FACE_OUTER_BOUND('',#3824,.T.);
#2971=FACE_OUTER_BOUND('',#3825,.T.);
#2972=FACE_OUTER_BOUND('',#3826,.T.);
#2973=FACE_OUTER_BOUND('',#3827,.T.);
#2974=FACE_OUTER_BOUND('',#3828,.T.);
#2975=FACE_OUTER_BOUND('',#3829,.T.);
#2976=FACE_OUTER_BOUND('',#3830,.T.);
#2977=FACE_OUTER_BOUND('',#3831,.T.);
#2978=FACE_OUTER_BOUND('',#3832,.T.);
#2979=FACE_OUTER_BOUND('',#3833,.T.);
#2980=FACE_OUTER_BOUND('',#3834,.T.);
#2981=FACE_OUTER_BOUND('',#3835,.T.);
#2982=FACE_OUTER_BOUND('',#3836,.T.);
#2983=FACE_OUTER_BOUND('',#3837,.T.);
#2984=FACE_OUTER_BOUND('',#3838,.T.);
#2985=FACE_OUTER_BOUND('',#3839,.T.);
#2986=FACE_OUTER_BOUND('',#3840,.T.);
#2987=FACE_OUTER_BOUND('',#3841,.T.);
#2988=FACE_OUTER_BOUND('',#3842,.T.);
#2989=FACE_OUTER_BOUND('',#3843,.T.);
#2990=FACE_OUTER_BOUND('',#3844,.T.);
#2991=FACE_OUTER_BOUND('',#3845,.T.);
#2992=FACE_OUTER_BOUND('',#3846,.T.);
#2993=FACE_OUTER_BOUND('',#3847,.T.);
#2994=FACE_OUTER_BOUND('',#3848,.T.);
#2995=FACE_OUTER_BOUND('',#3849,.T.);
#2996=FACE_OUTER_BOUND('',#3850,.T.);
#2997=FACE_OUTER_BOUND('',#3851,.T.);
#2998=FACE_OUTER_BOUND('',#3852,.T.);
#2999=FACE_OUTER_BOUND('',#3853,.T.);
#3000=FACE_OUTER_BOUND('',#3854,.T.);
#3001=FACE_OUTER_BOUND('',#3855,.T.);
#3002=FACE_OUTER_BOUND('',#3856,.T.);
#3003=FACE_OUTER_BOUND('',#3857,.T.);
#3004=FACE_OUTER_BOUND('',#3858,.T.);
#3005=FACE_OUTER_BOUND('',#3859,.T.);
#3006=FACE_OUTER_BOUND('',#3860,.T.);
#3007=FACE_OUTER_BOUND('',#3861,.T.);
#3008=FACE_OUTER_BOUND('',#3862,.T.);
#3009=FACE_OUTER_BOUND('',#3863,.T.);
#3010=FACE_OUTER_BOUND('',#3864,.T.);
#3011=FACE_OUTER_BOUND('',#3865,.T.);
#3012=FACE_OUTER_BOUND('',#3866,.T.);
#3013=FACE_OUTER_BOUND('',#3867,.T.);
#3014=FACE_OUTER_BOUND('',#3868,.T.);
#3015=FACE_OUTER_BOUND('',#3869,.T.);
#3016=FACE_OUTER_BOUND('',#3870,.T.);
#3017=FACE_OUTER_BOUND('',#3871,.T.);
#3018=FACE_OUTER_BOUND('',#3872,.T.);
#3019=FACE_OUTER_BOUND('',#3873,.T.);
#3020=FACE_OUTER_BOUND('',#3874,.T.);
#3021=FACE_OUTER_BOUND('',#3875,.T.);
#3022=FACE_OUTER_BOUND('',#3876,.T.);
#3023=FACE_OUTER_BOUND('',#3877,.T.);
#3024=FACE_OUTER_BOUND('',#3878,.T.);
#3025=FACE_OUTER_BOUND('',#3879,.T.);
#3026=FACE_OUTER_BOUND('',#3880,.T.);
#3027=FACE_OUTER_BOUND('',#3881,.T.);
#3028=FACE_OUTER_BOUND('',#3882,.T.);
#3029=FACE_OUTER_BOUND('',#3883,.T.);
#3030=FACE_OUTER_BOUND('',#3884,.T.);
#3031=FACE_OUTER_BOUND('',#3885,.T.);
#3032=FACE_OUTER_BOUND('',#3886,.T.);
#3033=FACE_OUTER_BOUND('',#3887,.T.);
#3034=FACE_OUTER_BOUND('',#3888,.T.);
#3035=FACE_OUTER_BOUND('',#3889,.T.);
#3036=FACE_OUTER_BOUND('',#3890,.T.);
#3037=FACE_OUTER_BOUND('',#3891,.T.);
#3038=FACE_OUTER_BOUND('',#3892,.T.);
#3039=FACE_OUTER_BOUND('',#3893,.T.);
#3040=FACE_OUTER_BOUND('',#3894,.T.);
#3041=FACE_OUTER_BOUND('',#3895,.T.);
#3042=FACE_OUTER_BOUND('',#3896,.T.);
#3043=FACE_OUTER_BOUND('',#3897,.T.);
#3044=FACE_OUTER_BOUND('',#3898,.T.);
#3045=FACE_OUTER_BOUND('',#3899,.T.);
#3046=FACE_OUTER_BOUND('',#3900,.T.);
#3047=FACE_OUTER_BOUND('',#3906,.T.);
#3048=FACE_OUTER_BOUND('',#3907,.T.);
#3049=FACE_OUTER_BOUND('',#3908,.T.);
#3050=FACE_OUTER_BOUND('',#3909,.T.);
#3051=FACE_OUTER_BOUND('',#3911,.T.);
#3052=FACE_OUTER_BOUND('',#3912,.T.);
#3053=FACE_OUTER_BOUND('',#3913,.T.);
#3054=FACE_OUTER_BOUND('',#3914,.T.);
#3055=FACE_OUTER_BOUND('',#3915,.T.);
#3056=FACE_OUTER_BOUND('',#3917,.T.);
#3057=FACE_OUTER_BOUND('',#3919,.T.);
#3058=FACE_OUTER_BOUND('',#3921,.T.);
#3059=FACE_OUTER_BOUND('',#3922,.T.);
#3060=FACE_OUTER_BOUND('',#3923,.T.);
#3061=FACE_OUTER_BOUND('',#3925,.T.);
#3062=FACE_OUTER_BOUND('',#3927,.T.);
#3063=FACE_OUTER_BOUND('',#3928,.T.);
#3064=FACE_OUTER_BOUND('',#3929,.T.);
#3065=FACE_OUTER_BOUND('',#3930,.T.);
#3066=FACE_OUTER_BOUND('',#3932,.T.);
#3067=FACE_OUTER_BOUND('',#3938,.T.);
#3068=FACE_OUTER_BOUND('',#3939,.T.);
#3069=FACE_OUTER_BOUND('',#3940,.T.);
#3070=FACE_OUTER_BOUND('',#3941,.T.);
#3071=FACE_OUTER_BOUND('',#3942,.T.);
#3072=FACE_OUTER_BOUND('',#3943,.T.);
#3073=FACE_OUTER_BOUND('',#3944,.T.);
#3074=FACE_OUTER_BOUND('',#3945,.T.);
#3075=FACE_OUTER_BOUND('',#3946,.T.);
#3076=FACE_OUTER_BOUND('',#3947,.T.);
#3077=FACE_OUTER_BOUND('',#3948,.T.);
#3078=FACE_OUTER_BOUND('',#3949,.T.);
#3079=FACE_OUTER_BOUND('',#3950,.T.);
#3080=FACE_OUTER_BOUND('',#3951,.T.);
#3081=FACE_OUTER_BOUND('',#3952,.T.);
#3082=FACE_OUTER_BOUND('',#3953,.T.);
#3083=FACE_OUTER_BOUND('',#3954,.T.);
#3084=FACE_OUTER_BOUND('',#3955,.T.);
#3085=FACE_OUTER_BOUND('',#3956,.T.);
#3086=FACE_OUTER_BOUND('',#3957,.T.);
#3087=FACE_OUTER_BOUND('',#3958,.T.);
#3088=FACE_OUTER_BOUND('',#3959,.T.);
#3089=FACE_OUTER_BOUND('',#3960,.T.);
#3090=FACE_OUTER_BOUND('',#3961,.T.);
#3091=FACE_OUTER_BOUND('',#3962,.T.);
#3092=FACE_OUTER_BOUND('',#3963,.T.);
#3093=FACE_OUTER_BOUND('',#3964,.T.);
#3094=FACE_OUTER_BOUND('',#3965,.T.);
#3095=FACE_OUTER_BOUND('',#3966,.T.);
#3096=FACE_OUTER_BOUND('',#3967,.T.);
#3097=FACE_OUTER_BOUND('',#3968,.T.);
#3098=FACE_OUTER_BOUND('',#3969,.T.);
#3099=FACE_OUTER_BOUND('',#3970,.T.);
#3100=FACE_OUTER_BOUND('',#3971,.T.);
#3101=FACE_OUTER_BOUND('',#3972,.T.);
#3102=FACE_OUTER_BOUND('',#3973,.T.);
#3103=FACE_OUTER_BOUND('',#3974,.T.);
#3104=FACE_OUTER_BOUND('',#3975,.T.);
#3105=FACE_OUTER_BOUND('',#3977,.T.);
#3106=FACE_OUTER_BOUND('',#3979,.T.);
#3107=FACE_OUTER_BOUND('',#3980,.T.);
#3108=FACE_OUTER_BOUND('',#3981,.T.);
#3109=FACE_OUTER_BOUND('',#3982,.T.);
#3110=FACE_OUTER_BOUND('',#3983,.T.);
#3111=FACE_OUTER_BOUND('',#3984,.T.);
#3112=FACE_OUTER_BOUND('',#3986,.T.);
#3113=FACE_OUTER_BOUND('',#3987,.T.);
#3114=FACE_OUTER_BOUND('',#3988,.T.);
#3115=FACE_OUTER_BOUND('',#3989,.T.);
#3116=FACE_OUTER_BOUND('',#3990,.T.);
#3117=FACE_OUTER_BOUND('',#3991,.T.);
#3118=FACE_OUTER_BOUND('',#3992,.T.);
#3119=FACE_OUTER_BOUND('',#3993,.T.);
#3120=FACE_OUTER_BOUND('',#3994,.T.);
#3121=FACE_OUTER_BOUND('',#3995,.T.);
#3122=FACE_OUTER_BOUND('',#3996,.T.);
#3123=FACE_OUTER_BOUND('',#3998,.T.);
#3124=FACE_OUTER_BOUND('',#4000,.T.);
#3125=FACE_OUTER_BOUND('',#4001,.T.);
#3126=FACE_OUTER_BOUND('',#4002,.T.);
#3127=FACE_OUTER_BOUND('',#4004,.T.);
#3128=FACE_OUTER_BOUND('',#4006,.T.);
#3129=FACE_OUTER_BOUND('',#4008,.T.);
#3130=FACE_OUTER_BOUND('',#4009,.T.);
#3131=FACE_OUTER_BOUND('',#4010,.T.);
#3132=FACE_OUTER_BOUND('',#4011,.T.);
#3133=FACE_OUTER_BOUND('',#4013,.T.);
#3134=FACE_OUTER_BOUND('',#4015,.T.);
#3135=FACE_OUTER_BOUND('',#4016,.T.);
#3136=FACE_OUTER_BOUND('',#4017,.T.);
#3137=FACE_OUTER_BOUND('',#4019,.T.);
#3138=FACE_OUTER_BOUND('',#4021,.T.);
#3139=FACE_OUTER_BOUND('',#4022,.T.);
#3140=FACE_OUTER_BOUND('',#4023,.T.);
#3141=FACE_OUTER_BOUND('',#4024,.T.);
#3142=FACE_OUTER_BOUND('',#4025,.T.);
#3143=FACE_OUTER_BOUND('',#4026,.T.);
#3144=FACE_OUTER_BOUND('',#4027,.T.);
#3145=FACE_OUTER_BOUND('',#4028,.T.);
#3146=FACE_OUTER_BOUND('',#4029,.T.);
#3147=FACE_OUTER_BOUND('',#4030,.T.);
#3148=FACE_OUTER_BOUND('',#4031,.T.);
#3149=FACE_OUTER_BOUND('',#4032,.T.);
#3150=FACE_OUTER_BOUND('',#4033,.T.);
#3151=FACE_OUTER_BOUND('',#4034,.T.);
#3152=FACE_OUTER_BOUND('',#4035,.T.);
#3153=FACE_OUTER_BOUND('',#4036,.T.);
#3154=FACE_OUTER_BOUND('',#4037,.T.);
#3155=FACE_OUTER_BOUND('',#4038,.T.);
#3156=FACE_OUTER_BOUND('',#4039,.T.);
#3157=FACE_OUTER_BOUND('',#4040,.T.);
#3158=FACE_OUTER_BOUND('',#4041,.T.);
#3159=FACE_OUTER_BOUND('',#4042,.T.);
#3160=FACE_OUTER_BOUND('',#4043,.T.);
#3161=FACE_OUTER_BOUND('',#4044,.T.);
#3162=FACE_OUTER_BOUND('',#4045,.T.);
#3163=FACE_OUTER_BOUND('',#4046,.T.);
#3164=FACE_OUTER_BOUND('',#4047,.T.);
#3165=FACE_OUTER_BOUND('',#4048,.T.);
#3166=FACE_OUTER_BOUND('',#4049,.T.);
#3167=FACE_OUTER_BOUND('',#4050,.T.);
#3168=FACE_OUTER_BOUND('',#4051,.T.);
#3169=FACE_OUTER_BOUND('',#4052,.T.);
#3170=FACE_OUTER_BOUND('',#4053,.T.);
#3171=FACE_OUTER_BOUND('',#4054,.T.);
#3172=FACE_OUTER_BOUND('',#4055,.T.);
#3173=FACE_OUTER_BOUND('',#4056,.T.);
#3174=FACE_OUTER_BOUND('',#4057,.T.);
#3175=FACE_OUTER_BOUND('',#4058,.T.);
#3176=FACE_OUTER_BOUND('',#4059,.T.);
#3177=FACE_OUTER_BOUND('',#4060,.T.);
#3178=FACE_OUTER_BOUND('',#4061,.T.);
#3179=FACE_OUTER_BOUND('',#4062,.T.);
#3180=FACE_OUTER_BOUND('',#4063,.T.);
#3181=FACE_OUTER_BOUND('',#4064,.T.);
#3182=FACE_OUTER_BOUND('',#4065,.T.);
#3183=FACE_OUTER_BOUND('',#4066,.T.);
#3184=FACE_OUTER_BOUND('',#4067,.T.);
#3185=FACE_OUTER_BOUND('',#4068,.T.);
#3186=FACE_OUTER_BOUND('',#4069,.T.);
#3187=FACE_OUTER_BOUND('',#4070,.T.);
#3188=FACE_OUTER_BOUND('',#4071,.T.);
#3189=FACE_OUTER_BOUND('',#4072,.T.);
#3190=FACE_OUTER_BOUND('',#4073,.T.);
#3191=FACE_OUTER_BOUND('',#4074,.T.);
#3192=FACE_OUTER_BOUND('',#4075,.T.);
#3193=FACE_OUTER_BOUND('',#4076,.T.);
#3194=FACE_OUTER_BOUND('',#4077,.T.);
#3195=FACE_OUTER_BOUND('',#4078,.T.);
#3196=FACE_OUTER_BOUND('',#4079,.T.);
#3197=FACE_OUTER_BOUND('',#4080,.T.);
#3198=FACE_OUTER_BOUND('',#4081,.T.);
#3199=FACE_OUTER_BOUND('',#4082,.T.);
#3200=FACE_OUTER_BOUND('',#4083,.T.);
#3201=FACE_OUTER_BOUND('',#4084,.T.);
#3202=FACE_OUTER_BOUND('',#4085,.T.);
#3203=FACE_OUTER_BOUND('',#4086,.T.);
#3204=FACE_OUTER_BOUND('',#4087,.T.);
#3205=FACE_OUTER_BOUND('',#4088,.T.);
#3206=FACE_OUTER_BOUND('',#4089,.T.);
#3207=FACE_OUTER_BOUND('',#4090,.T.);
#3208=FACE_OUTER_BOUND('',#4091,.T.);
#3209=FACE_OUTER_BOUND('',#4092,.T.);
#3210=FACE_OUTER_BOUND('',#4093,.T.);
#3211=FACE_OUTER_BOUND('',#4094,.T.);
#3212=FACE_OUTER_BOUND('',#4095,.T.);
#3213=FACE_OUTER_BOUND('',#4096,.T.);
#3214=FACE_OUTER_BOUND('',#4097,.T.);
#3215=FACE_OUTER_BOUND('',#4098,.T.);
#3216=FACE_OUTER_BOUND('',#4099,.T.);
#3217=FACE_OUTER_BOUND('',#4100,.T.);
#3218=FACE_OUTER_BOUND('',#4101,.T.);
#3219=FACE_OUTER_BOUND('',#4102,.T.);
#3220=FACE_OUTER_BOUND('',#4103,.T.);
#3221=FACE_OUTER_BOUND('',#4104,.T.);
#3222=FACE_OUTER_BOUND('',#4105,.T.);
#3223=FACE_OUTER_BOUND('',#4106,.T.);
#3224=FACE_OUTER_BOUND('',#4107,.T.);
#3225=FACE_OUTER_BOUND('',#4108,.T.);
#3226=FACE_OUTER_BOUND('',#4109,.T.);
#3227=FACE_OUTER_BOUND('',#4110,.T.);
#3228=FACE_OUTER_BOUND('',#4111,.T.);
#3229=FACE_OUTER_BOUND('',#4112,.T.);
#3230=FACE_OUTER_BOUND('',#4113,.T.);
#3231=FACE_OUTER_BOUND('',#4114,.T.);
#3232=FACE_OUTER_BOUND('',#4115,.T.);
#3233=FACE_OUTER_BOUND('',#4116,.T.);
#3234=FACE_OUTER_BOUND('',#4117,.T.);
#3235=FACE_OUTER_BOUND('',#4118,.T.);
#3236=FACE_OUTER_BOUND('',#4119,.T.);
#3237=FACE_OUTER_BOUND('',#4120,.T.);
#3238=FACE_OUTER_BOUND('',#4121,.T.);
#3239=FACE_OUTER_BOUND('',#4122,.T.);
#3240=FACE_OUTER_BOUND('',#4123,.T.);
#3241=FACE_OUTER_BOUND('',#4124,.T.);
#3242=FACE_OUTER_BOUND('',#4125,.T.);
#3243=FACE_OUTER_BOUND('',#4126,.T.);
#3244=FACE_OUTER_BOUND('',#4127,.T.);
#3245=FACE_OUTER_BOUND('',#4128,.T.);
#3246=FACE_OUTER_BOUND('',#4129,.T.);
#3247=FACE_OUTER_BOUND('',#4130,.T.);
#3248=FACE_OUTER_BOUND('',#4131,.T.);
#3249=FACE_OUTER_BOUND('',#4132,.T.);
#3250=FACE_OUTER_BOUND('',#4133,.T.);
#3251=FACE_OUTER_BOUND('',#4134,.T.);
#3252=FACE_OUTER_BOUND('',#4135,.T.);
#3253=FACE_OUTER_BOUND('',#4136,.T.);
#3254=FACE_OUTER_BOUND('',#4137,.T.);
#3255=FACE_OUTER_BOUND('',#4138,.T.);
#3256=FACE_OUTER_BOUND('',#4139,.T.);
#3257=FACE_OUTER_BOUND('',#4140,.T.);
#3258=FACE_OUTER_BOUND('',#4141,.T.);
#3259=FACE_OUTER_BOUND('',#4142,.T.);
#3260=FACE_OUTER_BOUND('',#4143,.T.);
#3261=FACE_OUTER_BOUND('',#4144,.T.);
#3262=FACE_OUTER_BOUND('',#4145,.T.);
#3263=FACE_OUTER_BOUND('',#4146,.T.);
#3264=FACE_OUTER_BOUND('',#4147,.T.);
#3265=FACE_OUTER_BOUND('',#4148,.T.);
#3266=FACE_OUTER_BOUND('',#4149,.T.);
#3267=FACE_OUTER_BOUND('',#4150,.T.);
#3268=FACE_OUTER_BOUND('',#4151,.T.);
#3269=FACE_OUTER_BOUND('',#4152,.T.);
#3270=FACE_OUTER_BOUND('',#4153,.T.);
#3271=FACE_OUTER_BOUND('',#4154,.T.);
#3272=FACE_OUTER_BOUND('',#4155,.T.);
#3273=FACE_OUTER_BOUND('',#4156,.T.);
#3274=FACE_OUTER_BOUND('',#4157,.T.);
#3275=FACE_OUTER_BOUND('',#4158,.T.);
#3276=FACE_OUTER_BOUND('',#4159,.T.);
#3277=FACE_OUTER_BOUND('',#4160,.T.);
#3278=FACE_OUTER_BOUND('',#4161,.T.);
#3279=FACE_OUTER_BOUND('',#4162,.T.);
#3280=FACE_OUTER_BOUND('',#4163,.T.);
#3281=FACE_OUTER_BOUND('',#4164,.T.);
#3282=FACE_OUTER_BOUND('',#4165,.T.);
#3283=FACE_OUTER_BOUND('',#4166,.T.);
#3284=FACE_OUTER_BOUND('',#4167,.T.);
#3285=FACE_OUTER_BOUND('',#4168,.T.);
#3286=FACE_OUTER_BOUND('',#4169,.T.);
#3287=FACE_OUTER_BOUND('',#4170,.T.);
#3288=FACE_OUTER_BOUND('',#4171,.T.);
#3289=FACE_OUTER_BOUND('',#4172,.T.);
#3290=FACE_OUTER_BOUND('',#4173,.T.);
#3291=FACE_OUTER_BOUND('',#4174,.T.);
#3292=FACE_OUTER_BOUND('',#4175,.T.);
#3293=FACE_OUTER_BOUND('',#4176,.T.);
#3294=FACE_OUTER_BOUND('',#4177,.T.);
#3295=FACE_OUTER_BOUND('',#4178,.T.);
#3296=FACE_OUTER_BOUND('',#4179,.T.);
#3297=FACE_OUTER_BOUND('',#4180,.T.);
#3298=FACE_OUTER_BOUND('',#4181,.T.);
#3299=FACE_OUTER_BOUND('',#4182,.T.);
#3300=FACE_OUTER_BOUND('',#4183,.T.);
#3301=FACE_OUTER_BOUND('',#4184,.T.);
#3302=FACE_OUTER_BOUND('',#4185,.T.);
#3303=FACE_OUTER_BOUND('',#4186,.T.);
#3304=FACE_OUTER_BOUND('',#4187,.T.);
#3305=FACE_OUTER_BOUND('',#4188,.T.);
#3306=FACE_OUTER_BOUND('',#4189,.T.);
#3307=FACE_OUTER_BOUND('',#4190,.T.);
#3308=FACE_OUTER_BOUND('',#4191,.T.);
#3309=FACE_OUTER_BOUND('',#4192,.T.);
#3310=FACE_OUTER_BOUND('',#4193,.T.);
#3311=FACE_OUTER_BOUND('',#4194,.T.);
#3312=FACE_OUTER_BOUND('',#4195,.T.);
#3313=FACE_OUTER_BOUND('',#4197,.T.);
#3314=FACE_OUTER_BOUND('',#4199,.T.);
#3315=FACE_OUTER_BOUND('',#4200,.T.);
#3316=FACE_OUTER_BOUND('',#4201,.T.);
#3317=FACE_OUTER_BOUND('',#4202,.T.);
#3318=FACE_OUTER_BOUND('',#4203,.T.);
#3319=FACE_OUTER_BOUND('',#4204,.T.);
#3320=FACE_OUTER_BOUND('',#4205,.T.);
#3321=FACE_OUTER_BOUND('',#4206,.T.);
#3322=FACE_OUTER_BOUND('',#4207,.T.);
#3323=FACE_OUTER_BOUND('',#4208,.T.);
#3324=FACE_OUTER_BOUND('',#4209,.T.);
#3325=FACE_OUTER_BOUND('',#4210,.T.);
#3326=FACE_OUTER_BOUND('',#4211,.T.);
#3327=FACE_OUTER_BOUND('',#4219,.T.);
#3328=FACE_OUTER_BOUND('',#4220,.T.);
#3329=FACE_OUTER_BOUND('',#4227,.T.);
#3330=FACE_OUTER_BOUND('',#4229,.T.);
#3331=FACE_OUTER_BOUND('',#4230,.T.);
#3332=FACE_OUTER_BOUND('',#4231,.T.);
#3333=FACE_OUTER_BOUND('',#4232,.T.);
#3334=FACE_OUTER_BOUND('',#4234,.T.);
#3335=FACE_OUTER_BOUND('',#4236,.T.);
#3336=FACE_OUTER_BOUND('',#4237,.T.);
#3337=FACE_OUTER_BOUND('',#4238,.T.);
#3338=FACE_OUTER_BOUND('',#4239,.T.);
#3339=FACE_OUTER_BOUND('',#4240,.T.);
#3340=FACE_OUTER_BOUND('',#4241,.T.);
#3341=FACE_OUTER_BOUND('',#4242,.T.);
#3342=FACE_OUTER_BOUND('',#4243,.T.);
#3343=FACE_OUTER_BOUND('',#4244,.T.);
#3344=FACE_OUTER_BOUND('',#4245,.T.);
#3345=FACE_OUTER_BOUND('',#4246,.T.);
#3346=FACE_OUTER_BOUND('',#4247,.T.);
#3347=FACE_OUTER_BOUND('',#4248,.T.);
#3348=FACE_OUTER_BOUND('',#4249,.T.);
#3349=FACE_OUTER_BOUND('',#4250,.T.);
#3350=FACE_OUTER_BOUND('',#4251,.T.);
#3351=FACE_OUTER_BOUND('',#4252,.T.);
#3352=FACE_OUTER_BOUND('',#4253,.T.);
#3353=FACE_OUTER_BOUND('',#4254,.T.);
#3354=FACE_OUTER_BOUND('',#4255,.T.);
#3355=FACE_OUTER_BOUND('',#4256,.T.);
#3356=FACE_OUTER_BOUND('',#4257,.T.);
#3357=FACE_OUTER_BOUND('',#4258,.T.);
#3358=FACE_OUTER_BOUND('',#4259,.T.);
#3359=FACE_OUTER_BOUND('',#4260,.T.);
#3360=FACE_OUTER_BOUND('',#4261,.T.);
#3361=FACE_OUTER_BOUND('',#4262,.T.);
#3362=FACE_OUTER_BOUND('',#4263,.T.);
#3363=FACE_OUTER_BOUND('',#4264,.T.);
#3364=FACE_OUTER_BOUND('',#4265,.T.);
#3365=FACE_OUTER_BOUND('',#4266,.T.);
#3366=FACE_OUTER_BOUND('',#4267,.T.);
#3367=FACE_OUTER_BOUND('',#4268,.T.);
#3368=FACE_OUTER_BOUND('',#4269,.T.);
#3369=FACE_OUTER_BOUND('',#4270,.T.);
#3370=FACE_OUTER_BOUND('',#4271,.T.);
#3371=FACE_OUTER_BOUND('',#4272,.T.);
#3372=FACE_OUTER_BOUND('',#4273,.T.);
#3373=FACE_OUTER_BOUND('',#4274,.T.);
#3374=FACE_OUTER_BOUND('',#4275,.T.);
#3375=FACE_OUTER_BOUND('',#4276,.T.);
#3376=FACE_OUTER_BOUND('',#4277,.T.);
#3377=FACE_OUTER_BOUND('',#4278,.T.);
#3378=FACE_OUTER_BOUND('',#4279,.T.);
#3379=FACE_OUTER_BOUND('',#4280,.T.);
#3380=FACE_OUTER_BOUND('',#4281,.T.);
#3381=FACE_OUTER_BOUND('',#4282,.T.);
#3382=FACE_OUTER_BOUND('',#4283,.T.);
#3383=FACE_OUTER_BOUND('',#4284,.T.);
#3384=FACE_OUTER_BOUND('',#4285,.T.);
#3385=FACE_OUTER_BOUND('',#4286,.T.);
#3386=FACE_OUTER_BOUND('',#4287,.T.);
#3387=FACE_OUTER_BOUND('',#4288,.T.);
#3388=FACE_OUTER_BOUND('',#4289,.T.);
#3389=FACE_OUTER_BOUND('',#4290,.T.);
#3390=FACE_OUTER_BOUND('',#4292,.T.);
#3391=FACE_OUTER_BOUND('',#4294,.T.);
#3392=FACE_OUTER_BOUND('',#4295,.T.);
#3393=FACE_OUTER_BOUND('',#4296,.T.);
#3394=FACE_OUTER_BOUND('',#4298,.T.);
#3395=FACE_OUTER_BOUND('',#4299,.T.);
#3396=FACE_OUTER_BOUND('',#4300,.T.);
#3397=FACE_OUTER_BOUND('',#4302,.T.);
#3398=FACE_OUTER_BOUND('',#4303,.T.);
#3399=FACE_OUTER_BOUND('',#4304,.T.);
#3400=FACE_OUTER_BOUND('',#4306,.T.);
#3401=FACE_OUTER_BOUND('',#4307,.T.);
#3402=FACE_OUTER_BOUND('',#4308,.T.);
#3403=FACE_OUTER_BOUND('',#4309,.T.);
#3404=FACE_OUTER_BOUND('',#4310,.T.);
#3405=FACE_OUTER_BOUND('',#4316,.T.);
#3406=FACE_OUTER_BOUND('',#4322,.T.);
#3407=FACE_OUTER_BOUND('',#4323,.T.);
#3408=FACE_OUTER_BOUND('',#4324,.T.);
#3409=FACE_OUTER_BOUND('',#4325,.T.);
#3410=FACE_OUTER_BOUND('',#4326,.T.);
#3411=FACE_OUTER_BOUND('',#4328,.T.);
#3412=FACE_OUTER_BOUND('',#4330,.T.);
#3413=FACE_OUTER_BOUND('',#4331,.T.);
#3414=FACE_OUTER_BOUND('',#4332,.T.);
#3415=FACE_OUTER_BOUND('',#4333,.T.);
#3416=FACE_OUTER_BOUND('',#4334,.T.);
#3417=FACE_OUTER_BOUND('',#4336,.T.);
#3418=FACE_OUTER_BOUND('',#4338,.T.);
#3419=FACE_OUTER_BOUND('',#4339,.T.);
#3420=FACE_OUTER_BOUND('',#4340,.T.);
#3421=FACE_OUTER_BOUND('',#4341,.T.);
#3422=FACE_OUTER_BOUND('',#4342,.T.);
#3423=FACE_OUTER_BOUND('',#4343,.T.);
#3424=FACE_OUTER_BOUND('',#4344,.T.);
#3425=FACE_OUTER_BOUND('',#4345,.T.);
#3426=FACE_OUTER_BOUND('',#4346,.T.);
#3427=FACE_OUTER_BOUND('',#4347,.T.);
#3428=FACE_OUTER_BOUND('',#4348,.T.);
#3429=FACE_OUTER_BOUND('',#4349,.T.);
#3430=FACE_OUTER_BOUND('',#4350,.T.);
#3431=FACE_OUTER_BOUND('',#4351,.T.);
#3432=FACE_OUTER_BOUND('',#4352,.T.);
#3433=FACE_OUTER_BOUND('',#4353,.T.);
#3434=FACE_OUTER_BOUND('',#4354,.T.);
#3435=FACE_OUTER_BOUND('',#4355,.T.);
#3436=FACE_OUTER_BOUND('',#4356,.T.);
#3437=FACE_OUTER_BOUND('',#4357,.T.);
#3438=FACE_OUTER_BOUND('',#4358,.T.);
#3439=FACE_OUTER_BOUND('',#4359,.T.);
#3440=FACE_OUTER_BOUND('',#4360,.T.);
#3441=FACE_OUTER_BOUND('',#4361,.T.);
#3442=FACE_OUTER_BOUND('',#4362,.T.);
#3443=FACE_OUTER_BOUND('',#4363,.T.);
#3444=FACE_OUTER_BOUND('',#4364,.T.);
#3445=FACE_OUTER_BOUND('',#4366,.T.);
#3446=FACE_OUTER_BOUND('',#4367,.T.);
#3447=FACE_OUTER_BOUND('',#4368,.T.);
#3448=FACE_OUTER_BOUND('',#4369,.T.);
#3449=FACE_OUTER_BOUND('',#4371,.T.);
#3450=FACE_OUTER_BOUND('',#4373,.T.);
#3451=FACE_OUTER_BOUND('',#4374,.T.);
#3452=FACE_OUTER_BOUND('',#4375,.T.);
#3453=FACE_OUTER_BOUND('',#4376,.T.);
#3454=FACE_OUTER_BOUND('',#4377,.T.);
#3455=FACE_OUTER_BOUND('',#4378,.T.);
#3456=FACE_OUTER_BOUND('',#4379,.T.);
#3457=FACE_OUTER_BOUND('',#4380,.T.);
#3458=FACE_OUTER_BOUND('',#4381,.T.);
#3459=FACE_OUTER_BOUND('',#4382,.T.);
#3460=FACE_OUTER_BOUND('',#4383,.T.);
#3461=FACE_OUTER_BOUND('',#4384,.T.);
#3462=FACE_OUTER_BOUND('',#4385,.T.);
#3463=FACE_OUTER_BOUND('',#4386,.T.);
#3464=FACE_OUTER_BOUND('',#4387,.T.);
#3465=FACE_OUTER_BOUND('',#4388,.T.);
#3466=FACE_OUTER_BOUND('',#4389,.T.);
#3467=FACE_OUTER_BOUND('',#4390,.T.);
#3468=FACE_OUTER_BOUND('',#4391,.T.);
#3469=FACE_OUTER_BOUND('',#4392,.T.);
#3470=FACE_OUTER_BOUND('',#4393,.T.);
#3471=FACE_OUTER_BOUND('',#4394,.T.);
#3472=FACE_OUTER_BOUND('',#4395,.T.);
#3473=FACE_OUTER_BOUND('',#4396,.T.);
#3474=FACE_OUTER_BOUND('',#4397,.T.);
#3475=FACE_OUTER_BOUND('',#4398,.T.);
#3476=FACE_OUTER_BOUND('',#4399,.T.);
#3477=FACE_OUTER_BOUND('',#4400,.T.);
#3478=FACE_OUTER_BOUND('',#4401,.T.);
#3479=FACE_OUTER_BOUND('',#4402,.T.);
#3480=FACE_OUTER_BOUND('',#4403,.T.);
#3481=FACE_OUTER_BOUND('',#4404,.T.);
#3482=FACE_OUTER_BOUND('',#4405,.T.);
#3483=FACE_OUTER_BOUND('',#4406,.T.);
#3484=FACE_OUTER_BOUND('',#4407,.T.);
#3485=FACE_OUTER_BOUND('',#4408,.T.);
#3486=FACE_OUTER_BOUND('',#4409,.T.);
#3487=FACE_OUTER_BOUND('',#4410,.T.);
#3488=FACE_OUTER_BOUND('',#4411,.T.);
#3489=FACE_OUTER_BOUND('',#4412,.T.);
#3490=FACE_OUTER_BOUND('',#4413,.T.);
#3491=FACE_OUTER_BOUND('',#4414,.T.);
#3492=FACE_OUTER_BOUND('',#4415,.T.);
#3493=FACE_OUTER_BOUND('',#4416,.T.);
#3494=FACE_OUTER_BOUND('',#4417,.T.);
#3495=FACE_OUTER_BOUND('',#4419,.T.);
#3496=FACE_OUTER_BOUND('',#4420,.T.);
#3497=FACE_OUTER_BOUND('',#4422,.T.);
#3498=EDGE_LOOP('',(#9844,#9845,#9846,#9847));
#3499=EDGE_LOOP('',(#9848,#9849,#9850,#9851,#9852));
#3500=EDGE_LOOP('',(#9853,#9854,#9855,#9856));
#3501=EDGE_LOOP('',(#9857,#9858,#9859,#9860));
#3502=EDGE_LOOP('',(#9861,#9862,#9863,#9864,#9865));
#3503=EDGE_LOOP('',(#9866,#9867));
#3504=EDGE_LOOP('',(#9868,#9869,#9870,#9871));
#3505=EDGE_LOOP('',(#9872,#9873,#9874,#9875,#9876,#9877,#9878,#9879,#9880,
#9881,#9882,#9883));
#3506=EDGE_LOOP('',(#9884,#9885,#9886,#9887));
#3507=EDGE_LOOP('',(#9888,#9889,#9890,#9891));
#3508=EDGE_LOOP('',(#9892,#9893,#9894,#9895));
#3509=EDGE_LOOP('',(#9896,#9897,#9898,#9899));
#3510=EDGE_LOOP('',(#9900,#9901,#9902,#9903));
#3511=EDGE_LOOP('',(#9904,#9905,#9906,#9907));
#3512=EDGE_LOOP('',(#9908,#9909,#9910,#9911));
#3513=EDGE_LOOP('',(#9912,#9913,#9914,#9915));
#3514=EDGE_LOOP('',(#9916,#9917,#9918,#9919));
#3515=EDGE_LOOP('',(#9920,#9921,#9922,#9923,#9924,#9925));
#3516=EDGE_LOOP('',(#9926));
#3517=EDGE_LOOP('',(#9927));
#3518=EDGE_LOOP('',(#9928));
#3519=EDGE_LOOP('',(#9929));
#3520=EDGE_LOOP('',(#9930));
#3521=EDGE_LOOP('',(#9931));
#3522=EDGE_LOOP('',(#9932));
#3523=EDGE_LOOP('',(#9933));
#3524=EDGE_LOOP('',(#9934));
#3525=EDGE_LOOP('',(#9935));
#3526=EDGE_LOOP('',(#9936));
#3527=EDGE_LOOP('',(#9937));
#3528=EDGE_LOOP('',(#9938));
#3529=EDGE_LOOP('',(#9939));
#3530=EDGE_LOOP('',(#9940));
#3531=EDGE_LOOP('',(#9941,#9942,#9943,#9944));
#3532=EDGE_LOOP('',(#9945,#9946,#9947,#9948));
#3533=EDGE_LOOP('',(#9949,#9950,#9951,#9952,#9953,#9954,#9955,#9956,#9957,
#9958,#9959,#9960));
#3534=EDGE_LOOP('',(#9961,#9962,#9963,#9964,#9965));
#3535=EDGE_LOOP('',(#9966));
#3536=EDGE_LOOP('',(#9967));
#3537=EDGE_LOOP('',(#9968));
#3538=EDGE_LOOP('',(#9969));
#3539=EDGE_LOOP('',(#9970,#9971,#9972));
#3540=EDGE_LOOP('',(#9973,#9974,#9975,#9976,#9977));
#3541=EDGE_LOOP('',(#9978,#9979,#9980,#9981));
#3542=EDGE_LOOP('',(#9982,#9983,#9984,#9985));
#3543=EDGE_LOOP('',(#9986,#9987,#9988,#9989));
#3544=EDGE_LOOP('',(#9990,#9991,#9992,#9993));
#3545=EDGE_LOOP('',(#9994,#9995,#9996,#9997));
#3546=EDGE_LOOP('',(#9998,#9999,#10000,#10001));
#3547=EDGE_LOOP('',(#10002,#10003,#10004,#10005));
#3548=EDGE_LOOP('',(#10006,#10007,#10008,#10009));
#3549=EDGE_LOOP('',(#10010,#10011,#10012,#10013));
#3550=EDGE_LOOP('',(#10014,#10015,#10016,#10017));
#3551=EDGE_LOOP('',(#10018,#10019,#10020,#10021));
#3552=EDGE_LOOP('',(#10022,#10023,#10024,#10025));
#3553=EDGE_LOOP('',(#10026,#10027,#10028,#10029,#10030,#10031,#10032,#10033));
#3554=EDGE_LOOP('',(#10034,#10035,#10036,#10037));
#3555=EDGE_LOOP('',(#10038,#10039,#10040,#10041));
#3556=EDGE_LOOP('',(#10042,#10043,#10044,#10045));
#3557=EDGE_LOOP('',(#10046,#10047,#10048,#10049));
#3558=EDGE_LOOP('',(#10050,#10051,#10052,#10053));
#3559=EDGE_LOOP('',(#10054,#10055,#10056,#10057));
#3560=EDGE_LOOP('',(#10058,#10059,#10060,#10061));
#3561=EDGE_LOOP('',(#10062,#10063,#10064,#10065));
#3562=EDGE_LOOP('',(#10066,#10067,#10068,#10069));
#3563=EDGE_LOOP('',(#10070,#10071,#10072,#10073));
#3564=EDGE_LOOP('',(#10074,#10075,#10076,#10077));
#3565=EDGE_LOOP('',(#10078,#10079,#10080,#10081));
#3566=EDGE_LOOP('',(#10082,#10083,#10084,#10085));
#3567=EDGE_LOOP('',(#10086,#10087,#10088,#10089));
#3568=EDGE_LOOP('',(#10090,#10091,#10092,#10093));
#3569=EDGE_LOOP('',(#10094,#10095,#10096,#10097));
#3570=EDGE_LOOP('',(#10098,#10099,#10100,#10101));
#3571=EDGE_LOOP('',(#10102,#10103,#10104,#10105));
#3572=EDGE_LOOP('',(#10106,#10107,#10108,#10109));
#3573=EDGE_LOOP('',(#10110,#10111,#10112,#10113));
#3574=EDGE_LOOP('',(#10114,#10115,#10116,#10117));
#3575=EDGE_LOOP('',(#10118,#10119,#10120,#10121));
#3576=EDGE_LOOP('',(#10122,#10123,#10124,#10125));
#3577=EDGE_LOOP('',(#10126,#10127,#10128,#10129));
#3578=EDGE_LOOP('',(#10130,#10131,#10132,#10133));
#3579=EDGE_LOOP('',(#10134,#10135,#10136,#10137));
#3580=EDGE_LOOP('',(#10138,#10139,#10140,#10141));
#3581=EDGE_LOOP('',(#10142,#10143,#10144,#10145));
#3582=EDGE_LOOP('',(#10146,#10147,#10148,#10149));
#3583=EDGE_LOOP('',(#10150,#10151,#10152,#10153));
#3584=EDGE_LOOP('',(#10154,#10155,#10156,#10157));
#3585=EDGE_LOOP('',(#10158,#10159,#10160,#10161));
#3586=EDGE_LOOP('',(#10162,#10163,#10164,#10165));
#3587=EDGE_LOOP('',(#10166,#10167,#10168,#10169));
#3588=EDGE_LOOP('',(#10170,#10171,#10172,#10173));
#3589=EDGE_LOOP('',(#10174,#10175,#10176,#10177));
#3590=EDGE_LOOP('',(#10178,#10179,#10180,#10181,#10182,#10183,#10184,#10185));
#3591=EDGE_LOOP('',(#10186,#10187,#10188,#10189));
#3592=EDGE_LOOP('',(#10190,#10191,#10192,#10193));
#3593=EDGE_LOOP('',(#10194,#10195,#10196,#10197));
#3594=EDGE_LOOP('',(#10198,#10199,#10200,#10201));
#3595=EDGE_LOOP('',(#10202,#10203,#10204,#10205));
#3596=EDGE_LOOP('',(#10206,#10207,#10208,#10209));
#3597=EDGE_LOOP('',(#10210,#10211,#10212,#10213));
#3598=EDGE_LOOP('',(#10214,#10215,#10216,#10217));
#3599=EDGE_LOOP('',(#10218,#10219,#10220,#10221));
#3600=EDGE_LOOP('',(#10222,#10223,#10224,#10225));
#3601=EDGE_LOOP('',(#10226,#10227,#10228,#10229));
#3602=EDGE_LOOP('',(#10230,#10231,#10232,#10233));
#3603=EDGE_LOOP('',(#10234,#10235,#10236,#10237));
#3604=EDGE_LOOP('',(#10238,#10239,#10240,#10241));
#3605=EDGE_LOOP('',(#10242,#10243,#10244,#10245));
#3606=EDGE_LOOP('',(#10246,#10247,#10248,#10249));
#3607=EDGE_LOOP('',(#10250,#10251,#10252,#10253));
#3608=EDGE_LOOP('',(#10254,#10255,#10256,#10257));
#3609=EDGE_LOOP('',(#10258,#10259,#10260,#10261));
#3610=EDGE_LOOP('',(#10262,#10263,#10264,#10265));
#3611=EDGE_LOOP('',(#10266,#10267,#10268,#10269));
#3612=EDGE_LOOP('',(#10270,#10271,#10272,#10273));
#3613=EDGE_LOOP('',(#10274,#10275,#10276,#10277));
#3614=EDGE_LOOP('',(#10278,#10279,#10280,#10281));
#3615=EDGE_LOOP('',(#10282,#10283,#10284,#10285));
#3616=EDGE_LOOP('',(#10286,#10287,#10288,#10289));
#3617=EDGE_LOOP('',(#10290,#10291,#10292,#10293));
#3618=EDGE_LOOP('',(#10294,#10295,#10296,#10297));
#3619=EDGE_LOOP('',(#10298,#10299,#10300,#10301));
#3620=EDGE_LOOP('',(#10302,#10303,#10304,#10305));
#3621=EDGE_LOOP('',(#10306,#10307,#10308,#10309));
#3622=EDGE_LOOP('',(#10310,#10311,#10312,#10313));
#3623=EDGE_LOOP('',(#10314,#10315,#10316,#10317));
#3624=EDGE_LOOP('',(#10318,#10319,#10320,#10321));
#3625=EDGE_LOOP('',(#10322,#10323,#10324,#10325));
#3626=EDGE_LOOP('',(#10326,#10327,#10328,#10329));
#3627=EDGE_LOOP('',(#10330,#10331,#10332,#10333,#10334,#10335,#10336,#10337));
#3628=EDGE_LOOP('',(#10338,#10339,#10340,#10341));
#3629=EDGE_LOOP('',(#10342,#10343,#10344,#10345));
#3630=EDGE_LOOP('',(#10346,#10347,#10348,#10349));
#3631=EDGE_LOOP('',(#10350,#10351,#10352,#10353));
#3632=EDGE_LOOP('',(#10354,#10355,#10356,#10357));
#3633=EDGE_LOOP('',(#10358,#10359,#10360,#10361));
#3634=EDGE_LOOP('',(#10362,#10363,#10364,#10365));
#3635=EDGE_LOOP('',(#10366,#10367,#10368,#10369));
#3636=EDGE_LOOP('',(#10370,#10371,#10372,#10373));
#3637=EDGE_LOOP('',(#10374,#10375,#10376,#10377));
#3638=EDGE_LOOP('',(#10378,#10379,#10380,#10381));
#3639=EDGE_LOOP('',(#10382,#10383,#10384,#10385));
#3640=EDGE_LOOP('',(#10386,#10387,#10388,#10389));
#3641=EDGE_LOOP('',(#10390,#10391,#10392,#10393));
#3642=EDGE_LOOP('',(#10394,#10395,#10396,#10397));
#3643=EDGE_LOOP('',(#10398,#10399,#10400,#10401));
#3644=EDGE_LOOP('',(#10402,#10403,#10404,#10405));
#3645=EDGE_LOOP('',(#10406,#10407,#10408,#10409));
#3646=EDGE_LOOP('',(#10410,#10411,#10412,#10413));
#3647=EDGE_LOOP('',(#10414,#10415,#10416,#10417));
#3648=EDGE_LOOP('',(#10418,#10419,#10420,#10421));
#3649=EDGE_LOOP('',(#10422,#10423,#10424,#10425));
#3650=EDGE_LOOP('',(#10426,#10427,#10428,#10429));
#3651=EDGE_LOOP('',(#10430,#10431,#10432,#10433));
#3652=EDGE_LOOP('',(#10434,#10435,#10436,#10437));
#3653=EDGE_LOOP('',(#10438,#10439,#10440,#10441));
#3654=EDGE_LOOP('',(#10442,#10443,#10444,#10445));
#3655=EDGE_LOOP('',(#10446,#10447,#10448,#10449));
#3656=EDGE_LOOP('',(#10450,#10451,#10452,#10453));
#3657=EDGE_LOOP('',(#10454,#10455,#10456,#10457));
#3658=EDGE_LOOP('',(#10458,#10459,#10460,#10461));
#3659=EDGE_LOOP('',(#10462,#10463,#10464,#10465));
#3660=EDGE_LOOP('',(#10466,#10467,#10468,#10469));
#3661=EDGE_LOOP('',(#10470,#10471,#10472,#10473));
#3662=EDGE_LOOP('',(#10474,#10475,#10476,#10477));
#3663=EDGE_LOOP('',(#10478,#10479,#10480,#10481));
#3664=EDGE_LOOP('',(#10482,#10483,#10484,#10485,#10486,#10487,#10488,#10489));
#3665=EDGE_LOOP('',(#10490,#10491,#10492,#10493));
#3666=EDGE_LOOP('',(#10494,#10495,#10496,#10497));
#3667=EDGE_LOOP('',(#10498,#10499,#10500,#10501));
#3668=EDGE_LOOP('',(#10502,#10503,#10504,#10505));
#3669=EDGE_LOOP('',(#10506,#10507,#10508,#10509));
#3670=EDGE_LOOP('',(#10510,#10511,#10512,#10513));
#3671=EDGE_LOOP('',(#10514,#10515,#10516,#10517));
#3672=EDGE_LOOP('',(#10518,#10519,#10520,#10521));
#3673=EDGE_LOOP('',(#10522,#10523,#10524,#10525));
#3674=EDGE_LOOP('',(#10526,#10527,#10528,#10529));
#3675=EDGE_LOOP('',(#10530,#10531,#10532,#10533));
#3676=EDGE_LOOP('',(#10534,#10535,#10536,#10537));
#3677=EDGE_LOOP('',(#10538,#10539,#10540,#10541));
#3678=EDGE_LOOP('',(#10542,#10543,#10544,#10545));
#3679=EDGE_LOOP('',(#10546,#10547,#10548,#10549));
#3680=EDGE_LOOP('',(#10550,#10551,#10552,#10553));
#3681=EDGE_LOOP('',(#10554,#10555,#10556,#10557));
#3682=EDGE_LOOP('',(#10558,#10559,#10560,#10561));
#3683=EDGE_LOOP('',(#10562,#10563,#10564,#10565));
#3684=EDGE_LOOP('',(#10566,#10567,#10568,#10569));
#3685=EDGE_LOOP('',(#10570,#10571,#10572,#10573));
#3686=EDGE_LOOP('',(#10574,#10575,#10576,#10577));
#3687=EDGE_LOOP('',(#10578,#10579,#10580,#10581));
#3688=EDGE_LOOP('',(#10582,#10583,#10584,#10585));
#3689=EDGE_LOOP('',(#10586,#10587,#10588,#10589));
#3690=EDGE_LOOP('',(#10590,#10591,#10592,#10593));
#3691=EDGE_LOOP('',(#10594,#10595,#10596,#10597));
#3692=EDGE_LOOP('',(#10598,#10599,#10600,#10601));
#3693=EDGE_LOOP('',(#10602,#10603,#10604,#10605));
#3694=EDGE_LOOP('',(#10606,#10607,#10608,#10609));
#3695=EDGE_LOOP('',(#10610,#10611,#10612,#10613));
#3696=EDGE_LOOP('',(#10614,#10615,#10616,#10617));
#3697=EDGE_LOOP('',(#10618,#10619,#10620,#10621));
#3698=EDGE_LOOP('',(#10622,#10623,#10624,#10625));
#3699=EDGE_LOOP('',(#10626,#10627,#10628,#10629));
#3700=EDGE_LOOP('',(#10630,#10631,#10632,#10633));
#3701=EDGE_LOOP('',(#10634,#10635,#10636,#10637,#10638,#10639,#10640,#10641));
#3702=EDGE_LOOP('',(#10642,#10643,#10644,#10645));
#3703=EDGE_LOOP('',(#10646,#10647,#10648,#10649));
#3704=EDGE_LOOP('',(#10650,#10651,#10652,#10653));
#3705=EDGE_LOOP('',(#10654,#10655,#10656,#10657));
#3706=EDGE_LOOP('',(#10658,#10659,#10660,#10661));
#3707=EDGE_LOOP('',(#10662,#10663,#10664,#10665));
#3708=EDGE_LOOP('',(#10666,#10667,#10668,#10669));
#3709=EDGE_LOOP('',(#10670,#10671,#10672,#10673));
#3710=EDGE_LOOP('',(#10674,#10675,#10676,#10677));
#3711=EDGE_LOOP('',(#10678,#10679,#10680,#10681));
#3712=EDGE_LOOP('',(#10682,#10683,#10684,#10685));
#3713=EDGE_LOOP('',(#10686,#10687,#10688,#10689));
#3714=EDGE_LOOP('',(#10690,#10691,#10692,#10693));
#3715=EDGE_LOOP('',(#10694,#10695,#10696,#10697));
#3716=EDGE_LOOP('',(#10698,#10699,#10700,#10701));
#3717=EDGE_LOOP('',(#10702,#10703,#10704,#10705));
#3718=EDGE_LOOP('',(#10706,#10707,#10708,#10709));
#3719=EDGE_LOOP('',(#10710,#10711,#10712,#10713));
#3720=EDGE_LOOP('',(#10714,#10715,#10716,#10717));
#3721=EDGE_LOOP('',(#10718,#10719,#10720,#10721));
#3722=EDGE_LOOP('',(#10722,#10723,#10724,#10725));
#3723=EDGE_LOOP('',(#10726,#10727,#10728,#10729));
#3724=EDGE_LOOP('',(#10730,#10731,#10732,#10733));
#3725=EDGE_LOOP('',(#10734,#10735,#10736,#10737));
#3726=EDGE_LOOP('',(#10738,#10739,#10740,#10741));
#3727=EDGE_LOOP('',(#10742,#10743,#10744,#10745));
#3728=EDGE_LOOP('',(#10746,#10747,#10748,#10749));
#3729=EDGE_LOOP('',(#10750,#10751,#10752,#10753));
#3730=EDGE_LOOP('',(#10754,#10755,#10756,#10757));
#3731=EDGE_LOOP('',(#10758,#10759,#10760,#10761));
#3732=EDGE_LOOP('',(#10762,#10763,#10764,#10765));
#3733=EDGE_LOOP('',(#10766,#10767,#10768,#10769));
#3734=EDGE_LOOP('',(#10770,#10771,#10772,#10773));
#3735=EDGE_LOOP('',(#10774,#10775,#10776,#10777));
#3736=EDGE_LOOP('',(#10778,#10779,#10780,#10781));
#3737=EDGE_LOOP('',(#10782,#10783,#10784,#10785));
#3738=EDGE_LOOP('',(#10786,#10787,#10788,#10789,#10790,#10791,#10792,#10793));
#3739=EDGE_LOOP('',(#10794,#10795,#10796,#10797));
#3740=EDGE_LOOP('',(#10798,#10799,#10800,#10801));
#3741=EDGE_LOOP('',(#10802,#10803,#10804,#10805));
#3742=EDGE_LOOP('',(#10806,#10807,#10808,#10809));
#3743=EDGE_LOOP('',(#10810,#10811,#10812,#10813));
#3744=EDGE_LOOP('',(#10814,#10815,#10816,#10817));
#3745=EDGE_LOOP('',(#10818,#10819,#10820,#10821));
#3746=EDGE_LOOP('',(#10822,#10823,#10824,#10825));
#3747=EDGE_LOOP('',(#10826,#10827,#10828,#10829));
#3748=EDGE_LOOP('',(#10830,#10831,#10832,#10833));
#3749=EDGE_LOOP('',(#10834,#10835,#10836,#10837));
#3750=EDGE_LOOP('',(#10838,#10839,#10840,#10841));
#3751=EDGE_LOOP('',(#10842,#10843,#10844,#10845));
#3752=EDGE_LOOP('',(#10846,#10847,#10848,#10849));
#3753=EDGE_LOOP('',(#10850,#10851,#10852,#10853));
#3754=EDGE_LOOP('',(#10854,#10855,#10856,#10857));
#3755=EDGE_LOOP('',(#10858,#10859,#10860,#10861));
#3756=EDGE_LOOP('',(#10862,#10863,#10864,#10865));
#3757=EDGE_LOOP('',(#10866,#10867,#10868,#10869));
#3758=EDGE_LOOP('',(#10870,#10871,#10872,#10873));
#3759=EDGE_LOOP('',(#10874,#10875,#10876,#10877));
#3760=EDGE_LOOP('',(#10878,#10879,#10880,#10881));
#3761=EDGE_LOOP('',(#10882,#10883,#10884,#10885));
#3762=EDGE_LOOP('',(#10886,#10887,#10888,#10889));
#3763=EDGE_LOOP('',(#10890,#10891,#10892,#10893));
#3764=EDGE_LOOP('',(#10894,#10895,#10896,#10897));
#3765=EDGE_LOOP('',(#10898,#10899,#10900,#10901));
#3766=EDGE_LOOP('',(#10902,#10903,#10904,#10905));
#3767=EDGE_LOOP('',(#10906,#10907,#10908,#10909));
#3768=EDGE_LOOP('',(#10910,#10911,#10912,#10913));
#3769=EDGE_LOOP('',(#10914,#10915,#10916,#10917));
#3770=EDGE_LOOP('',(#10918,#10919,#10920,#10921));
#3771=EDGE_LOOP('',(#10922,#10923,#10924,#10925));
#3772=EDGE_LOOP('',(#10926,#10927,#10928,#10929));
#3773=EDGE_LOOP('',(#10930,#10931,#10932,#10933));
#3774=EDGE_LOOP('',(#10934,#10935,#10936,#10937));
#3775=EDGE_LOOP('',(#10938,#10939,#10940,#10941,#10942,#10943,#10944,#10945));
#3776=EDGE_LOOP('',(#10946,#10947,#10948,#10949));
#3777=EDGE_LOOP('',(#10950,#10951,#10952,#10953));
#3778=EDGE_LOOP('',(#10954,#10955,#10956,#10957));
#3779=EDGE_LOOP('',(#10958,#10959,#10960,#10961));
#3780=EDGE_LOOP('',(#10962,#10963,#10964,#10965));
#3781=EDGE_LOOP('',(#10966,#10967,#10968,#10969));
#3782=EDGE_LOOP('',(#10970,#10971,#10972,#10973));
#3783=EDGE_LOOP('',(#10974,#10975,#10976,#10977));
#3784=EDGE_LOOP('',(#10978,#10979,#10980,#10981));
#3785=EDGE_LOOP('',(#10982,#10983,#10984,#10985));
#3786=EDGE_LOOP('',(#10986,#10987,#10988,#10989));
#3787=EDGE_LOOP('',(#10990,#10991,#10992,#10993));
#3788=EDGE_LOOP('',(#10994,#10995,#10996,#10997));
#3789=EDGE_LOOP('',(#10998,#10999,#11000,#11001));
#3790=EDGE_LOOP('',(#11002,#11003,#11004,#11005));
#3791=EDGE_LOOP('',(#11006,#11007,#11008,#11009));
#3792=EDGE_LOOP('',(#11010,#11011,#11012,#11013));
#3793=EDGE_LOOP('',(#11014,#11015,#11016,#11017));
#3794=EDGE_LOOP('',(#11018,#11019,#11020,#11021));
#3795=EDGE_LOOP('',(#11022,#11023,#11024,#11025));
#3796=EDGE_LOOP('',(#11026,#11027,#11028,#11029));
#3797=EDGE_LOOP('',(#11030,#11031,#11032,#11033));
#3798=EDGE_LOOP('',(#11034,#11035,#11036,#11037));
#3799=EDGE_LOOP('',(#11038,#11039,#11040,#11041));
#3800=EDGE_LOOP('',(#11042,#11043,#11044,#11045));
#3801=EDGE_LOOP('',(#11046,#11047,#11048,#11049));
#3802=EDGE_LOOP('',(#11050,#11051,#11052,#11053));
#3803=EDGE_LOOP('',(#11054,#11055,#11056,#11057));
#3804=EDGE_LOOP('',(#11058,#11059,#11060,#11061));
#3805=EDGE_LOOP('',(#11062,#11063,#11064,#11065));
#3806=EDGE_LOOP('',(#11066,#11067,#11068,#11069));
#3807=EDGE_LOOP('',(#11070,#11071,#11072,#11073));
#3808=EDGE_LOOP('',(#11074,#11075,#11076,#11077));
#3809=EDGE_LOOP('',(#11078,#11079,#11080,#11081));
#3810=EDGE_LOOP('',(#11082,#11083,#11084,#11085));
#3811=EDGE_LOOP('',(#11086,#11087,#11088,#11089));
#3812=EDGE_LOOP('',(#11090,#11091,#11092,#11093,#11094,#11095,#11096,#11097));
#3813=EDGE_LOOP('',(#11098,#11099,#11100,#11101));
#3814=EDGE_LOOP('',(#11102,#11103,#11104,#11105));
#3815=EDGE_LOOP('',(#11106,#11107,#11108,#11109));
#3816=EDGE_LOOP('',(#11110,#11111,#11112,#11113));
#3817=EDGE_LOOP('',(#11114,#11115,#11116,#11117));
#3818=EDGE_LOOP('',(#11118,#11119,#11120,#11121));
#3819=EDGE_LOOP('',(#11122,#11123,#11124,#11125));
#3820=EDGE_LOOP('',(#11126,#11127,#11128,#11129));
#3821=EDGE_LOOP('',(#11130,#11131,#11132,#11133));
#3822=EDGE_LOOP('',(#11134,#11135,#11136,#11137));
#3823=EDGE_LOOP('',(#11138,#11139,#11140,#11141));
#3824=EDGE_LOOP('',(#11142,#11143,#11144,#11145));
#3825=EDGE_LOOP('',(#11146,#11147,#11148,#11149));
#3826=EDGE_LOOP('',(#11150,#11151,#11152,#11153));
#3827=EDGE_LOOP('',(#11154,#11155,#11156,#11157));
#3828=EDGE_LOOP('',(#11158,#11159,#11160,#11161));
#3829=EDGE_LOOP('',(#11162,#11163,#11164,#11165));
#3830=EDGE_LOOP('',(#11166,#11167,#11168,#11169));
#3831=EDGE_LOOP('',(#11170,#11171,#11172,#11173));
#3832=EDGE_LOOP('',(#11174,#11175,#11176,#11177));
#3833=EDGE_LOOP('',(#11178,#11179,#11180,#11181));
#3834=EDGE_LOOP('',(#11182,#11183,#11184,#11185));
#3835=EDGE_LOOP('',(#11186,#11187,#11188,#11189));
#3836=EDGE_LOOP('',(#11190,#11191,#11192,#11193));
#3837=EDGE_LOOP('',(#11194,#11195,#11196,#11197));
#3838=EDGE_LOOP('',(#11198,#11199,#11200,#11201));
#3839=EDGE_LOOP('',(#11202,#11203,#11204,#11205));
#3840=EDGE_LOOP('',(#11206,#11207,#11208,#11209));
#3841=EDGE_LOOP('',(#11210,#11211,#11212,#11213));
#3842=EDGE_LOOP('',(#11214,#11215,#11216,#11217));
#3843=EDGE_LOOP('',(#11218,#11219,#11220,#11221));
#3844=EDGE_LOOP('',(#11222,#11223,#11224,#11225));
#3845=EDGE_LOOP('',(#11226,#11227,#11228,#11229));
#3846=EDGE_LOOP('',(#11230,#11231,#11232,#11233));
#3847=EDGE_LOOP('',(#11234,#11235,#11236,#11237));
#3848=EDGE_LOOP('',(#11238,#11239,#11240,#11241));
#3849=EDGE_LOOP('',(#11242,#11243,#11244,#11245,#11246));
#3850=EDGE_LOOP('',(#11247,#11248,#11249,#11250));
#3851=EDGE_LOOP('',(#11251,#11252,#11253,#11254,#11255,#11256,#11257,#11258,
#11259,#11260,#11261,#11262,#11263,#11264,#11265,#11266,#11267,#11268,#11269,
#11270,#11271,#11272,#11273,#11274,#11275,#11276,#11277,#11278,#11279,#11280,
#11281,#11282,#11283,#11284,#11285,#11286,#11287,#11288,#11289,#11290,#11291));
#3852=EDGE_LOOP('',(#11292,#11293,#11294,#11295,#11296,#11297,#11298,#11299,
#11300,#11301,#11302,#11303,#11304,#11305,#11306,#11307,#11308,#11309,#11310,
#11311,#11312,#11313,#11314,#11315,#11316,#11317,#11318,#11319,#11320,#11321,
#11322,#11323,#11324,#11325,#11326,#11327,#11328,#11329,#11330,#11331,#11332));
#3853=EDGE_LOOP('',(#11333,#11334,#11335,#11336));
#3854=EDGE_LOOP('',(#11337,#11338,#11339,#11340,#11341));
#3855=EDGE_LOOP('',(#11342,#11343,#11344,#11345));
#3856=EDGE_LOOP('',(#11346,#11347,#11348,#11349,#11350,#11351,#11352,#11353,
#11354,#11355,#11356,#11357,#11358,#11359,#11360,#11361,#11362,#11363,#11364,
#11365,#11366,#11367,#11368,#11369,#11370,#11371,#11372,#11373,#11374,#11375,
#11376,#11377,#11378,#11379,#11380,#11381,#11382,#11383,#11384,#11385,#11386));
#3857=EDGE_LOOP('',(#11387,#11388,#11389,#11390,#11391,#11392,#11393,#11394,
#11395,#11396,#11397,#11398,#11399,#11400,#11401,#11402,#11403,#11404,#11405,
#11406,#11407,#11408,#11409,#11410,#11411,#11412,#11413,#11414,#11415,#11416,
#11417,#11418,#11419,#11420,#11421,#11422,#11423,#11424,#11425,#11426,#11427));
#3858=EDGE_LOOP('',(#11428,#11429,#11430,#11431));
#3859=EDGE_LOOP('',(#11432,#11433,#11434,#11435,#11436));
#3860=EDGE_LOOP('',(#11437,#11438,#11439,#11440));
#3861=EDGE_LOOP('',(#11441,#11442,#11443,#11444,#11445,#11446,#11447,#11448,
#11449,#11450,#11451,#11452,#11453,#11454,#11455,#11456,#11457,#11458,#11459,
#11460,#11461,#11462,#11463,#11464,#11465,#11466,#11467,#11468,#11469,#11470,
#11471,#11472,#11473,#11474,#11475,#11476,#11477,#11478,#11479,#11480,#11481));
#3862=EDGE_LOOP('',(#11482,#11483,#11484,#11485,#11486,#11487,#11488,#11489,
#11490,#11491,#11492,#11493,#11494,#11495,#11496,#11497,#11498,#11499,#11500,
#11501,#11502,#11503,#11504,#11505,#11506,#11507,#11508,#11509,#11510,#11511,
#11512,#11513,#11514,#11515,#11516,#11517,#11518,#11519,#11520,#11521,#11522));
#3863=EDGE_LOOP('',(#11523,#11524,#11525,#11526));
#3864=EDGE_LOOP('',(#11527,#11528,#11529,#11530,#11531));
#3865=EDGE_LOOP('',(#11532,#11533,#11534,#11535));
#3866=EDGE_LOOP('',(#11536,#11537,#11538,#11539,#11540,#11541,#11542,#11543,
#11544,#11545,#11546,#11547,#11548,#11549,#11550,#11551,#11552,#11553,#11554,
#11555,#11556,#11557,#11558,#11559,#11560,#11561,#11562,#11563,#11564,#11565,
#11566,#11567,#11568,#11569,#11570,#11571,#11572,#11573,#11574,#11575,#11576));
#3867=EDGE_LOOP('',(#11577,#11578,#11579,#11580,#11581,#11582,#11583,#11584,
#11585,#11586,#11587,#11588,#11589,#11590,#11591,#11592,#11593,#11594,#11595,
#11596,#11597,#11598,#11599,#11600,#11601,#11602,#11603,#11604,#11605,#11606,
#11607,#11608,#11609,#11610,#11611,#11612,#11613,#11614,#11615,#11616,#11617));
#3868=EDGE_LOOP('',(#11618,#11619,#11620,#11621));
#3869=EDGE_LOOP('',(#11622));
#3870=EDGE_LOOP('',(#11623));
#3871=EDGE_LOOP('',(#11624));
#3872=EDGE_LOOP('',(#11625));
#3873=EDGE_LOOP('',(#11626,#11627,#11628,#11629,#11630));
#3874=EDGE_LOOP('',(#11631,#11632,#11633,#11634));
#3875=EDGE_LOOP('',(#11635,#11636,#11637,#11638,#11639,#11640,#11641,#11642,
#11643,#11644,#11645,#11646,#11647,#11648,#11649,#11650,#11651,#11652,#11653,
#11654,#11655,#11656,#11657,#11658,#11659,#11660,#11661,#11662,#11663,#11664,
#11665,#11666,#11667,#11668,#11669,#11670,#11671,#11672,#11673,#11674,#11675));
#3876=EDGE_LOOP('',(#11676,#11677,#11678,#11679,#11680,#11681,#11682,#11683,
#11684,#11685,#11686,#11687,#11688,#11689,#11690,#11691,#11692,#11693,#11694,
#11695,#11696,#11697,#11698,#11699,#11700,#11701,#11702,#11703,#11704,#11705,
#11706,#11707,#11708,#11709,#11710,#11711,#11712,#11713,#11714,#11715,#11716));
#3877=EDGE_LOOP('',(#11717,#11718,#11719,#11720));
#3878=EDGE_LOOP('',(#11721,#11722,#11723,#11724,#11725));
#3879=EDGE_LOOP('',(#11726,#11727,#11728,#11729));
#3880=EDGE_LOOP('',(#11730,#11731,#11732,#11733,#11734,#11735,#11736,#11737,
#11738,#11739,#11740,#11741,#11742,#11743,#11744,#11745,#11746,#11747,#11748,
#11749,#11750,#11751,#11752,#11753,#11754,#11755,#11756,#11757,#11758,#11759,
#11760,#11761,#11762,#11763,#11764,#11765,#11766,#11767,#11768,#11769,#11770));
#3881=EDGE_LOOP('',(#11771,#11772,#11773,#11774,#11775,#11776,#11777,#11778,
#11779,#11780,#11781,#11782,#11783,#11784,#11785,#11786,#11787,#11788,#11789,
#11790,#11791,#11792,#11793,#11794,#11795,#11796,#11797,#11798,#11799,#11800,
#11801,#11802,#11803,#11804,#11805,#11806,#11807,#11808,#11809,#11810,#11811));
#3882=EDGE_LOOP('',(#11812,#11813,#11814,#11815));
#3883=EDGE_LOOP('',(#11816,#11817,#11818,#11819,#11820));
#3884=EDGE_LOOP('',(#11821,#11822,#11823,#11824));
#3885=EDGE_LOOP('',(#11825,#11826,#11827,#11828,#11829,#11830,#11831,#11832,
#11833,#11834,#11835,#11836,#11837,#11838,#11839,#11840,#11841,#11842,#11843,
#11844,#11845,#11846,#11847,#11848,#11849,#11850,#11851,#11852,#11853,#11854,
#11855,#11856,#11857,#11858,#11859,#11860,#11861,#11862,#11863,#11864,#11865));
#3886=EDGE_LOOP('',(#11866,#11867,#11868,#11869,#11870,#11871,#11872,#11873,
#11874,#11875,#11876,#11877,#11878,#11879,#11880,#11881,#11882,#11883,#11884,
#11885,#11886,#11887,#11888,#11889,#11890,#11891,#11892,#11893,#11894,#11895,
#11896,#11897,#11898,#11899,#11900,#11901,#11902,#11903,#11904,#11905,#11906));
#3887=EDGE_LOOP('',(#11907,#11908,#11909,#11910));
#3888=EDGE_LOOP('',(#11911,#11912,#11913,#11914,#11915));
#3889=EDGE_LOOP('',(#11916,#11917,#11918,#11919));
#3890=EDGE_LOOP('',(#11920,#11921,#11922,#11923,#11924,#11925,#11926,#11927,
#11928,#11929,#11930,#11931,#11932,#11933,#11934,#11935,#11936,#11937,#11938,
#11939,#11940,#11941,#11942,#11943,#11944,#11945,#11946,#11947,#11948,#11949,
#11950,#11951,#11952,#11953,#11954,#11955,#11956,#11957,#11958,#11959,#11960));
#3891=EDGE_LOOP('',(#11961,#11962,#11963,#11964,#11965,#11966,#11967,#11968,
#11969,#11970,#11971,#11972,#11973,#11974,#11975,#11976,#11977,#11978,#11979,
#11980,#11981,#11982,#11983,#11984,#11985,#11986,#11987,#11988,#11989,#11990,
#11991,#11992,#11993,#11994,#11995,#11996,#11997,#11998,#11999,#12000,#12001));
#3892=EDGE_LOOP('',(#12002,#12003,#12004,#12005));
#3893=EDGE_LOOP('',(#12006));
#3894=EDGE_LOOP('',(#12007));
#3895=EDGE_LOOP('',(#12008));
#3896=EDGE_LOOP('',(#12009));
#3897=EDGE_LOOP('',(#12010,#12011,#12012,#12013));
#3898=EDGE_LOOP('',(#12014,#12015,#12016,#12017));
#3899=EDGE_LOOP('',(#12018,#12019,#12020,#12021));
#3900=EDGE_LOOP('',(#12022,#12023,#12024,#12025));
#3901=EDGE_LOOP('',(#12026,#12027,#12028,#12029));
#3902=EDGE_LOOP('',(#12030,#12031,#12032,#12033));
#3903=EDGE_LOOP('',(#12034,#12035,#12036,#12037));
#3904=EDGE_LOOP('',(#12038,#12039,#12040,#12041));
#3905=EDGE_LOOP('',(#12042));
#3906=EDGE_LOOP('',(#12043,#12044,#12045,#12046));
#3907=EDGE_LOOP('',(#12047,#12048,#12049,#12050,#12051,#12052,#12053,#12054,
#12055,#12056,#12057,#12058,#12059,#12060,#12061,#12062,#12063,#12064));
#3908=EDGE_LOOP('',(#12065,#12066,#12067,#12068,#12069,#12070,#12071,#12072,
#12073,#12074,#12075,#12076,#12077,#12078,#12079,#12080,#12081));
#3909=EDGE_LOOP('',(#12082,#12083,#12084,#12085));
#3910=EDGE_LOOP('',(#12086,#12087,#12088,#12089));
#3911=EDGE_LOOP('',(#12090,#12091,#12092,#12093));
#3912=EDGE_LOOP('',(#12094,#12095,#12096,#12097));
#3913=EDGE_LOOP('',(#12098,#12099,#12100,#12101));
#3914=EDGE_LOOP('',(#12102,#12103,#12104,#12105));
#3915=EDGE_LOOP('',(#12106,#12107,#12108,#12109));
#3916=EDGE_LOOP('',(#12110,#12111,#12112,#12113,#12114));
#3917=EDGE_LOOP('',(#12115));
#3918=EDGE_LOOP('',(#12116));
#3919=EDGE_LOOP('',(#12117));
#3920=EDGE_LOOP('',(#12118));
#3921=EDGE_LOOP('',(#12119,#12120,#12121,#12122));
#3922=EDGE_LOOP('',(#12123,#12124,#12125,#12126));
#3923=EDGE_LOOP('',(#12127));
#3924=EDGE_LOOP('',(#12128));
#3925=EDGE_LOOP('',(#12129));
#3926=EDGE_LOOP('',(#12130));
#3927=EDGE_LOOP('',(#12131,#12132,#12133,#12134));
#3928=EDGE_LOOP('',(#12135,#12136,#12137,#12138));
#3929=EDGE_LOOP('',(#12139,#12140,#12141,#12142));
#3930=EDGE_LOOP('',(#12143,#12144,#12145,#12146));
#3931=EDGE_LOOP('',(#12147,#12148,#12149,#12150));
#3932=EDGE_LOOP('',(#12151,#12152,#12153,#12154));
#3933=EDGE_LOOP('',(#12155,#12156,#12157,#12158));
#3934=EDGE_LOOP('',(#12159,#12160,#12161,#12162));
#3935=EDGE_LOOP('',(#12163,#12164,#12165,#12166));
#3936=EDGE_LOOP('',(#12167,#12168,#12169,#12170));
#3937=EDGE_LOOP('',(#12171));
#3938=EDGE_LOOP('',(#12172,#12173,#12174,#12175,#12176));
#3939=EDGE_LOOP('',(#12177,#12178,#12179,#12180));
#3940=EDGE_LOOP('',(#12181,#12182,#12183,#12184));
#3941=EDGE_LOOP('',(#12185,#12186,#12187,#12188));
#3942=EDGE_LOOP('',(#12189,#12190,#12191,#12192));
#3943=EDGE_LOOP('',(#12193,#12194,#12195,#12196));
#3944=EDGE_LOOP('',(#12197,#12198,#12199,#12200));
#3945=EDGE_LOOP('',(#12201,#12202,#12203,#12204));
#3946=EDGE_LOOP('',(#12205,#12206,#12207,#12208));
#3947=EDGE_LOOP('',(#12209,#12210,#12211,#12212));
#3948=EDGE_LOOP('',(#12213,#12214,#12215,#12216));
#3949=EDGE_LOOP('',(#12217,#12218,#12219,#12220));
#3950=EDGE_LOOP('',(#12221,#12222,#12223,#12224));
#3951=EDGE_LOOP('',(#12225,#12226,#12227,#12228));
#3952=EDGE_LOOP('',(#12229,#12230,#12231,#12232));
#3953=EDGE_LOOP('',(#12233,#12234,#12235,#12236));
#3954=EDGE_LOOP('',(#12237,#12238,#12239,#12240));
#3955=EDGE_LOOP('',(#12241,#12242,#12243,#12244));
#3956=EDGE_LOOP('',(#12245,#12246,#12247,#12248,#12249));
#3957=EDGE_LOOP('',(#12250,#12251,#12252,#12253));
#3958=EDGE_LOOP('',(#12254,#12255,#12256,#12257));
#3959=EDGE_LOOP('',(#12258,#12259,#12260,#12261));
#3960=EDGE_LOOP('',(#12262,#12263,#12264,#12265));
#3961=EDGE_LOOP('',(#12266,#12267,#12268,#12269));
#3962=EDGE_LOOP('',(#12270,#12271,#12272,#12273));
#3963=EDGE_LOOP('',(#12274,#12275,#12276,#12277));
#3964=EDGE_LOOP('',(#12278,#12279,#12280,#12281));
#3965=EDGE_LOOP('',(#12282,#12283,#12284,#12285));
#3966=EDGE_LOOP('',(#12286,#12287,#12288,#12289));
#3967=EDGE_LOOP('',(#12290,#12291,#12292,#12293));
#3968=EDGE_LOOP('',(#12294,#12295,#12296,#12297));
#3969=EDGE_LOOP('',(#12298,#12299,#12300,#12301));
#3970=EDGE_LOOP('',(#12302,#12303,#12304,#12305));
#3971=EDGE_LOOP('',(#12306,#12307,#12308,#12309));
#3972=EDGE_LOOP('',(#12310,#12311,#12312,#12313));
#3973=EDGE_LOOP('',(#12314,#12315,#12316,#12317,#12318));
#3974=EDGE_LOOP('',(#12319,#12320,#12321,#12322));
#3975=EDGE_LOOP('',(#12323));
#3976=EDGE_LOOP('',(#12324));
#3977=EDGE_LOOP('',(#12325));
#3978=EDGE_LOOP('',(#12326));
#3979=EDGE_LOOP('',(#12327,#12328,#12329,#12330));
#3980=EDGE_LOOP('',(#12331,#12332,#12333,#12334));
#3981=EDGE_LOOP('',(#12335,#12336,#12337,#12338));
#3982=EDGE_LOOP('',(#12339,#12340,#12341,#12342));
#3983=EDGE_LOOP('',(#12343,#12344,#12345,#12346));
#3984=EDGE_LOOP('',(#12347));
#3985=EDGE_LOOP('',(#12348,#12349,#12350,#12351,#12352));
#3986=EDGE_LOOP('',(#12353,#12354,#12355,#12356,#12357,#12358,#12359,#12360,
#12361,#12362,#12363,#12364,#12365,#12366,#12367,#12368,#12369,#12370,#12371,
#12372,#12373,#12374,#12375,#12376,#12377,#12378,#12379,#12380,#12381,#12382,
#12383,#12384,#12385,#12386,#12387,#12388,#12389,#12390,#12391,#12392));
#3987=EDGE_LOOP('',(#12393,#12394,#12395,#12396));
#3988=EDGE_LOOP('',(#12397,#12398,#12399,#12400,#12401,#12402,#12403,#12404,
#12405,#12406,#12407,#12408,#12409,#12410,#12411,#12412,#12413,#12414,#12415,
#12416,#12417,#12418,#12419,#12420,#12421,#12422,#12423,#12424,#12425,#12426,
#12427,#12428,#12429,#12430,#12431,#12432,#12433,#12434,#12435,#12436));
#3989=EDGE_LOOP('',(#12437,#12438,#12439,#12440));
#3990=EDGE_LOOP('',(#12441,#12442,#12443,#12444));
#3991=EDGE_LOOP('',(#12445,#12446,#12447,#12448));
#3992=EDGE_LOOP('',(#12449,#12450,#12451,#12452,#12453,#12454,#12455,#12456));
#3993=EDGE_LOOP('',(#12457));
#3994=EDGE_LOOP('',(#12458,#12459,#12460,#12461,#12462,#12463,#12464,#12465));
#3995=EDGE_LOOP('',(#12466));
#3996=EDGE_LOOP('',(#12467));
#3997=EDGE_LOOP('',(#12468));
#3998=EDGE_LOOP('',(#12469));
#3999=EDGE_LOOP('',(#12470));
#4000=EDGE_LOOP('',(#12471,#12472,#12473,#12474));
#4001=EDGE_LOOP('',(#12475,#12476,#12477,#12478));
#4002=EDGE_LOOP('',(#12479));
#4003=EDGE_LOOP('',(#12480));
#4004=EDGE_LOOP('',(#12481,#12482,#12483,#12484));
#4005=EDGE_LOOP('',(#12485,#12486,#12487,#12488,#12489));
#4006=EDGE_LOOP('',(#12490));
#4007=EDGE_LOOP('',(#12491));
#4008=EDGE_LOOP('',(#12492,#12493,#12494,#12495));
#4009=EDGE_LOOP('',(#12496,#12497,#12498,#12499));
#4010=EDGE_LOOP('',(#12500,#12501,#12502,#12503));
#4011=EDGE_LOOP('',(#12504));
#4012=EDGE_LOOP('',(#12505));
#4013=EDGE_LOOP('',(#12506));
#4014=EDGE_LOOP('',(#12507));
#4015=EDGE_LOOP('',(#12508,#12509,#12510,#12511));
#4016=EDGE_LOOP('',(#12512,#12513,#12514,#12515));
#4017=EDGE_LOOP('',(#12516));
#4018=EDGE_LOOP('',(#12517));
#4019=EDGE_LOOP('',(#12518));
#4020=EDGE_LOOP('',(#12519));
#4021=EDGE_LOOP('',(#12520,#12521,#12522,#12523));
#4022=EDGE_LOOP('',(#12524,#12525,#12526,#12527));
#4023=EDGE_LOOP('',(#12528,#12529,#12530,#12531));
#4024=EDGE_LOOP('',(#12532,#12533,#12534,#12535));
#4025=EDGE_LOOP('',(#12536,#12537,#12538,#12539));
#4026=EDGE_LOOP('',(#12540,#12541,#12542,#12543));
#4027=EDGE_LOOP('',(#12544,#12545,#12546,#12547));
#4028=EDGE_LOOP('',(#12548,#12549,#12550,#12551));
#4029=EDGE_LOOP('',(#12552,#12553,#12554,#12555));
#4030=EDGE_LOOP('',(#12556,#12557,#12558,#12559));
#4031=EDGE_LOOP('',(#12560,#12561,#12562,#12563));
#4032=EDGE_LOOP('',(#12564,#12565,#12566,#12567));
#4033=EDGE_LOOP('',(#12568,#12569,#12570,#12571));
#4034=EDGE_LOOP('',(#12572,#12573,#12574,#12575));
#4035=EDGE_LOOP('',(#12576,#12577,#12578,#12579));
#4036=EDGE_LOOP('',(#12580,#12581,#12582,#12583));
#4037=EDGE_LOOP('',(#12584,#12585,#12586,#12587));
#4038=EDGE_LOOP('',(#12588,#12589,#12590,#12591));
#4039=EDGE_LOOP('',(#12592,#12593,#12594,#12595));
#4040=EDGE_LOOP('',(#12596,#12597,#12598,#12599));
#4041=EDGE_LOOP('',(#12600,#12601,#12602,#12603));
#4042=EDGE_LOOP('',(#12604,#12605,#12606,#12607));
#4043=EDGE_LOOP('',(#12608,#12609,#12610,#12611));
#4044=EDGE_LOOP('',(#12612,#12613,#12614,#12615));
#4045=EDGE_LOOP('',(#12616,#12617,#12618,#12619));
#4046=EDGE_LOOP('',(#12620,#12621,#12622,#12623));
#4047=EDGE_LOOP('',(#12624,#12625,#12626,#12627));
#4048=EDGE_LOOP('',(#12628,#12629,#12630,#12631));
#4049=EDGE_LOOP('',(#12632,#12633,#12634,#12635));
#4050=EDGE_LOOP('',(#12636,#12637,#12638,#12639));
#4051=EDGE_LOOP('',(#12640,#12641,#12642,#12643));
#4052=EDGE_LOOP('',(#12644,#12645,#12646,#12647));
#4053=EDGE_LOOP('',(#12648,#12649,#12650,#12651));
#4054=EDGE_LOOP('',(#12652,#12653,#12654,#12655));
#4055=EDGE_LOOP('',(#12656,#12657,#12658,#12659));
#4056=EDGE_LOOP('',(#12660,#12661,#12662,#12663));
#4057=EDGE_LOOP('',(#12664,#12665,#12666,#12667));
#4058=EDGE_LOOP('',(#12668,#12669,#12670,#12671));
#4059=EDGE_LOOP('',(#12672,#12673,#12674,#12675));
#4060=EDGE_LOOP('',(#12676,#12677,#12678,#12679));
#4061=EDGE_LOOP('',(#12680,#12681,#12682,#12683));
#4062=EDGE_LOOP('',(#12684,#12685,#12686,#12687));
#4063=EDGE_LOOP('',(#12688,#12689,#12690,#12691));
#4064=EDGE_LOOP('',(#12692,#12693,#12694,#12695));
#4065=EDGE_LOOP('',(#12696,#12697,#12698,#12699));
#4066=EDGE_LOOP('',(#12700,#12701,#12702,#12703));
#4067=EDGE_LOOP('',(#12704,#12705,#12706,#12707));
#4068=EDGE_LOOP('',(#12708,#12709,#12710,#12711));
#4069=EDGE_LOOP('',(#12712,#12713,#12714,#12715));
#4070=EDGE_LOOP('',(#12716,#12717,#12718,#12719));
#4071=EDGE_LOOP('',(#12720,#12721,#12722,#12723));
#4072=EDGE_LOOP('',(#12724,#12725,#12726,#12727));
#4073=EDGE_LOOP('',(#12728,#12729,#12730,#12731));
#4074=EDGE_LOOP('',(#12732,#12733,#12734,#12735));
#4075=EDGE_LOOP('',(#12736,#12737,#12738,#12739));
#4076=EDGE_LOOP('',(#12740,#12741,#12742,#12743));
#4077=EDGE_LOOP('',(#12744,#12745,#12746,#12747));
#4078=EDGE_LOOP('',(#12748,#12749,#12750,#12751));
#4079=EDGE_LOOP('',(#12752,#12753,#12754,#12755));
#4080=EDGE_LOOP('',(#12756,#12757,#12758,#12759));
#4081=EDGE_LOOP('',(#12760,#12761,#12762,#12763));
#4082=EDGE_LOOP('',(#12764,#12765,#12766,#12767));
#4083=EDGE_LOOP('',(#12768,#12769,#12770,#12771));
#4084=EDGE_LOOP('',(#12772,#12773,#12774,#12775));
#4085=EDGE_LOOP('',(#12776,#12777,#12778,#12779));
#4086=EDGE_LOOP('',(#12780,#12781,#12782,#12783));
#4087=EDGE_LOOP('',(#12784,#12785,#12786,#12787));
#4088=EDGE_LOOP('',(#12788,#12789,#12790,#12791));
#4089=EDGE_LOOP('',(#12792,#12793,#12794,#12795));
#4090=EDGE_LOOP('',(#12796,#12797,#12798,#12799));
#4091=EDGE_LOOP('',(#12800,#12801,#12802,#12803));
#4092=EDGE_LOOP('',(#12804,#12805,#12806,#12807));
#4093=EDGE_LOOP('',(#12808,#12809,#12810,#12811));
#4094=EDGE_LOOP('',(#12812,#12813,#12814,#12815));
#4095=EDGE_LOOP('',(#12816,#12817,#12818,#12819));
#4096=EDGE_LOOP('',(#12820,#12821,#12822,#12823));
#4097=EDGE_LOOP('',(#12824,#12825,#12826,#12827));
#4098=EDGE_LOOP('',(#12828,#12829,#12830,#12831));
#4099=EDGE_LOOP('',(#12832,#12833,#12834,#12835));
#4100=EDGE_LOOP('',(#12836,#12837,#12838,#12839));
#4101=EDGE_LOOP('',(#12840,#12841,#12842,#12843));
#4102=EDGE_LOOP('',(#12844,#12845,#12846,#12847));
#4103=EDGE_LOOP('',(#12848,#12849,#12850,#12851));
#4104=EDGE_LOOP('',(#12852,#12853,#12854,#12855));
#4105=EDGE_LOOP('',(#12856,#12857,#12858,#12859));
#4106=EDGE_LOOP('',(#12860,#12861,#12862,#12863));
#4107=EDGE_LOOP('',(#12864,#12865,#12866,#12867));
#4108=EDGE_LOOP('',(#12868,#12869,#12870,#12871));
#4109=EDGE_LOOP('',(#12872,#12873,#12874,#12875));
#4110=EDGE_LOOP('',(#12876,#12877,#12878,#12879));
#4111=EDGE_LOOP('',(#12880,#12881,#12882,#12883,#12884,#12885,#12886,#12887));
#4112=EDGE_LOOP('',(#12888,#12889,#12890,#12891));
#4113=EDGE_LOOP('',(#12892,#12893,#12894,#12895));
#4114=EDGE_LOOP('',(#12896,#12897,#12898,#12899));
#4115=EDGE_LOOP('',(#12900,#12901,#12902,#12903));
#4116=EDGE_LOOP('',(#12904,#12905,#12906,#12907));
#4117=EDGE_LOOP('',(#12908,#12909,#12910,#12911));
#4118=EDGE_LOOP('',(#12912,#12913,#12914,#12915));
#4119=EDGE_LOOP('',(#12916,#12917,#12918,#12919));
#4120=EDGE_LOOP('',(#12920,#12921,#12922,#12923));
#4121=EDGE_LOOP('',(#12924,#12925,#12926,#12927));
#4122=EDGE_LOOP('',(#12928,#12929,#12930,#12931));
#4123=EDGE_LOOP('',(#12932,#12933,#12934,#12935));
#4124=EDGE_LOOP('',(#12936,#12937,#12938,#12939));
#4125=EDGE_LOOP('',(#12940,#12941,#12942,#12943));
#4126=EDGE_LOOP('',(#12944,#12945,#12946,#12947));
#4127=EDGE_LOOP('',(#12948,#12949,#12950,#12951));
#4128=EDGE_LOOP('',(#12952,#12953,#12954,#12955));
#4129=EDGE_LOOP('',(#12956,#12957,#12958,#12959));
#4130=EDGE_LOOP('',(#12960,#12961,#12962,#12963));
#4131=EDGE_LOOP('',(#12964,#12965,#12966,#12967));
#4132=EDGE_LOOP('',(#12968,#12969,#12970,#12971));
#4133=EDGE_LOOP('',(#12972,#12973,#12974,#12975));
#4134=EDGE_LOOP('',(#12976,#12977,#12978,#12979));
#4135=EDGE_LOOP('',(#12980,#12981,#12982,#12983));
#4136=EDGE_LOOP('',(#12984,#12985,#12986,#12987));
#4137=EDGE_LOOP('',(#12988,#12989,#12990,#12991));
#4138=EDGE_LOOP('',(#12992,#12993,#12994,#12995));
#4139=EDGE_LOOP('',(#12996,#12997,#12998,#12999));
#4140=EDGE_LOOP('',(#13000,#13001,#13002,#13003));
#4141=EDGE_LOOP('',(#13004,#13005,#13006,#13007));
#4142=EDGE_LOOP('',(#13008,#13009,#13010,#13011));
#4143=EDGE_LOOP('',(#13012,#13013,#13014,#13015));
#4144=EDGE_LOOP('',(#13016,#13017,#13018,#13019));
#4145=EDGE_LOOP('',(#13020,#13021,#13022,#13023));
#4146=EDGE_LOOP('',(#13024,#13025,#13026,#13027));
#4147=EDGE_LOOP('',(#13028,#13029,#13030,#13031));
#4148=EDGE_LOOP('',(#13032,#13033,#13034,#13035));
#4149=EDGE_LOOP('',(#13036,#13037,#13038,#13039));
#4150=EDGE_LOOP('',(#13040,#13041,#13042,#13043));
#4151=EDGE_LOOP('',(#13044,#13045,#13046,#13047));
#4152=EDGE_LOOP('',(#13048,#13049,#13050,#13051));
#4153=EDGE_LOOP('',(#13052,#13053,#13054,#13055));
#4154=EDGE_LOOP('',(#13056,#13057,#13058,#13059));
#4155=EDGE_LOOP('',(#13060,#13061,#13062,#13063));
#4156=EDGE_LOOP('',(#13064,#13065,#13066,#13067));
#4157=EDGE_LOOP('',(#13068,#13069,#13070,#13071));
#4158=EDGE_LOOP('',(#13072,#13073,#13074,#13075));
#4159=EDGE_LOOP('',(#13076,#13077,#13078,#13079));
#4160=EDGE_LOOP('',(#13080,#13081,#13082,#13083));
#4161=EDGE_LOOP('',(#13084,#13085,#13086,#13087));
#4162=EDGE_LOOP('',(#13088,#13089,#13090,#13091));
#4163=EDGE_LOOP('',(#13092,#13093,#13094,#13095));
#4164=EDGE_LOOP('',(#13096,#13097,#13098,#13099));
#4165=EDGE_LOOP('',(#13100,#13101,#13102,#13103));
#4166=EDGE_LOOP('',(#13104,#13105,#13106,#13107));
#4167=EDGE_LOOP('',(#13108,#13109,#13110,#13111));
#4168=EDGE_LOOP('',(#13112,#13113,#13114,#13115));
#4169=EDGE_LOOP('',(#13116,#13117,#13118,#13119));
#4170=EDGE_LOOP('',(#13120,#13121,#13122,#13123));
#4171=EDGE_LOOP('',(#13124,#13125,#13126,#13127));
#4172=EDGE_LOOP('',(#13128,#13129,#13130,#13131));
#4173=EDGE_LOOP('',(#13132,#13133,#13134,#13135));
#4174=EDGE_LOOP('',(#13136,#13137,#13138,#13139));
#4175=EDGE_LOOP('',(#13140,#13141,#13142,#13143));
#4176=EDGE_LOOP('',(#13144,#13145,#13146,#13147));
#4177=EDGE_LOOP('',(#13148,#13149,#13150,#13151));
#4178=EDGE_LOOP('',(#13152,#13153,#13154,#13155));
#4179=EDGE_LOOP('',(#13156,#13157,#13158,#13159));
#4180=EDGE_LOOP('',(#13160,#13161,#13162,#13163));
#4181=EDGE_LOOP('',(#13164,#13165,#13166,#13167));
#4182=EDGE_LOOP('',(#13168,#13169,#13170,#13171));
#4183=EDGE_LOOP('',(#13172,#13173,#13174,#13175));
#4184=EDGE_LOOP('',(#13176,#13177,#13178,#13179));
#4185=EDGE_LOOP('',(#13180,#13181,#13182,#13183));
#4186=EDGE_LOOP('',(#13184,#13185,#13186,#13187));
#4187=EDGE_LOOP('',(#13188,#13189,#13190,#13191));
#4188=EDGE_LOOP('',(#13192,#13193,#13194,#13195));
#4189=EDGE_LOOP('',(#13196,#13197,#13198,#13199));
#4190=EDGE_LOOP('',(#13200,#13201,#13202,#13203));
#4191=EDGE_LOOP('',(#13204,#13205,#13206,#13207));
#4192=EDGE_LOOP('',(#13208,#13209,#13210,#13211));
#4193=EDGE_LOOP('',(#13212,#13213,#13214,#13215));
#4194=EDGE_LOOP('',(#13216,#13217,#13218,#13219));
#4195=EDGE_LOOP('',(#13220));
#4196=EDGE_LOOP('',(#13221));
#4197=EDGE_LOOP('',(#13222));
#4198=EDGE_LOOP('',(#13223));
#4199=EDGE_LOOP('',(#13224,#13225,#13226,#13227));
#4200=EDGE_LOOP('',(#13228,#13229,#13230,#13231,#13232));
#4201=EDGE_LOOP('',(#13233,#13234,#13235,#13236,#13237,#13238,#13239,#13240,
#13241,#13242,#13243,#13244,#13245,#13246,#13247,#13248,#13249,#13250,#13251,
#13252,#13253,#13254,#13255,#13256,#13257,#13258,#13259,#13260,#13261,#13262,
#13263,#13264,#13265,#13266,#13267,#13268,#13269,#13270,#13271,#13272,#13273,
#13274,#13275,#13276,#13277,#13278,#13279,#13280,#13281,#13282,#13283,#13284,
#13285,#13286,#13287,#13288,#13289,#13290,#13291,#13292,#13293,#13294,#13295,
#13296,#13297,#13298,#13299,#13300,#13301,#13302,#13303,#13304,#13305,#13306,
#13307,#13308,#13309,#13310,#13311,#13312,#13313,#13314,#13315,#13316,#13317,
#13318,#13319,#13320,#13321,#13322,#13323,#13324,#13325,#13326,#13327,#13328,
#13329,#13330,#13331,#13332,#13333,#13334,#13335,#13336,#13337,#13338,#13339,
#13340,#13341,#13342,#13343,#13344,#13345,#13346,#13347,#13348,#13349,#13350,
#13351,#13352,#13353,#13354,#13355,#13356,#13357,#13358,#13359,#13360,#13361,
#13362,#13363,#13364,#13365,#13366,#13367,#13368,#13369,#13370,#13371,#13372,
#13373,#13374,#13375,#13376,#13377,#13378,#13379,#13380,#13381,#13382,#13383,
#13384,#13385,#13386,#13387,#13388,#13389,#13390,#13391,#13392,#13393,#13394,
#13395,#13396));
#4202=EDGE_LOOP('',(#13397,#13398,#13399,#13400));
#4203=EDGE_LOOP('',(#13401,#13402,#13403,#13404,#13405,#13406,#13407,#13408,
#13409,#13410,#13411,#13412,#13413,#13414,#13415,#13416,#13417,#13418,#13419,
#13420,#13421,#13422,#13423,#13424,#13425,#13426,#13427,#13428,#13429,#13430,
#13431,#13432,#13433,#13434,#13435,#13436,#13437,#13438,#13439,#13440,#13441,
#13442,#13443,#13444,#13445,#13446,#13447,#13448,#13449,#13450,#13451,#13452,
#13453,#13454,#13455,#13456,#13457,#13458,#13459,#13460,#13461,#13462,#13463,
#13464,#13465,#13466,#13467,#13468,#13469,#13470,#13471,#13472,#13473,#13474,
#13475,#13476,#13477,#13478,#13479,#13480,#13481,#13482,#13483,#13484,#13485,
#13486,#13487,#13488,#13489,#13490,#13491,#13492,#13493,#13494,#13495,#13496,
#13497,#13498,#13499,#13500,#13501,#13502,#13503,#13504,#13505,#13506,#13507,
#13508,#13509,#13510,#13511,#13512,#13513,#13514,#13515,#13516,#13517,#13518,
#13519,#13520,#13521,#13522,#13523,#13524,#13525,#13526,#13527,#13528,#13529,
#13530,#13531,#13532,#13533,#13534,#13535,#13536,#13537,#13538,#13539,#13540,
#13541,#13542,#13543,#13544,#13545,#13546,#13547,#13548,#13549,#13550,#13551,
#13552,#13553,#13554,#13555,#13556,#13557,#13558,#13559,#13560,#13561,#13562,
#13563,#13564));
#4204=EDGE_LOOP('',(#13565,#13566,#13567,#13568));
#4205=EDGE_LOOP('',(#13569,#13570,#13571,#13572));
#4206=EDGE_LOOP('',(#13573,#13574,#13575,#13576));
#4207=EDGE_LOOP('',(#13577,#13578,#13579,#13580));
#4208=EDGE_LOOP('',(#13581,#13582,#13583,#13584));
#4209=EDGE_LOOP('',(#13585,#13586,#13587,#13588));
#4210=EDGE_LOOP('',(#13589,#13590,#13591,#13592));
#4211=EDGE_LOOP('',(#13593));
#4212=EDGE_LOOP('',(#13594));
#4213=EDGE_LOOP('',(#13595));
#4214=EDGE_LOOP('',(#13596));
#4215=EDGE_LOOP('',(#13597));
#4216=EDGE_LOOP('',(#13598));
#4217=EDGE_LOOP('',(#13599));
#4218=EDGE_LOOP('',(#13600));
#4219=EDGE_LOOP('',(#13601,#13602,#13603,#13604));
#4220=EDGE_LOOP('',(#13605));
#4221=EDGE_LOOP('',(#13606));
#4222=EDGE_LOOP('',(#13607));
#4223=EDGE_LOOP('',(#13608));
#4224=EDGE_LOOP('',(#13609));
#4225=EDGE_LOOP('',(#13610));
#4226=EDGE_LOOP('',(#13611));
#4227=EDGE_LOOP('',(#13612));
#4228=EDGE_LOOP('',(#13613));
#4229=EDGE_LOOP('',(#13614,#13615,#13616,#13617));
#4230=EDGE_LOOP('',(#13618,#13619,#13620,#13621));
#4231=EDGE_LOOP('',(#13622,#13623,#13624,#13625));
#4232=EDGE_LOOP('',(#13626));
#4233=EDGE_LOOP('',(#13627));
#4234=EDGE_LOOP('',(#13628));
#4235=EDGE_LOOP('',(#13629));
#4236=EDGE_LOOP('',(#13630,#13631,#13632,#13633));
#4237=EDGE_LOOP('',(#13634,#13635,#13636,#13637));
#4238=EDGE_LOOP('',(#13638,#13639,#13640,#13641));
#4239=EDGE_LOOP('',(#13642,#13643,#13644,#13645));
#4240=EDGE_LOOP('',(#13646,#13647,#13648,#13649));
#4241=EDGE_LOOP('',(#13650,#13651,#13652,#13653));
#4242=EDGE_LOOP('',(#13654,#13655,#13656,#13657));
#4243=EDGE_LOOP('',(#13658,#13659,#13660,#13661));
#4244=EDGE_LOOP('',(#13662,#13663,#13664,#13665));
#4245=EDGE_LOOP('',(#13666,#13667,#13668,#13669));
#4246=EDGE_LOOP('',(#13670,#13671,#13672,#13673));
#4247=EDGE_LOOP('',(#13674,#13675,#13676,#13677));
#4248=EDGE_LOOP('',(#13678,#13679,#13680,#13681));
#4249=EDGE_LOOP('',(#13682,#13683,#13684,#13685));
#4250=EDGE_LOOP('',(#13686,#13687,#13688,#13689));
#4251=EDGE_LOOP('',(#13690,#13691,#13692,#13693));
#4252=EDGE_LOOP('',(#13694,#13695,#13696,#13697));
#4253=EDGE_LOOP('',(#13698,#13699,#13700,#13701));
#4254=EDGE_LOOP('',(#13702,#13703,#13704,#13705));
#4255=EDGE_LOOP('',(#13706,#13707,#13708,#13709));
#4256=EDGE_LOOP('',(#13710,#13711,#13712,#13713));
#4257=EDGE_LOOP('',(#13714,#13715,#13716,#13717));
#4258=EDGE_LOOP('',(#13718,#13719,#13720,#13721));
#4259=EDGE_LOOP('',(#13722,#13723,#13724,#13725));
#4260=EDGE_LOOP('',(#13726,#13727,#13728,#13729));
#4261=EDGE_LOOP('',(#13730,#13731,#13732,#13733));
#4262=EDGE_LOOP('',(#13734,#13735,#13736,#13737));
#4263=EDGE_LOOP('',(#13738,#13739,#13740,#13741));
#4264=EDGE_LOOP('',(#13742,#13743,#13744,#13745));
#4265=EDGE_LOOP('',(#13746,#13747,#13748,#13749));
#4266=EDGE_LOOP('',(#13750,#13751,#13752,#13753));
#4267=EDGE_LOOP('',(#13754,#13755,#13756,#13757));
#4268=EDGE_LOOP('',(#13758,#13759,#13760,#13761));
#4269=EDGE_LOOP('',(#13762,#13763,#13764,#13765));
#4270=EDGE_LOOP('',(#13766,#13767,#13768,#13769));
#4271=EDGE_LOOP('',(#13770,#13771,#13772,#13773));
#4272=EDGE_LOOP('',(#13774,#13775,#13776,#13777));
#4273=EDGE_LOOP('',(#13778,#13779,#13780,#13781));
#4274=EDGE_LOOP('',(#13782,#13783,#13784,#13785));
#4275=EDGE_LOOP('',(#13786,#13787,#13788,#13789));
#4276=EDGE_LOOP('',(#13790,#13791,#13792,#13793));
#4277=EDGE_LOOP('',(#13794,#13795,#13796,#13797));
#4278=EDGE_LOOP('',(#13798,#13799,#13800,#13801));
#4279=EDGE_LOOP('',(#13802,#13803,#13804,#13805));
#4280=EDGE_LOOP('',(#13806,#13807,#13808,#13809));
#4281=EDGE_LOOP('',(#13810,#13811,#13812,#13813));
#4282=EDGE_LOOP('',(#13814,#13815,#13816,#13817));
#4283=EDGE_LOOP('',(#13818,#13819,#13820,#13821));
#4284=EDGE_LOOP('',(#13822,#13823,#13824,#13825,#13826,#13827));
#4285=EDGE_LOOP('',(#13828,#13829,#13830,#13831,#13832,#13833,#13834,#13835,
#13836,#13837,#13838,#13839,#13840,#13841,#13842,#13843,#13844,#13845,#13846,
#13847,#13848,#13849,#13850,#13851,#13852,#13853,#13854,#13855,#13856,#13857,
#13858,#13859,#13860,#13861,#13862,#13863,#13864,#13865,#13866,#13867));
#4286=EDGE_LOOP('',(#13868,#13869,#13870,#13871));
#4287=EDGE_LOOP('',(#13872,#13873,#13874,#13875,#13876,#13877,#13878,#13879,
#13880,#13881,#13882,#13883,#13884,#13885,#13886,#13887,#13888,#13889,#13890,
#13891,#13892,#13893,#13894,#13895,#13896,#13897,#13898,#13899,#13900,#13901,
#13902,#13903,#13904,#13905,#13906,#13907,#13908,#13909,#13910,#13911));
#4288=EDGE_LOOP('',(#13912,#13913,#13914,#13915));
#4289=EDGE_LOOP('',(#13916,#13917,#13918,#13919));
#4290=EDGE_LOOP('',(#13920,#13921,#13922,#13923));
#4291=EDGE_LOOP('',(#13924,#13925,#13926,#13927,#13928,#13929));
#4292=EDGE_LOOP('',(#13930));
#4293=EDGE_LOOP('',(#13931));
#4294=EDGE_LOOP('',(#13932,#13933,#13934,#13935));
#4295=EDGE_LOOP('',(#13936,#13937,#13938,#13939));
#4296=EDGE_LOOP('',(#13940));
#4297=EDGE_LOOP('',(#13941));
#4298=EDGE_LOOP('',(#13942,#13943,#13944,#13945));
#4299=EDGE_LOOP('',(#13946,#13947,#13948,#13949));
#4300=EDGE_LOOP('',(#13950));
#4301=EDGE_LOOP('',(#13951));
#4302=EDGE_LOOP('',(#13952,#13953,#13954,#13955));
#4303=EDGE_LOOP('',(#13956,#13957,#13958,#13959));
#4304=EDGE_LOOP('',(#13960));
#4305=EDGE_LOOP('',(#13961));
#4306=EDGE_LOOP('',(#13962,#13963,#13964,#13965));
#4307=EDGE_LOOP('',(#13966,#13967,#13968,#13969));
#4308=EDGE_LOOP('',(#13970,#13971,#13972,#13973));
#4309=EDGE_LOOP('',(#13974,#13975,#13976,#13977));
#4310=EDGE_LOOP('',(#13978));
#4311=EDGE_LOOP('',(#13979));
#4312=EDGE_LOOP('',(#13980));
#4313=EDGE_LOOP('',(#13981));
#4314=EDGE_LOOP('',(#13982));
#4315=EDGE_LOOP('',(#13983));
#4316=EDGE_LOOP('',(#13984));
#4317=EDGE_LOOP('',(#13985));
#4318=EDGE_LOOP('',(#13986));
#4319=EDGE_LOOP('',(#13987));
#4320=EDGE_LOOP('',(#13988));
#4321=EDGE_LOOP('',(#13989));
#4322=EDGE_LOOP('',(#13990,#13991,#13992,#13993));
#4323=EDGE_LOOP('',(#13994,#13995,#13996,#13997));
#4324=EDGE_LOOP('',(#13998,#13999,#14000,#14001));
#4325=EDGE_LOOP('',(#14002,#14003,#14004,#14005));
#4326=EDGE_LOOP('',(#14006));
#4327=EDGE_LOOP('',(#14007));
#4328=EDGE_LOOP('',(#14008));
#4329=EDGE_LOOP('',(#14009));
#4330=EDGE_LOOP('',(#14010,#14011,#14012,#14013));
#4331=EDGE_LOOP('',(#14014,#14015,#14016,#14017));
#4332=EDGE_LOOP('',(#14018,#14019,#14020,#14021));
#4333=EDGE_LOOP('',(#14022,#14023,#14024,#14025));
#4334=EDGE_LOOP('',(#14026));
#4335=EDGE_LOOP('',(#14027));
#4336=EDGE_LOOP('',(#14028));
#4337=EDGE_LOOP('',(#14029));
#4338=EDGE_LOOP('',(#14030,#14031));
#4339=EDGE_LOOP('',(#14032,#14033,#14034,#14035,#14036,#14037,#14038));
#4340=EDGE_LOOP('',(#14039,#14040,#14041,#14042,#14043,#14044,#14045,#14046,
#14047,#14048,#14049,#14050,#14051,#14052,#14053,#14054,#14055,#14056,#14057,
#14058,#14059,#14060,#14061,#14062,#14063,#14064,#14065,#14066,#14067,#14068,
#14069,#14070,#14071));
#4341=EDGE_LOOP('',(#14072,#14073,#14074,#14075));
#4342=EDGE_LOOP('',(#14076,#14077,#14078,#14079,#14080,#14081,#14082));
#4343=EDGE_LOOP('',(#14083,#14084,#14085,#14086));
#4344=EDGE_LOOP('',(#14087,#14088,#14089,#14090,#14091,#14092,#14093));
#4345=EDGE_LOOP('',(#14094,#14095,#14096,#14097,#14098));
#4346=EDGE_LOOP('',(#14099,#14100,#14101,#14102,#14103,#14104,#14105));
#4347=EDGE_LOOP('',(#14106,#14107,#14108,#14109));
#4348=EDGE_LOOP('',(#14110,#14111,#14112,#14113,#14114,#14115,#14116));
#4349=EDGE_LOOP('',(#14117,#14118,#14119,#14120));
#4350=EDGE_LOOP('',(#14121,#14122,#14123,#14124,#14125,#14126,#14127,#14128));
#4351=EDGE_LOOP('',(#14129,#14130,#14131,#14132));
#4352=EDGE_LOOP('',(#14133,#14134,#14135,#14136,#14137,#14138,#14139));
#4353=EDGE_LOOP('',(#14140,#14141,#14142,#14143));
#4354=EDGE_LOOP('',(#14144,#14145,#14146,#14147,#14148,#14149,#14150));
#4355=EDGE_LOOP('',(#14151,#14152,#14153,#14154,#14155));
#4356=EDGE_LOOP('',(#14156,#14157,#14158,#14159,#14160,#14161,#14162));
#4357=EDGE_LOOP('',(#14163,#14164,#14165,#14166));
#4358=EDGE_LOOP('',(#14167,#14168,#14169,#14170,#14171,#14172,#14173));
#4359=EDGE_LOOP('',(#14174,#14175,#14176,#14177));
#4360=EDGE_LOOP('',(#14178,#14179,#14180,#14181,#14182,#14183,#14184));
#4361=EDGE_LOOP('',(#14185,#14186,#14187,#14188));
#4362=EDGE_LOOP('',(#14189,#14190,#14191,#14192,#14193,#14194,#14195));
#4363=EDGE_LOOP('',(#14196,#14197,#14198,#14199,#14200,#14201,#14202,#14203,
#14204,#14205,#14206,#14207,#14208,#14209,#14210,#14211,#14212,#14213,#14214,
#14215,#14216,#14217,#14218,#14219,#14220,#14221,#14222,#14223,#14224,#14225,
#14226,#14227));
#4364=EDGE_LOOP('',(#14228));
#4365=EDGE_LOOP('',(#14229));
#4366=EDGE_LOOP('',(#14230,#14231,#14232,#14233));
#4367=EDGE_LOOP('',(#14234,#14235,#14236,#14237));
#4368=EDGE_LOOP('',(#14238,#14239,#14240,#14241));
#4369=EDGE_LOOP('',(#14242));
#4370=EDGE_LOOP('',(#14243));
#4371=EDGE_LOOP('',(#14244));
#4372=EDGE_LOOP('',(#14245));
#4373=EDGE_LOOP('',(#14246,#14247,#14248,#14249));
#4374=EDGE_LOOP('',(#14250,#14251,#14252,#14253));
#4375=EDGE_LOOP('',(#14254,#14255,#14256,#14257));
#4376=EDGE_LOOP('',(#14258,#14259,#14260,#14261));
#4377=EDGE_LOOP('',(#14262,#14263,#14264,#14265));
#4378=EDGE_LOOP('',(#14266,#14267,#14268,#14269));
#4379=EDGE_LOOP('',(#14270,#14271,#14272,#14273));
#4380=EDGE_LOOP('',(#14274,#14275,#14276,#14277));
#4381=EDGE_LOOP('',(#14278,#14279,#14280,#14281));
#4382=EDGE_LOOP('',(#14282,#14283,#14284,#14285));
#4383=EDGE_LOOP('',(#14286,#14287,#14288,#14289));
#4384=EDGE_LOOP('',(#14290,#14291,#14292,#14293));
#4385=EDGE_LOOP('',(#14294,#14295,#14296,#14297));
#4386=EDGE_LOOP('',(#14298,#14299,#14300,#14301));
#4387=EDGE_LOOP('',(#14302,#14303,#14304,#14305));
#4388=EDGE_LOOP('',(#14306,#14307,#14308,#14309));
#4389=EDGE_LOOP('',(#14310,#14311,#14312,#14313));
#4390=EDGE_LOOP('',(#14314,#14315,#14316,#14317));
#4391=EDGE_LOOP('',(#14318,#14319,#14320,#14321));
#4392=EDGE_LOOP('',(#14322,#14323,#14324,#14325));
#4393=EDGE_LOOP('',(#14326,#14327,#14328,#14329));
#4394=EDGE_LOOP('',(#14330,#14331,#14332,#14333));
#4395=EDGE_LOOP('',(#14334,#14335,#14336,#14337));
#4396=EDGE_LOOP('',(#14338,#14339,#14340,#14341));
#4397=EDGE_LOOP('',(#14342,#14343,#14344,#14345));
#4398=EDGE_LOOP('',(#14346,#14347,#14348,#14349));
#4399=EDGE_LOOP('',(#14350,#14351,#14352,#14353));
#4400=EDGE_LOOP('',(#14354,#14355,#14356,#14357));
#4401=EDGE_LOOP('',(#14358,#14359,#14360,#14361));
#4402=EDGE_LOOP('',(#14362,#14363,#14364,#14365));
#4403=EDGE_LOOP('',(#14366,#14367,#14368,#14369));
#4404=EDGE_LOOP('',(#14370,#14371,#14372,#14373));
#4405=EDGE_LOOP('',(#14374,#14375,#14376,#14377,#14378,#14379,#14380,#14381));
#4406=EDGE_LOOP('',(#14382,#14383,#14384,#14385,#14386,#14387,#14388,#14389,
#14390,#14391,#14392,#14393,#14394,#14395,#14396,#14397,#14398,#14399,#14400,
#14401,#14402,#14403,#14404,#14405,#14406,#14407,#14408,#14409,#14410,#14411,
#14412,#14413,#14414,#14415,#14416,#14417));
#4407=EDGE_LOOP('',(#14418,#14419,#14420,#14421));
#4408=EDGE_LOOP('',(#14422,#14423,#14424,#14425,#14426,#14427,#14428,#14429,
#14430,#14431,#14432,#14433,#14434,#14435,#14436,#14437,#14438,#14439,#14440,
#14441,#14442,#14443,#14444,#14445,#14446,#14447,#14448,#14449,#14450,#14451,
#14452,#14453,#14454,#14455,#14456,#14457,#14458));
#4409=EDGE_LOOP('',(#14459,#14460,#14461,#14462));
#4410=EDGE_LOOP('',(#14463,#14464,#14465,#14466));
#4411=EDGE_LOOP('',(#14467,#14468,#14469,#14470));
#4412=EDGE_LOOP('',(#14471,#14472,#14473,#14474));
#4413=EDGE_LOOP('',(#14475,#14476,#14477,#14478));
#4414=EDGE_LOOP('',(#14479,#14480,#14481,#14482));
#4415=EDGE_LOOP('',(#14483,#14484,#14485,#14486));
#4416=EDGE_LOOP('',(#14487,#14488,#14489,#14490,#14491,#14492));
#4417=EDGE_LOOP('',(#14493));
#4418=EDGE_LOOP('',(#14494,#14495,#14496,#14497));
#4419=EDGE_LOOP('',(#14498,#14499,#14500,#14501));
#4420=EDGE_LOOP('',(#14502));
#4421=EDGE_LOOP('',(#14503,#14504,#14505,#14506,#14507,#14508));
#4422=EDGE_LOOP('',(#14509));
#4423=LINE('',#19955,#5186);
#4424=LINE('',#19957,#5187);
#4425=LINE('',#19959,#5188);
#4426=LINE('',#19960,#5189);
#4427=LINE('',#19965,#5190);
#4428=LINE('',#19967,#5191);
#4429=LINE('',#19971,#5192);
#4430=LINE('',#19973,#5193);
#4431=LINE('',#19974,#5194);
#4432=LINE('',#19976,#5195);
#4433=LINE('',#19988,#5196);
#4434=LINE('',#19991,#5197);
#4435=LINE('',#19996,#5198);
#4436=LINE('',#20000,#5199);
#4437=LINE('',#20005,#5200);
#4438=LINE('',#20011,#5201);
#4439=LINE('',#20017,#5202);
#4440=LINE('',#20023,#5203);
#4441=LINE('',#20029,#5204);
#4442=LINE('',#20035,#5205);
#4443=LINE('',#20041,#5206);
#4444=LINE('',#20045,#5207);
#4445=LINE('',#20047,#5208);
#4446=LINE('',#20048,#5209);
#4447=LINE('',#20051,#5210);
#4448=LINE('',#20053,#5211);
#4449=LINE('',#20054,#5212);
#4450=LINE('',#20056,#5213);
#4451=LINE('',#20057,#5214);
#4452=LINE('',#20068,#5215);
#4453=LINE('',#20071,#5216);
#4454=LINE('',#20076,#5217);
#4455=LINE('',#20078,#5218);
#4456=LINE('',#20086,#5219);
#4457=LINE('',#20105,#5220);
#4458=LINE('',#20194,#5221);
#4459=LINE('',#20281,#5222);
#4460=LINE('',#20371,#5223);
#4461=LINE('',#20458,#5224);
#4462=LINE('',#20548,#5225);
#4463=LINE('',#20617,#5226);
#4464=LINE('',#20647,#5227);
#4465=LINE('',#20685,#5228);
#4466=LINE('',#20722,#5229);
#4467=LINE('',#20759,#5230);
#4468=LINE('',#20797,#5231);
#4469=LINE('',#20835,#5232);
#4470=LINE('',#20855,#5233);
#4471=LINE('',#20876,#5234);
#4472=LINE('',#20905,#5235);
#4473=LINE('',#20953,#5236);
#4474=LINE('',#21001,#5237);
#4475=LINE('',#21052,#5238);
#4476=LINE('',#21103,#5239);
#4477=LINE('',#21151,#5240);
#4478=LINE('',#21202,#5241);
#4479=LINE('',#21253,#5242);
#4480=LINE('',#21301,#5243);
#4481=LINE('',#21349,#5244);
#4482=LINE('',#21403,#5245);
#4483=LINE('',#21451,#5246);
#4484=LINE('',#21499,#5247);
#4485=LINE('',#21550,#5248);
#4486=LINE('',#21601,#5249);
#4487=LINE('',#21649,#5250);
#4488=LINE('',#21700,#5251);
#4489=LINE('',#21739,#5252);
#4490=LINE('',#21757,#5253);
#4491=LINE('',#21782,#5254);
#4492=LINE('',#21806,#5255);
#4493=LINE('',#21831,#5256);
#4494=LINE('',#21855,#5257);
#4495=LINE('',#21880,#5258);
#4496=LINE('',#21905,#5259);
#4497=LINE('',#21929,#5260);
#4498=LINE('',#21954,#5261);
#4499=LINE('',#21978,#5262);
#4500=LINE('',#22003,#5263);
#4501=LINE('',#22028,#5264);
#4502=LINE('',#22052,#5265);
#4503=LINE('',#22077,#5266);
#4504=LINE('',#22101,#5267);
#4505=LINE('',#22126,#5268);
#4506=LINE('',#22151,#5269);
#4507=LINE('',#22175,#5270);
#4508=LINE('',#22192,#5271);
#4509=LINE('',#22213,#5272);
#4510=LINE('',#22242,#5273);
#4511=LINE('',#22290,#5274);
#4512=LINE('',#22338,#5275);
#4513=LINE('',#22389,#5276);
#4514=LINE('',#22440,#5277);
#4515=LINE('',#22488,#5278);
#4516=LINE('',#22539,#5279);
#4517=LINE('',#22590,#5280);
#4518=LINE('',#22638,#5281);
#4519=LINE('',#22686,#5282);
#4520=LINE('',#22740,#5283);
#4521=LINE('',#22788,#5284);
#4522=LINE('',#22836,#5285);
#4523=LINE('',#22887,#5286);
#4524=LINE('',#22938,#5287);
#4525=LINE('',#22986,#5288);
#4526=LINE('',#23037,#5289);
#4527=LINE('',#23076,#5290);
#4528=LINE('',#23094,#5291);
#4529=LINE('',#23119,#5292);
#4530=LINE('',#23143,#5293);
#4531=LINE('',#23168,#5294);
#4532=LINE('',#23192,#5295);
#4533=LINE('',#23217,#5296);
#4534=LINE('',#23242,#5297);
#4535=LINE('',#23266,#5298);
#4536=LINE('',#23291,#5299);
#4537=LINE('',#23315,#5300);
#4538=LINE('',#23340,#5301);
#4539=LINE('',#23365,#5302);
#4540=LINE('',#23389,#5303);
#4541=LINE('',#23414,#5304);
#4542=LINE('',#23438,#5305);
#4543=LINE('',#23463,#5306);
#4544=LINE('',#23488,#5307);
#4545=LINE('',#23512,#5308);
#4546=LINE('',#23529,#5309);
#4547=LINE('',#23550,#5310);
#4548=LINE('',#23579,#5311);
#4549=LINE('',#23627,#5312);
#4550=LINE('',#23675,#5313);
#4551=LINE('',#23726,#5314);
#4552=LINE('',#23777,#5315);
#4553=LINE('',#23825,#5316);
#4554=LINE('',#23876,#5317);
#4555=LINE('',#23927,#5318);
#4556=LINE('',#23975,#5319);
#4557=LINE('',#24023,#5320);
#4558=LINE('',#24077,#5321);
#4559=LINE('',#24125,#5322);
#4560=LINE('',#24173,#5323);
#4561=LINE('',#24224,#5324);
#4562=LINE('',#24275,#5325);
#4563=LINE('',#24323,#5326);
#4564=LINE('',#24374,#5327);
#4565=LINE('',#24413,#5328);
#4566=LINE('',#24431,#5329);
#4567=LINE('',#24456,#5330);
#4568=LINE('',#24480,#5331);
#4569=LINE('',#24505,#5332);
#4570=LINE('',#24529,#5333);
#4571=LINE('',#24554,#5334);
#4572=LINE('',#24579,#5335);
#4573=LINE('',#24603,#5336);
#4574=LINE('',#24628,#5337);
#4575=LINE('',#24652,#5338);
#4576=LINE('',#24677,#5339);
#4577=LINE('',#24702,#5340);
#4578=LINE('',#24726,#5341);
#4579=LINE('',#24751,#5342);
#4580=LINE('',#24775,#5343);
#4581=LINE('',#24800,#5344);
#4582=LINE('',#24825,#5345);
#4583=LINE('',#24849,#5346);
#4584=LINE('',#24866,#5347);
#4585=LINE('',#24887,#5348);
#4586=LINE('',#24916,#5349);
#4587=LINE('',#24964,#5350);
#4588=LINE('',#25012,#5351);
#4589=LINE('',#25063,#5352);
#4590=LINE('',#25114,#5353);
#4591=LINE('',#25162,#5354);
#4592=LINE('',#25213,#5355);
#4593=LINE('',#25264,#5356);
#4594=LINE('',#25312,#5357);
#4595=LINE('',#25360,#5358);
#4596=LINE('',#25414,#5359);
#4597=LINE('',#25462,#5360);
#4598=LINE('',#25510,#5361);
#4599=LINE('',#25561,#5362);
#4600=LINE('',#25612,#5363);
#4601=LINE('',#25660,#5364);
#4602=LINE('',#25711,#5365);
#4603=LINE('',#25750,#5366);
#4604=LINE('',#25768,#5367);
#4605=LINE('',#25793,#5368);
#4606=LINE('',#25817,#5369);
#4607=LINE('',#25842,#5370);
#4608=LINE('',#25866,#5371);
#4609=LINE('',#25891,#5372);
#4610=LINE('',#25916,#5373);
#4611=LINE('',#25940,#5374);
#4612=LINE('',#25965,#5375);
#4613=LINE('',#25989,#5376);
#4614=LINE('',#26014,#5377);
#4615=LINE('',#26039,#5378);
#4616=LINE('',#26063,#5379);
#4617=LINE('',#26088,#5380);
#4618=LINE('',#26112,#5381);
#4619=LINE('',#26137,#5382);
#4620=LINE('',#26162,#5383);
#4621=LINE('',#26186,#5384);
#4622=LINE('',#26203,#5385);
#4623=LINE('',#26224,#5386);
#4624=LINE('',#26253,#5387);
#4625=LINE('',#26301,#5388);
#4626=LINE('',#26349,#5389);
#4627=LINE('',#26400,#5390);
#4628=LINE('',#26451,#5391);
#4629=LINE('',#26499,#5392);
#4630=LINE('',#26550,#5393);
#4631=LINE('',#26601,#5394);
#4632=LINE('',#26649,#5395);
#4633=LINE('',#26697,#5396);
#4634=LINE('',#26751,#5397);
#4635=LINE('',#26799,#5398);
#4636=LINE('',#26847,#5399);
#4637=LINE('',#26898,#5400);
#4638=LINE('',#26949,#5401);
#4639=LINE('',#26997,#5402);
#4640=LINE('',#27048,#5403);
#4641=LINE('',#27087,#5404);
#4642=LINE('',#27105,#5405);
#4643=LINE('',#27130,#5406);
#4644=LINE('',#27154,#5407);
#4645=LINE('',#27179,#5408);
#4646=LINE('',#27203,#5409);
#4647=LINE('',#27228,#5410);
#4648=LINE('',#27253,#5411);
#4649=LINE('',#27277,#5412);
#4650=LINE('',#27302,#5413);
#4651=LINE('',#27326,#5414);
#4652=LINE('',#27351,#5415);
#4653=LINE('',#27376,#5416);
#4654=LINE('',#27400,#5417);
#4655=LINE('',#27425,#5418);
#4656=LINE('',#27449,#5419);
#4657=LINE('',#27474,#5420);
#4658=LINE('',#27499,#5421);
#4659=LINE('',#27523,#5422);
#4660=LINE('',#27540,#5423);
#4661=LINE('',#27561,#5424);
#4662=LINE('',#27590,#5425);
#4663=LINE('',#27638,#5426);
#4664=LINE('',#27686,#5427);
#4665=LINE('',#27737,#5428);
#4666=LINE('',#27788,#5429);
#4667=LINE('',#27836,#5430);
#4668=LINE('',#27887,#5431);
#4669=LINE('',#27938,#5432);
#4670=LINE('',#27986,#5433);
#4671=LINE('',#28034,#5434);
#4672=LINE('',#28088,#5435);
#4673=LINE('',#28136,#5436);
#4674=LINE('',#28184,#5437);
#4675=LINE('',#28235,#5438);
#4676=LINE('',#28286,#5439);
#4677=LINE('',#28334,#5440);
#4678=LINE('',#28385,#5441);
#4679=LINE('',#28424,#5442);
#4680=LINE('',#28442,#5443);
#4681=LINE('',#28467,#5444);
#4682=LINE('',#28491,#5445);
#4683=LINE('',#28516,#5446);
#4684=LINE('',#28540,#5447);
#4685=LINE('',#28565,#5448);
#4686=LINE('',#28590,#5449);
#4687=LINE('',#28614,#5450);
#4688=LINE('',#28639,#5451);
#4689=LINE('',#28663,#5452);
#4690=LINE('',#28688,#5453);
#4691=LINE('',#28713,#5454);
#4692=LINE('',#28737,#5455);
#4693=LINE('',#28762,#5456);
#4694=LINE('',#28786,#5457);
#4695=LINE('',#28811,#5458);
#4696=LINE('',#28836,#5459);
#4697=LINE('',#28860,#5460);
#4698=LINE('',#28877,#5461);
#4699=LINE('',#28898,#5462);
#4700=LINE('',#28927,#5463);
#4701=LINE('',#28975,#5464);
#4702=LINE('',#29023,#5465);
#4703=LINE('',#29074,#5466);
#4704=LINE('',#29125,#5467);
#4705=LINE('',#29173,#5468);
#4706=LINE('',#29224,#5469);
#4707=LINE('',#29275,#5470);
#4708=LINE('',#29323,#5471);
#4709=LINE('',#29371,#5472);
#4710=LINE('',#29425,#5473);
#4711=LINE('',#29473,#5474);
#4712=LINE('',#29521,#5475);
#4713=LINE('',#29572,#5476);
#4714=LINE('',#29623,#5477);
#4715=LINE('',#29671,#5478);
#4716=LINE('',#29722,#5479);
#4717=LINE('',#29761,#5480);
#4718=LINE('',#29779,#5481);
#4719=LINE('',#29804,#5482);
#4720=LINE('',#29828,#5483);
#4721=LINE('',#29853,#5484);
#4722=LINE('',#29877,#5485);
#4723=LINE('',#29902,#5486);
#4724=LINE('',#29927,#5487);
#4725=LINE('',#29951,#5488);
#4726=LINE('',#29976,#5489);
#4727=LINE('',#30000,#5490);
#4728=LINE('',#30025,#5491);
#4729=LINE('',#30050,#5492);
#4730=LINE('',#30074,#5493);
#4731=LINE('',#30099,#5494);
#4732=LINE('',#30123,#5495);
#4733=LINE('',#30148,#5496);
#4734=LINE('',#30173,#5497);
#4735=LINE('',#30197,#5498);
#4736=LINE('',#30214,#5499);
#4737=LINE('',#30235,#5500);
#4738=LINE('',#30264,#5501);
#4739=LINE('',#30312,#5502);
#4740=LINE('',#30360,#5503);
#4741=LINE('',#30411,#5504);
#4742=LINE('',#30462,#5505);
#4743=LINE('',#30510,#5506);
#4744=LINE('',#30561,#5507);
#4745=LINE('',#30612,#5508);
#4746=LINE('',#30660,#5509);
#4747=LINE('',#30708,#5510);
#4748=LINE('',#30762,#5511);
#4749=LINE('',#30810,#5512);
#4750=LINE('',#30858,#5513);
#4751=LINE('',#30909,#5514);
#4752=LINE('',#30960,#5515);
#4753=LINE('',#31008,#5516);
#4754=LINE('',#31059,#5517);
#4755=LINE('',#31098,#5518);
#4756=LINE('',#31116,#5519);
#4757=LINE('',#31141,#5520);
#4758=LINE('',#31165,#5521);
#4759=LINE('',#31190,#5522);
#4760=LINE('',#31214,#5523);
#4761=LINE('',#31239,#5524);
#4762=LINE('',#31264,#5525);
#4763=LINE('',#31288,#5526);
#4764=LINE('',#31313,#5527);
#4765=LINE('',#31337,#5528);
#4766=LINE('',#31362,#5529);
#4767=LINE('',#31387,#5530);
#4768=LINE('',#31411,#5531);
#4769=LINE('',#31436,#5532);
#4770=LINE('',#31460,#5533);
#4771=LINE('',#31485,#5534);
#4772=LINE('',#31510,#5535);
#4773=LINE('',#31534,#5536);
#4774=LINE('',#42655,#5537);
#4775=LINE('',#42657,#5538);
#4776=LINE('',#42659,#5539);
#4777=LINE('',#42660,#5540);
#4778=LINE('',#42663,#5541);
#4779=LINE('',#42665,#5542);
#4780=LINE('',#42666,#5543);
#4781=LINE('',#42670,#5544);
#4782=LINE('',#42671,#5545);
#4783=LINE('',#42672,#5546);
#4784=LINE('',#44023,#5547);
#4785=LINE('',#44025,#5548);
#4786=LINE('',#44026,#5549);
#4787=LINE('',#44030,#5550);
#4788=LINE('',#44032,#5551);
#4789=LINE('',#44033,#5552);
#4790=LINE('',#44036,#5553);
#4791=LINE('',#44038,#5554);
#4792=LINE('',#44039,#5555);
#4793=LINE('',#44041,#5556);
#4794=LINE('',#44055,#5557);
#4795=LINE('',#44058,#5558);
#4796=LINE('',#44069,#5559);
#4797=LINE('',#44071,#5560);
#4798=LINE('',#44075,#5561);
#4799=LINE('',#44083,#5562);
#4800=LINE('',#44106,#5563);
#4801=LINE('',#44157,#5564);
#4802=LINE('',#44208,#5565);
#4803=LINE('',#44256,#5566);
#4804=LINE('',#44307,#5567);
#4805=LINE('',#44358,#5568);
#4806=LINE('',#44406,#5569);
#4807=LINE('',#44457,#5570);
#4808=LINE('',#44508,#5571);
#4809=LINE('',#44556,#5572);
#4810=LINE('',#44607,#5573);
#4811=LINE('',#44655,#5574);
#4812=LINE('',#44706,#5575);
#4813=LINE('',#44757,#5576);
#4814=LINE('',#44805,#5577);
#4815=LINE('',#44856,#5578);
#4816=LINE('',#44907,#5579);
#4817=LINE('',#44961,#5580);
#4818=LINE('',#44987,#5581);
#4819=LINE('',#45011,#5582);
#4820=LINE('',#45036,#5583);
#4821=LINE('',#45061,#5584);
#4822=LINE('',#45085,#5585);
#4823=LINE('',#45110,#5586);
#4824=LINE('',#45135,#5587);
#4825=LINE('',#45159,#5588);
#4826=LINE('',#45184,#5589);
#4827=LINE('',#45209,#5590);
#4828=LINE('',#45233,#5591);
#4829=LINE('',#45257,#5592);
#4830=LINE('',#45283,#5593);
#4831=LINE('',#45307,#5594);
#4832=LINE('',#45331,#5595);
#4833=LINE('',#45357,#5596);
#4834=LINE('',#45381,#5597);
#4835=LINE('',#45413,#5598);
#4836=LINE('',#45424,#5599);
#4837=LINE('',#45428,#5600);
#4838=LINE('',#45430,#5601);
#4839=LINE('',#45432,#5602);
#4840=LINE('',#45433,#5603);
#4841=LINE('',#45436,#5604);
#4842=LINE('',#45438,#5605);
#4843=LINE('',#45439,#5606);
#4844=LINE('',#45443,#5607);
#4845=LINE('',#45446,#5608);
#4846=LINE('',#45447,#5609);
#4847=LINE('',#46712,#5610);
#4848=LINE('',#46715,#5611);
#4849=LINE('',#46719,#5612);
#4850=LINE('',#46721,#5613);
#4851=LINE('',#46727,#5614);
#4852=LINE('',#46740,#5615);
#4853=LINE('',#46743,#5616);
#4854=LINE('',#46750,#5617);
#4855=LINE('',#46754,#5618);
#4856=LINE('',#46760,#5619);
#4857=LINE('',#46766,#5620);
#4858=LINE('',#46775,#5621);
#4859=LINE('',#46781,#5622);
#4860=LINE('',#46789,#5623);
#4861=LINE('',#46791,#5624);
#4862=LINE('',#46793,#5625);
#4863=LINE('',#46794,#5626);
#4864=LINE('',#46798,#5627);
#4865=LINE('',#46800,#5628);
#4866=LINE('',#46802,#5629);
#4867=LINE('',#46803,#5630);
#4868=LINE('',#46816,#5631);
#4869=LINE('',#46818,#5632);
#4870=LINE('',#46820,#5633);
#4871=LINE('',#46821,#5634);
#4872=LINE('',#46824,#5635);
#4873=LINE('',#46826,#5636);
#4874=LINE('',#46827,#5637);
#4875=LINE('',#46830,#5638);
#4876=LINE('',#46832,#5639);
#4877=LINE('',#46833,#5640);
#4878=LINE('',#46835,#5641);
#4879=LINE('',#46836,#5642);
#4880=LINE('',#46843,#5643);
#4881=LINE('',#46885,#5644);
#4882=LINE('',#46933,#5645);
#4883=LINE('',#46984,#5646);
#4884=LINE('',#47035,#5647);
#4885=LINE('',#47083,#5648);
#4886=LINE('',#47131,#5649);
#4887=LINE('',#47185,#5650);
#4888=LINE('',#47233,#5651);
#4889=LINE('',#47281,#5652);
#4890=LINE('',#47332,#5653);
#4891=LINE('',#47383,#5654);
#4892=LINE('',#47431,#5655);
#4893=LINE('',#47479,#5656);
#4894=LINE('',#47533,#5657);
#4895=LINE('',#47581,#5658);
#4896=LINE('',#47629,#5659);
#4897=LINE('',#47680,#5660);
#4898=LINE('',#47731,#5661);
#4899=LINE('',#47779,#5662);
#4900=LINE('',#47827,#5663);
#4901=LINE('',#47881,#5664);
#4902=LINE('',#47929,#5665);
#4903=LINE('',#47977,#5666);
#4904=LINE('',#48028,#5667);
#4905=LINE('',#48079,#5668);
#4906=LINE('',#48127,#5669);
#4907=LINE('',#48175,#5670);
#4908=LINE('',#48229,#5671);
#4909=LINE('',#48277,#5672);
#4910=LINE('',#48325,#5673);
#4911=LINE('',#48376,#5674);
#4912=LINE('',#48427,#5675);
#4913=LINE('',#48475,#5676);
#4914=LINE('',#48523,#5677);
#4915=LINE('',#48577,#5678);
#4916=LINE('',#48625,#5679);
#4917=LINE('',#48673,#5680);
#4918=LINE('',#48724,#5681);
#4919=LINE('',#48775,#5682);
#4920=LINE('',#48823,#5683);
#4921=LINE('',#48871,#5684);
#4922=LINE('',#48925,#5685);
#4923=LINE('',#48973,#5686);
#4924=LINE('',#49021,#5687);
#4925=LINE('',#49072,#5688);
#4926=LINE('',#49123,#5689);
#4927=LINE('',#49171,#5690);
#4928=LINE('',#49219,#5691);
#4929=LINE('',#49273,#5692);
#4930=LINE('',#49321,#5693);
#4931=LINE('',#49369,#5694);
#4932=LINE('',#49420,#5695);
#4933=LINE('',#49468,#5696);
#4934=LINE('',#49516,#5697);
#4935=LINE('',#49564,#5698);
#4936=LINE('',#49618,#5699);
#4937=LINE('',#49666,#5700);
#4938=LINE('',#49714,#5701);
#4939=LINE('',#49768,#5702);
#4940=LINE('',#49816,#5703);
#4941=LINE('',#49864,#5704);
#4942=LINE('',#49912,#5705);
#4943=LINE('',#49966,#5706);
#4944=LINE('',#50014,#5707);
#4945=LINE('',#50062,#5708);
#4946=LINE('',#50116,#5709);
#4947=LINE('',#50164,#5710);
#4948=LINE('',#50212,#5711);
#4949=LINE('',#50260,#5712);
#4950=LINE('',#50314,#5713);
#4951=LINE('',#50362,#5714);
#4952=LINE('',#50410,#5715);
#4953=LINE('',#50464,#5716);
#4954=LINE('',#50512,#5717);
#4955=LINE('',#50560,#5718);
#4956=LINE('',#50608,#5719);
#4957=LINE('',#50662,#5720);
#4958=LINE('',#50711,#5721);
#4959=LINE('',#50735,#5722);
#4960=LINE('',#50760,#5723);
#4961=LINE('',#50784,#5724);
#4962=LINE('',#50809,#5725);
#4963=LINE('',#50833,#5726);
#4964=LINE('',#50858,#5727);
#4965=LINE('',#50883,#5728);
#4966=LINE('',#50907,#5729);
#4967=LINE('',#50931,#5730);
#4968=LINE('',#50956,#5731);
#4969=LINE('',#50981,#5732);
#4970=LINE('',#51005,#5733);
#4971=LINE('',#51030,#5734);
#4972=LINE('',#51055,#5735);
#4973=LINE('',#51079,#5736);
#4974=LINE('',#51103,#5737);
#4975=LINE('',#51128,#5738);
#4976=LINE('',#51153,#5739);
#4977=LINE('',#51177,#5740);
#4978=LINE('',#51202,#5741);
#4979=LINE('',#51227,#5742);
#4980=LINE('',#51251,#5743);
#4981=LINE('',#51275,#5744);
#4982=LINE('',#51300,#5745);
#4983=LINE('',#51325,#5746);
#4984=LINE('',#51349,#5747);
#4985=LINE('',#51374,#5748);
#4986=LINE('',#51411,#5749);
#4987=LINE('',#51447,#5750);
#4988=LINE('',#51472,#5751);
#4989=LINE('',#51496,#5752);
#4990=LINE('',#51521,#5753);
#4991=LINE('',#51545,#5754);
#4992=LINE('',#51570,#5755);
#4993=LINE('',#51595,#5756);
#4994=LINE('',#51619,#5757);
#4995=LINE('',#51644,#5758);
#4996=LINE('',#51668,#5759);
#4997=LINE('',#51693,#5760);
#4998=LINE('',#51717,#5761);
#4999=LINE('',#51742,#5762);
#5000=LINE('',#51767,#5763);
#5001=LINE('',#51791,#5764);
#5002=LINE('',#51816,#5765);
#5003=LINE('',#51840,#5766);
#5004=LINE('',#51865,#5767);
#5005=LINE('',#51889,#5768);
#5006=LINE('',#51914,#5769);
#5007=LINE('',#51939,#5770);
#5008=LINE('',#51963,#5771);
#5009=LINE('',#51988,#5772);
#5010=LINE('',#52012,#5773);
#5011=LINE('',#52037,#5774);
#5012=LINE('',#52061,#5775);
#5013=LINE('',#52086,#5776);
#5014=LINE('',#52111,#5777);
#5015=LINE('',#52135,#5778);
#5016=LINE('',#52160,#5779);
#5017=LINE('',#52184,#5780);
#5018=LINE('',#52209,#5781);
#5019=LINE('',#52233,#5782);
#5020=LINE('',#52258,#5783);
#5021=LINE('',#52283,#5784);
#5022=LINE('',#52307,#5785);
#5023=LINE('',#52332,#5786);
#5024=LINE('',#52356,#5787);
#5025=LINE('',#52381,#5788);
#5026=LINE('',#52405,#5789);
#5027=LINE('',#52430,#5790);
#5028=LINE('',#52455,#5791);
#5029=LINE('',#52479,#5792);
#5030=LINE('',#52504,#5793);
#5031=LINE('',#52528,#5794);
#5032=LINE('',#52553,#5795);
#5033=LINE('',#52577,#5796);
#5034=LINE('',#52602,#5797);
#5035=LINE('',#52627,#5798);
#5036=LINE('',#52651,#5799);
#5037=LINE('',#52676,#5800);
#5038=LINE('',#52700,#5801);
#5039=LINE('',#52725,#5802);
#5040=LINE('',#53125,#5803);
#5041=LINE('',#53134,#5804);
#5042=LINE('',#57501,#5805);
#5043=LINE('',#57507,#5806);
#5044=LINE('',#57513,#5807);
#5045=LINE('',#57519,#5808);
#5046=LINE('',#57525,#5809);
#5047=LINE('',#57531,#5810);
#5048=LINE('',#57541,#5811);
#5049=LINE('',#57547,#5812);
#5050=LINE('',#57553,#5813);
#5051=LINE('',#57559,#5814);
#5052=LINE('',#57567,#5815);
#5053=LINE('',#57569,#5816);
#5054=LINE('',#57571,#5817);
#5055=LINE('',#57572,#5818);
#5056=LINE('',#57576,#5819);
#5057=LINE('',#57578,#5820);
#5058=LINE('',#57580,#5821);
#5059=LINE('',#57581,#5822);
#5060=LINE('',#57594,#5823);
#5061=LINE('',#57618,#5824);
#5062=LINE('',#57666,#5825);
#5063=LINE('',#57714,#5826);
#5064=LINE('',#57768,#5827);
#5065=LINE('',#57816,#5828);
#5066=LINE('',#57864,#5829);
#5067=LINE('',#57918,#5830);
#5068=LINE('',#57966,#5831);
#5069=LINE('',#58014,#5832);
#5070=LINE('',#58068,#5833);
#5071=LINE('',#58116,#5834);
#5072=LINE('',#58164,#5835);
#5073=LINE('',#58218,#5836);
#5074=LINE('',#58266,#5837);
#5075=LINE('',#58314,#5838);
#5076=LINE('',#58368,#5839);
#5077=LINE('',#58416,#5840);
#5078=LINE('',#58464,#5841);
#5079=LINE('',#58481,#5842);
#5080=LINE('',#58506,#5843);
#5081=LINE('',#58530,#5844);
#5082=LINE('',#58555,#5845);
#5083=LINE('',#58580,#5846);
#5084=LINE('',#58604,#5847);
#5085=LINE('',#58629,#5848);
#5086=LINE('',#58654,#5849);
#5087=LINE('',#58678,#5850);
#5088=LINE('',#58703,#5851);
#5089=LINE('',#58728,#5852);
#5090=LINE('',#58752,#5853);
#5091=LINE('',#58777,#5854);
#5092=LINE('',#58802,#5855);
#5093=LINE('',#58826,#5856);
#5094=LINE('',#58851,#5857);
#5095=LINE('',#58876,#5858);
#5096=LINE('',#58900,#5859);
#5097=LINE('',#58902,#5860);
#5098=LINE('',#58904,#5861);
#5099=LINE('',#58905,#5862);
#5100=LINE('',#58908,#5863);
#5101=LINE('',#58910,#5864);
#5102=LINE('',#58911,#5865);
#5103=LINE('',#58914,#5866);
#5104=LINE('',#58916,#5867);
#5105=LINE('',#58917,#5868);
#5106=LINE('',#58920,#5869);
#5107=LINE('',#58922,#5870);
#5108=LINE('',#58923,#5871);
#5109=LINE('',#58926,#5872);
#5110=LINE('',#58928,#5873);
#5111=LINE('',#58929,#5874);
#5112=LINE('',#58931,#5875);
#5113=LINE('',#58932,#5876);
#5114=LINE('',#60321,#5877);
#5115=LINE('',#60324,#5878);
#5116=LINE('',#60334,#5879);
#5117=LINE('',#60337,#5880);
#5118=LINE('',#60347,#5881);
#5119=LINE('',#60350,#5882);
#5120=LINE('',#60360,#5883);
#5121=LINE('',#60363,#5884);
#5122=LINE('',#60369,#5885);
#5123=LINE('',#60375,#5886);
#5124=LINE('',#60388,#5887);
#5125=LINE('',#60394,#5888);
#5126=LINE('',#60399,#5889);
#5127=LINE('',#60412,#5890);
#5128=LINE('',#60415,#5891);
#5129=LINE('',#60421,#5892);
#5130=LINE('',#60497,#5893);
#5131=LINE('',#61209,#5894);
#5132=LINE('',#61218,#5895);
#5133=LINE('',#61224,#5896);
#5134=LINE('',#61232,#5897);
#5135=LINE('',#61256,#5898);
#5136=LINE('',#61304,#5899);
#5137=LINE('',#61352,#5900);
#5138=LINE('',#61406,#5901);
#5139=LINE('',#61454,#5902);
#5140=LINE('',#61502,#5903);
#5141=LINE('',#61550,#5904);
#5142=LINE('',#61604,#5905);
#5143=LINE('',#61652,#5906);
#5144=LINE('',#61700,#5907);
#5145=LINE('',#61754,#5908);
#5146=LINE('',#61802,#5909);
#5147=LINE('',#61850,#5910);
#5148=LINE('',#61901,#5911);
#5149=LINE('',#61952,#5912);
#5150=LINE('',#62000,#5913);
#5151=LINE('',#62022,#5914);
#5152=LINE('',#62046,#5915);
#5153=LINE('',#62070,#5916);
#5154=LINE('',#62096,#5917);
#5155=LINE('',#62120,#5918);
#5156=LINE('',#62144,#5919);
#5157=LINE('',#62169,#5920);
#5158=LINE('',#62194,#5921);
#5159=LINE('',#62218,#5922);
#5160=LINE('',#62243,#5923);
#5161=LINE('',#62268,#5924);
#5162=LINE('',#62292,#5925);
#5163=LINE('',#62316,#5926);
#5164=LINE('',#62341,#5927);
#5165=LINE('',#62366,#5928);
#5166=LINE('',#62681,#5929);
#5167=LINE('',#63763,#5930);
#5168=LINE('',#63765,#5931);
#5169=LINE('',#63767,#5932);
#5170=LINE('',#63768,#5933);
#5171=LINE('',#63771,#5934);
#5172=LINE('',#63773,#5935);
#5173=LINE('',#63774,#5936);
#5174=LINE('',#63777,#5937);
#5175=LINE('',#63779,#5938);
#5176=LINE('',#63780,#5939);
#5177=LINE('',#63783,#5940);
#5178=LINE('',#63785,#5941);
#5179=LINE('',#63786,#5942);
#5180=LINE('',#63789,#5943);
#5181=LINE('',#63791,#5944);
#5182=LINE('',#63792,#5945);
#5183=LINE('',#63794,#5946);
#5184=LINE('',#63795,#5947);
#5185=LINE('',#63802,#5948);
#5186=VECTOR('',#16865,10.);
#5187=VECTOR('',#16866,10.);
#5188=VECTOR('',#16867,10.);
#5189=VECTOR('',#16868,10.);
#5190=VECTOR('',#16873,10.);
#5191=VECTOR('',#16874,10.);
#5192=VECTOR('',#16879,10.);
#5193=VECTOR('',#16880,10.);
#5194=VECTOR('',#16881,10.);
#5195=VECTOR('',#16884,10.);
#5196=VECTOR('',#16899,10.);
#5197=VECTOR('',#16902,10.);
#5198=VECTOR('',#16907,10.);
#5199=VECTOR('',#16910,70.);
#5200=VECTOR('',#16915,10.);
#5201=VECTOR('',#16922,8.);
#5202=VECTOR('',#16929,8.);
#5203=VECTOR('',#16936,5.5);
#5204=VECTOR('',#16943,5.5);
#5205=VECTOR('',#16950,5.5);
#5206=VECTOR('',#16957,5.5);
#5207=VECTOR('',#16962,10.);
#5208=VECTOR('',#16963,10.);
#5209=VECTOR('',#16964,10.);
#5210=VECTOR('',#16967,10.);
#5211=VECTOR('',#16968,10.);
#5212=VECTOR('',#16969,10.);
#5213=VECTOR('',#16972,10.);
#5214=VECTOR('',#16973,10.);
#5215=VECTOR('',#16988,100.);
#5216=VECTOR('',#16991,70.);
#5217=VECTOR('',#16998,50.);
#5218=VECTOR('',#16999,50.);
#5219=VECTOR('',#17010,6.);
#5220=VECTOR('',#17015,6.);
#5221=VECTOR('',#17020,6.);
#5222=VECTOR('',#17023,6.);
#5223=VECTOR('',#17026,6.);
#5224=VECTOR('',#17029,6.);
#5225=VECTOR('',#17032,6.);
#5226=VECTOR('',#17037,6.11325000000001);
#5227=VECTOR('',#17042,6.11325000000001);
#5228=VECTOR('',#17045,6.11325000000001);
#5229=VECTOR('',#17048,6.11325000000001);
#5230=VECTOR('',#17051,6.11325000000001);
#5231=VECTOR('',#17054,6.11325000000001);
#5232=VECTOR('',#17057,6.11325000000001);
#5233=VECTOR('',#17062,2.);
#5234=VECTOR('',#17065,2.);
#5235=VECTOR('',#17072,2.);
#5236=VECTOR('',#17075,2.);
#5237=VECTOR('',#17078,2.);
#5238=VECTOR('',#17081,2.);
#5239=VECTOR('',#17084,2.);
#5240=VECTOR('',#17087,2.);
#5241=VECTOR('',#17090,2.);
#5242=VECTOR('',#17093,2.);
#5243=VECTOR('',#17096,2.);
#5244=VECTOR('',#17099,2.);
#5245=VECTOR('',#17102,2.);
#5246=VECTOR('',#17105,2.);
#5247=VECTOR('',#17108,2.);
#5248=VECTOR('',#17111,2.);
#5249=VECTOR('',#17114,2.);
#5250=VECTOR('',#17117,2.);
#5251=VECTOR('',#17120,2.);
#5252=VECTOR('',#17125,2.05475);
#5253=VECTOR('',#17130,2.05475);
#5254=VECTOR('',#17133,2.05475);
#5255=VECTOR('',#17136,2.05475);
#5256=VECTOR('',#17139,2.05475);
#5257=VECTOR('',#17142,2.05475);
#5258=VECTOR('',#17145,2.05475);
#5259=VECTOR('',#17148,2.05475);
#5260=VECTOR('',#17151,2.05475);
#5261=VECTOR('',#17154,2.05475);
#5262=VECTOR('',#17157,2.05475);
#5263=VECTOR('',#17160,2.05475);
#5264=VECTOR('',#17163,2.05475);
#5265=VECTOR('',#17166,2.05475);
#5266=VECTOR('',#17169,2.05475);
#5267=VECTOR('',#17172,2.05475);
#5268=VECTOR('',#17175,2.05475);
#5269=VECTOR('',#17178,2.05475);
#5270=VECTOR('',#17181,2.05475);
#5271=VECTOR('',#17186,2.);
#5272=VECTOR('',#17189,2.);
#5273=VECTOR('',#17196,2.);
#5274=VECTOR('',#17199,2.);
#5275=VECTOR('',#17202,2.);
#5276=VECTOR('',#17205,2.);
#5277=VECTOR('',#17208,2.);
#5278=VECTOR('',#17211,2.);
#5279=VECTOR('',#17214,2.);
#5280=VECTOR('',#17217,2.);
#5281=VECTOR('',#17220,2.);
#5282=VECTOR('',#17223,2.);
#5283=VECTOR('',#17226,2.);
#5284=VECTOR('',#17229,2.);
#5285=VECTOR('',#17232,2.);
#5286=VECTOR('',#17235,2.);
#5287=VECTOR('',#17238,2.);
#5288=VECTOR('',#17241,2.);
#5289=VECTOR('',#17244,2.);
#5290=VECTOR('',#17249,2.05475);
#5291=VECTOR('',#17254,2.05475);
#5292=VECTOR('',#17257,2.05475);
#5293=VECTOR('',#17260,2.05475);
#5294=VECTOR('',#17263,2.05475);
#5295=VECTOR('',#17266,2.05475);
#5296=VECTOR('',#17269,2.05475);
#5297=VECTOR('',#17272,2.05475);
#5298=VECTOR('',#17275,2.05475);
#5299=VECTOR('',#17278,2.05475);
#5300=VECTOR('',#17281,2.05475);
#5301=VECTOR('',#17284,2.05475);
#5302=VECTOR('',#17287,2.05475);
#5303=VECTOR('',#17290,2.05475);
#5304=VECTOR('',#17293,2.05475);
#5305=VECTOR('',#17296,2.05475);
#5306=VECTOR('',#17299,2.05475);
#5307=VECTOR('',#17302,2.05475);
#5308=VECTOR('',#17305,2.05475);
#5309=VECTOR('',#17310,2.);
#5310=VECTOR('',#17313,2.);
#5311=VECTOR('',#17320,2.);
#5312=VECTOR('',#17323,2.);
#5313=VECTOR('',#17326,2.);
#5314=VECTOR('',#17329,2.);
#5315=VECTOR('',#17332,2.);
#5316=VECTOR('',#17335,2.);
#5317=VECTOR('',#17338,2.);
#5318=VECTOR('',#17341,2.);
#5319=VECTOR('',#17344,2.);
#5320=VECTOR('',#17347,2.);
#5321=VECTOR('',#17350,2.);
#5322=VECTOR('',#17353,2.);
#5323=VECTOR('',#17356,2.);
#5324=VECTOR('',#17359,2.);
#5325=VECTOR('',#17362,2.);
#5326=VECTOR('',#17365,2.);
#5327=VECTOR('',#17368,2.);
#5328=VECTOR('',#17373,2.05475);
#5329=VECTOR('',#17378,2.05475);
#5330=VECTOR('',#17381,2.05475);
#5331=VECTOR('',#17384,2.05475);
#5332=VECTOR('',#17387,2.05475);
#5333=VECTOR('',#17390,2.05475);
#5334=VECTOR('',#17393,2.05475);
#5335=VECTOR('',#17396,2.05475);
#5336=VECTOR('',#17399,2.05475);
#5337=VECTOR('',#17402,2.05475);
#5338=VECTOR('',#17405,2.05475);
#5339=VECTOR('',#17408,2.05475);
#5340=VECTOR('',#17411,2.05475);
#5341=VECTOR('',#17414,2.05475);
#5342=VECTOR('',#17417,2.05475);
#5343=VECTOR('',#17420,2.05475);
#5344=VECTOR('',#17423,2.05475);
#5345=VECTOR('',#17426,2.05475);
#5346=VECTOR('',#17429,2.05475);
#5347=VECTOR('',#17434,2.);
#5348=VECTOR('',#17437,2.);
#5349=VECTOR('',#17444,2.);
#5350=VECTOR('',#17447,2.);
#5351=VECTOR('',#17450,2.);
#5352=VECTOR('',#17453,2.);
#5353=VECTOR('',#17456,2.);
#5354=VECTOR('',#17459,2.);
#5355=VECTOR('',#17462,2.);
#5356=VECTOR('',#17465,2.);
#5357=VECTOR('',#17468,2.);
#5358=VECTOR('',#17471,2.);
#5359=VECTOR('',#17474,2.);
#5360=VECTOR('',#17477,2.);
#5361=VECTOR('',#17480,2.);
#5362=VECTOR('',#17483,2.);
#5363=VECTOR('',#17486,2.);
#5364=VECTOR('',#17489,2.);
#5365=VECTOR('',#17492,2.);
#5366=VECTOR('',#17497,2.05475);
#5367=VECTOR('',#17502,2.05475);
#5368=VECTOR('',#17505,2.05475);
#5369=VECTOR('',#17508,2.05475);
#5370=VECTOR('',#17511,2.05475);
#5371=VECTOR('',#17514,2.05475);
#5372=VECTOR('',#17517,2.05475);
#5373=VECTOR('',#17520,2.05475);
#5374=VECTOR('',#17523,2.05475);
#5375=VECTOR('',#17526,2.05475);
#5376=VECTOR('',#17529,2.05475);
#5377=VECTOR('',#17532,2.05475);
#5378=VECTOR('',#17535,2.05475);
#5379=VECTOR('',#17538,2.05475);
#5380=VECTOR('',#17541,2.05475);
#5381=VECTOR('',#17544,2.05475);
#5382=VECTOR('',#17547,2.05475);
#5383=VECTOR('',#17550,2.05475);
#5384=VECTOR('',#17553,2.05475);
#5385=VECTOR('',#17558,2.);
#5386=VECTOR('',#17561,2.);
#5387=VECTOR('',#17568,2.);
#5388=VECTOR('',#17571,2.);
#5389=VECTOR('',#17574,2.);
#5390=VECTOR('',#17577,2.);
#5391=VECTOR('',#17580,2.);
#5392=VECTOR('',#17583,2.);
#5393=VECTOR('',#17586,2.);
#5394=VECTOR('',#17589,2.);
#5395=VECTOR('',#17592,2.);
#5396=VECTOR('',#17595,2.);
#5397=VECTOR('',#17598,2.);
#5398=VECTOR('',#17601,2.);
#5399=VECTOR('',#17604,2.);
#5400=VECTOR('',#17607,2.);
#5401=VECTOR('',#17610,2.);
#5402=VECTOR('',#17613,2.);
#5403=VECTOR('',#17616,2.);
#5404=VECTOR('',#17621,2.05475);
#5405=VECTOR('',#17626,2.05475);
#5406=VECTOR('',#17629,2.05475);
#5407=VECTOR('',#17632,2.05475);
#5408=VECTOR('',#17635,2.05475);
#5409=VECTOR('',#17638,2.05475);
#5410=VECTOR('',#17641,2.05475);
#5411=VECTOR('',#17644,2.05475);
#5412=VECTOR('',#17647,2.05475);
#5413=VECTOR('',#17650,2.05475);
#5414=VECTOR('',#17653,2.05475);
#5415=VECTOR('',#17656,2.05475);
#5416=VECTOR('',#17659,2.05475);
#5417=VECTOR('',#17662,2.05475);
#5418=VECTOR('',#17665,2.05475);
#5419=VECTOR('',#17668,2.05475);
#5420=VECTOR('',#17671,2.05475);
#5421=VECTOR('',#17674,2.05475);
#5422=VECTOR('',#17677,2.05475);
#5423=VECTOR('',#17682,2.);
#5424=VECTOR('',#17685,2.);
#5425=VECTOR('',#17692,2.);
#5426=VECTOR('',#17695,2.);
#5427=VECTOR('',#17698,2.);
#5428=VECTOR('',#17701,2.);
#5429=VECTOR('',#17704,2.);
#5430=VECTOR('',#17707,2.);
#5431=VECTOR('',#17710,2.);
#5432=VECTOR('',#17713,2.);
#5433=VECTOR('',#17716,2.);
#5434=VECTOR('',#17719,2.);
#5435=VECTOR('',#17722,2.);
#5436=VECTOR('',#17725,2.);
#5437=VECTOR('',#17728,2.);
#5438=VECTOR('',#17731,2.);
#5439=VECTOR('',#17734,2.);
#5440=VECTOR('',#17737,2.);
#5441=VECTOR('',#17740,2.);
#5442=VECTOR('',#17745,2.05475000000001);
#5443=VECTOR('',#17750,2.05475000000001);
#5444=VECTOR('',#17753,2.05475000000001);
#5445=VECTOR('',#17756,2.05475000000001);
#5446=VECTOR('',#17759,2.05475000000001);
#5447=VECTOR('',#17762,2.05475000000001);
#5448=VECTOR('',#17765,2.05475000000001);
#5449=VECTOR('',#17768,2.05475000000001);
#5450=VECTOR('',#17771,2.05475000000001);
#5451=VECTOR('',#17774,2.05475000000001);
#5452=VECTOR('',#17777,2.05475000000001);
#5453=VECTOR('',#17780,2.05475000000001);
#5454=VECTOR('',#17783,2.05475000000001);
#5455=VECTOR('',#17786,2.05475000000001);
#5456=VECTOR('',#17789,2.05475000000001);
#5457=VECTOR('',#17792,2.05475000000001);
#5458=VECTOR('',#17795,2.05475000000001);
#5459=VECTOR('',#17798,2.05475000000001);
#5460=VECTOR('',#17801,2.05475000000001);
#5461=VECTOR('',#17806,2.);
#5462=VECTOR('',#17809,2.);
#5463=VECTOR('',#17816,2.);
#5464=VECTOR('',#17819,2.);
#5465=VECTOR('',#17822,2.);
#5466=VECTOR('',#17825,2.);
#5467=VECTOR('',#17828,2.);
#5468=VECTOR('',#17831,2.);
#5469=VECTOR('',#17834,2.);
#5470=VECTOR('',#17837,2.);
#5471=VECTOR('',#17840,2.);
#5472=VECTOR('',#17843,2.);
#5473=VECTOR('',#17846,2.);
#5474=VECTOR('',#17849,2.);
#5475=VECTOR('',#17852,2.);
#5476=VECTOR('',#17855,2.);
#5477=VECTOR('',#17858,2.);
#5478=VECTOR('',#17861,2.);
#5479=VECTOR('',#17864,2.);
#5480=VECTOR('',#17869,2.05475);
#5481=VECTOR('',#17874,2.05475);
#5482=VECTOR('',#17877,2.05475);
#5483=VECTOR('',#17880,2.05475);
#5484=VECTOR('',#17883,2.05475);
#5485=VECTOR('',#17886,2.05475);
#5486=VECTOR('',#17889,2.05475);
#5487=VECTOR('',#17892,2.05475);
#5488=VECTOR('',#17895,2.05475);
#5489=VECTOR('',#17898,2.05475);
#5490=VECTOR('',#17901,2.05475);
#5491=VECTOR('',#17904,2.05475);
#5492=VECTOR('',#17907,2.05475);
#5493=VECTOR('',#17910,2.05475);
#5494=VECTOR('',#17913,2.05475);
#5495=VECTOR('',#17916,2.05475);
#5496=VECTOR('',#17919,2.05475);
#5497=VECTOR('',#17922,2.05475);
#5498=VECTOR('',#17925,2.05475);
#5499=VECTOR('',#17930,2.);
#5500=VECTOR('',#17933,2.);
#5501=VECTOR('',#17940,2.);
#5502=VECTOR('',#17943,2.);
#5503=VECTOR('',#17946,2.);
#5504=VECTOR('',#17949,2.);
#5505=VECTOR('',#17952,2.);
#5506=VECTOR('',#17955,2.);
#5507=VECTOR('',#17958,2.);
#5508=VECTOR('',#17961,2.);
#5509=VECTOR('',#17964,2.);
#5510=VECTOR('',#17967,2.);
#5511=VECTOR('',#17970,2.);
#5512=VECTOR('',#17973,2.);
#5513=VECTOR('',#17976,2.);
#5514=VECTOR('',#17979,2.);
#5515=VECTOR('',#17982,2.);
#5516=VECTOR('',#17985,2.);
#5517=VECTOR('',#17988,2.);
#5518=VECTOR('',#17993,2.05475000000001);
#5519=VECTOR('',#17998,2.05475000000001);
#5520=VECTOR('',#18001,2.05475000000001);
#5521=VECTOR('',#18004,2.05475000000001);
#5522=VECTOR('',#18007,2.05475000000001);
#5523=VECTOR('',#18010,2.05475000000001);
#5524=VECTOR('',#18013,2.05475000000001);
#5525=VECTOR('',#18016,2.05475000000001);
#5526=VECTOR('',#18019,2.05475000000001);
#5527=VECTOR('',#18022,2.05475000000001);
#5528=VECTOR('',#18025,2.05475000000001);
#5529=VECTOR('',#18028,2.05475000000001);
#5530=VECTOR('',#18031,2.05475000000001);
#5531=VECTOR('',#18034,2.05475000000001);
#5532=VECTOR('',#18037,2.05475000000001);
#5533=VECTOR('',#18040,2.05475000000001);
#5534=VECTOR('',#18043,2.05475000000001);
#5535=VECTOR('',#18046,2.05475000000001);
#5536=VECTOR('',#18049,2.05475000000001);
#5537=VECTOR('',#18118,10.);
#5538=VECTOR('',#18119,10.);
#5539=VECTOR('',#18120,10.);
#5540=VECTOR('',#18121,10.);
#5541=VECTOR('',#18124,10.);
#5542=VECTOR('',#18125,10.);
#5543=VECTOR('',#18126,10.);
#5544=VECTOR('',#18129,10.);
#5545=VECTOR('',#18130,10.);
#5546=VECTOR('',#18131,10.);
#5547=VECTOR('',#18144,10.);
#5548=VECTOR('',#18145,10.);
#5549=VECTOR('',#18146,10.);
#5550=VECTOR('',#18151,10.);
#5551=VECTOR('',#18152,10.);
#5552=VECTOR('',#18153,10.);
#5553=VECTOR('',#18156,10.);
#5554=VECTOR('',#18157,10.);
#5555=VECTOR('',#18158,10.);
#5556=VECTOR('',#18161,10.);
#5557=VECTOR('',#18180,35.);
#5558=VECTOR('',#18183,40.);
#5559=VECTOR('',#18198,35.);
#5560=VECTOR('',#18201,40.);
#5561=VECTOR('',#18206,40.);
#5562=VECTOR('',#18217,3.);
#5563=VECTOR('',#18224,3.);
#5564=VECTOR('',#18227,3.);
#5565=VECTOR('',#18230,3.);
#5566=VECTOR('',#18233,3.);
#5567=VECTOR('',#18236,3.);
#5568=VECTOR('',#18239,3.);
#5569=VECTOR('',#18242,3.);
#5570=VECTOR('',#18245,3.);
#5571=VECTOR('',#18248,3.);
#5572=VECTOR('',#18251,3.);
#5573=VECTOR('',#18254,3.);
#5574=VECTOR('',#18257,3.);
#5575=VECTOR('',#18260,3.);
#5576=VECTOR('',#18263,3.);
#5577=VECTOR('',#18266,3.);
#5578=VECTOR('',#18269,3.);
#5579=VECTOR('',#18272,3.);
#5580=VECTOR('',#18275,3.0735);
#5581=VECTOR('',#18282,3.0735);
#5582=VECTOR('',#18285,3.0735);
#5583=VECTOR('',#18288,3.0735);
#5584=VECTOR('',#18291,3.0735);
#5585=VECTOR('',#18294,3.0735);
#5586=VECTOR('',#18297,3.0735);
#5587=VECTOR('',#18300,3.0735);
#5588=VECTOR('',#18303,3.0735);
#5589=VECTOR('',#18306,3.0735);
#5590=VECTOR('',#18309,3.0735);
#5591=VECTOR('',#18312,3.0735);
#5592=VECTOR('',#18315,3.0735);
#5593=VECTOR('',#18318,3.0735);
#5594=VECTOR('',#18321,3.0735);
#5595=VECTOR('',#18324,3.0735);
#5596=VECTOR('',#18327,3.0735);
#5597=VECTOR('',#18330,3.0735);
#5598=VECTOR('',#18335,19.);
#5599=VECTOR('',#18350,20.);
#5600=VECTOR('',#18353,10.);
#5601=VECTOR('',#18354,10.);
#5602=VECTOR('',#18355,10.);
#5603=VECTOR('',#18356,10.);
#5604=VECTOR('',#18359,10.);
#5605=VECTOR('',#18360,10.);
#5606=VECTOR('',#18361,10.);
#5607=VECTOR('',#18366,10.);
#5608=VECTOR('',#18369,10.);
#5609=VECTOR('',#18370,10.);
#5610=VECTOR('',#18381,10.);
#5611=VECTOR('',#18386,10.);
#5612=VECTOR('',#18391,8.);
#5613=VECTOR('',#18392,8.);
#5614=VECTOR('',#18401,12.);
#5615=VECTOR('',#18418,26.);
#5616=VECTOR('',#18421,20.);
#5617=VECTOR('',#18430,26.);
#5618=VECTOR('',#18437,20.);
#5619=VECTOR('',#18444,20.);
#5620=VECTOR('',#18451,27.);
#5621=VECTOR('',#18464,20.);
#5622=VECTOR('',#18471,27.5);
#5623=VECTOR('',#18482,10.);
#5624=VECTOR('',#18483,10.);
#5625=VECTOR('',#18484,10.);
#5626=VECTOR('',#18485,10.);
#5627=VECTOR('',#18488,10.);
#5628=VECTOR('',#18489,10.);
#5629=VECTOR('',#18490,10.);
#5630=VECTOR('',#18491,10.);
#5631=VECTOR('',#18512,10.);
#5632=VECTOR('',#18513,10.);
#5633=VECTOR('',#18514,10.);
#5634=VECTOR('',#18515,10.);
#5635=VECTOR('',#18518,10.);
#5636=VECTOR('',#18519,10.);
#5637=VECTOR('',#18520,10.);
#5638=VECTOR('',#18523,10.);
#5639=VECTOR('',#18524,10.);
#5640=VECTOR('',#18525,10.);
#5641=VECTOR('',#18528,10.);
#5642=VECTOR('',#18529,10.);
#5643=VECTOR('',#18538,6.);
#5644=VECTOR('',#18543,6.);
#5645=VECTOR('',#18546,6.);
#5646=VECTOR('',#18549,6.);
#5647=VECTOR('',#18552,6.);
#5648=VECTOR('',#18555,6.);
#5649=VECTOR('',#18558,6.);
#5650=VECTOR('',#18561,6.);
#5651=VECTOR('',#18564,6.);
#5652=VECTOR('',#18567,6.);
#5653=VECTOR('',#18570,6.);
#5654=VECTOR('',#18573,6.);
#5655=VECTOR('',#18576,6.);
#5656=VECTOR('',#18579,6.);
#5657=VECTOR('',#18582,6.);
#5658=VECTOR('',#18585,6.);
#5659=VECTOR('',#18588,6.);
#5660=VECTOR('',#18591,6.);
#5661=VECTOR('',#18594,6.);
#5662=VECTOR('',#18597,6.);
#5663=VECTOR('',#18600,6.);
#5664=VECTOR('',#18603,6.);
#5665=VECTOR('',#18606,6.);
#5666=VECTOR('',#18609,6.);
#5667=VECTOR('',#18612,6.);
#5668=VECTOR('',#18615,6.);
#5669=VECTOR('',#18618,6.);
#5670=VECTOR('',#18621,6.);
#5671=VECTOR('',#18624,6.);
#5672=VECTOR('',#18627,6.);
#5673=VECTOR('',#18630,6.);
#5674=VECTOR('',#18633,6.);
#5675=VECTOR('',#18636,6.);
#5676=VECTOR('',#18639,6.);
#5677=VECTOR('',#18642,6.);
#5678=VECTOR('',#18645,6.);
#5679=VECTOR('',#18648,6.);
#5680=VECTOR('',#18651,6.);
#5681=VECTOR('',#18654,6.);
#5682=VECTOR('',#18657,6.);
#5683=VECTOR('',#18660,6.);
#5684=VECTOR('',#18663,6.);
#5685=VECTOR('',#18666,6.);
#5686=VECTOR('',#18669,6.);
#5687=VECTOR('',#18672,6.);
#5688=VECTOR('',#18675,6.);
#5689=VECTOR('',#18678,6.);
#5690=VECTOR('',#18681,6.);
#5691=VECTOR('',#18684,6.);
#5692=VECTOR('',#18687,6.);
#5693=VECTOR('',#18690,6.);
#5694=VECTOR('',#18693,6.);
#5695=VECTOR('',#18696,6.);
#5696=VECTOR('',#18699,6.);
#5697=VECTOR('',#18702,6.);
#5698=VECTOR('',#18705,6.);
#5699=VECTOR('',#18708,6.);
#5700=VECTOR('',#18711,6.);
#5701=VECTOR('',#18714,6.);
#5702=VECTOR('',#18717,6.);
#5703=VECTOR('',#18720,6.);
#5704=VECTOR('',#18723,6.);
#5705=VECTOR('',#18726,6.);
#5706=VECTOR('',#18729,6.);
#5707=VECTOR('',#18732,6.);
#5708=VECTOR('',#18735,6.);
#5709=VECTOR('',#18738,6.);
#5710=VECTOR('',#18741,6.);
#5711=VECTOR('',#18744,6.);
#5712=VECTOR('',#18747,6.);
#5713=VECTOR('',#18750,6.);
#5714=VECTOR('',#18753,6.);
#5715=VECTOR('',#18756,6.);
#5716=VECTOR('',#18759,6.);
#5717=VECTOR('',#18762,6.);
#5718=VECTOR('',#18765,6.);
#5719=VECTOR('',#18768,6.);
#5720=VECTOR('',#18771,6.);
#5721=VECTOR('',#18776,6.);
#5722=VECTOR('',#18779,6.);
#5723=VECTOR('',#18784,4.91825);
#5724=VECTOR('',#18789,4.91825);
#5725=VECTOR('',#18792,4.91825);
#5726=VECTOR('',#18795,4.91825);
#5727=VECTOR('',#18798,4.91825);
#5728=VECTOR('',#18801,4.91825);
#5729=VECTOR('',#18804,4.91825);
#5730=VECTOR('',#18807,4.91825);
#5731=VECTOR('',#18810,4.91825);
#5732=VECTOR('',#18813,4.91825);
#5733=VECTOR('',#18816,4.91825);
#5734=VECTOR('',#18819,4.91825);
#5735=VECTOR('',#18822,4.91825);
#5736=VECTOR('',#18825,4.91825);
#5737=VECTOR('',#18828,4.91825);
#5738=VECTOR('',#18831,4.91825);
#5739=VECTOR('',#18834,4.91825);
#5740=VECTOR('',#18837,4.91825);
#5741=VECTOR('',#18840,4.91825);
#5742=VECTOR('',#18843,4.91825);
#5743=VECTOR('',#18846,4.91825);
#5744=VECTOR('',#18849,4.91825);
#5745=VECTOR('',#18852,4.91825);
#5746=VECTOR('',#18855,4.91825);
#5747=VECTOR('',#18858,4.91825);
#5748=VECTOR('',#18861,4.91825);
#5749=VECTOR('',#18864,4.91825);
#5750=VECTOR('',#18867,4.91825);
#5751=VECTOR('',#18870,4.91825);
#5752=VECTOR('',#18873,4.91825);
#5753=VECTOR('',#18876,4.91825);
#5754=VECTOR('',#18879,4.91825);
#5755=VECTOR('',#18882,4.91825);
#5756=VECTOR('',#18885,4.91825);
#5757=VECTOR('',#18888,4.91825);
#5758=VECTOR('',#18891,4.91825);
#5759=VECTOR('',#18894,4.91825);
#5760=VECTOR('',#18897,4.91825);
#5761=VECTOR('',#18900,4.91825);
#5762=VECTOR('',#18903,4.91825);
#5763=VECTOR('',#18906,4.91825);
#5764=VECTOR('',#18909,4.91825);
#5765=VECTOR('',#18912,4.91825);
#5766=VECTOR('',#18915,4.91825);
#5767=VECTOR('',#18918,4.91825);
#5768=VECTOR('',#18921,4.91825);
#5769=VECTOR('',#18924,4.91825);
#5770=VECTOR('',#18927,4.91825);
#5771=VECTOR('',#18930,4.91825);
#5772=VECTOR('',#18933,4.91825);
#5773=VECTOR('',#18936,4.91825);
#5774=VECTOR('',#18939,4.91825);
#5775=VECTOR('',#18942,4.91825);
#5776=VECTOR('',#18945,4.91825);
#5777=VECTOR('',#18948,4.91825);
#5778=VECTOR('',#18951,4.91825);
#5779=VECTOR('',#18954,4.91825);
#5780=VECTOR('',#18957,4.91825);
#5781=VECTOR('',#18960,4.91825);
#5782=VECTOR('',#18963,4.91825);
#5783=VECTOR('',#18966,4.91825);
#5784=VECTOR('',#18969,4.91825);
#5785=VECTOR('',#18972,4.91825);
#5786=VECTOR('',#18975,4.91825);
#5787=VECTOR('',#18978,4.91825);
#5788=VECTOR('',#18981,4.91825);
#5789=VECTOR('',#18984,4.91825);
#5790=VECTOR('',#18987,4.91825);
#5791=VECTOR('',#18990,4.91825);
#5792=VECTOR('',#18993,4.91825);
#5793=VECTOR('',#18996,4.91825);
#5794=VECTOR('',#18999,4.91825);
#5795=VECTOR('',#19002,4.91825);
#5796=VECTOR('',#19005,4.91825);
#5797=VECTOR('',#19008,4.91825);
#5798=VECTOR('',#19011,4.91825);
#5799=VECTOR('',#19014,4.91825);
#5800=VECTOR('',#19017,4.91825);
#5801=VECTOR('',#19020,4.91825);
#5802=VECTOR('',#19023,4.91825);
#5803=VECTOR('',#19036,5.);
#5804=VECTOR('',#19049,6.);
#5805=VECTOR('',#19060,3.);
#5806=VECTOR('',#19067,3.);
#5807=VECTOR('',#19074,3.);
#5808=VECTOR('',#19081,3.);
#5809=VECTOR('',#19088,3.);
#5810=VECTOR('',#19095,3.);
#5811=VECTOR('',#19108,25.);
#5812=VECTOR('',#19117,12.);
#5813=VECTOR('',#19124,6.);
#5814=VECTOR('',#19131,8.);
#5815=VECTOR('',#19142,10.);
#5816=VECTOR('',#19143,10.);
#5817=VECTOR('',#19144,10.);
#5818=VECTOR('',#19145,10.);
#5819=VECTOR('',#19148,10.);
#5820=VECTOR('',#19149,10.);
#5821=VECTOR('',#19150,10.);
#5822=VECTOR('',#19151,10.);
#5823=VECTOR('',#19172,3.);
#5824=VECTOR('',#19177,3.);
#5825=VECTOR('',#19180,3.);
#5826=VECTOR('',#19183,3.);
#5827=VECTOR('',#19186,3.);
#5828=VECTOR('',#19189,3.);
#5829=VECTOR('',#19192,3.);
#5830=VECTOR('',#19195,3.);
#5831=VECTOR('',#19198,3.);
#5832=VECTOR('',#19201,3.);
#5833=VECTOR('',#19204,3.);
#5834=VECTOR('',#19207,3.);
#5835=VECTOR('',#19210,3.);
#5836=VECTOR('',#19213,3.);
#5837=VECTOR('',#19216,3.);
#5838=VECTOR('',#19219,3.);
#5839=VECTOR('',#19222,3.);
#5840=VECTOR('',#19225,3.);
#5841=VECTOR('',#19228,2.37175);
#5842=VECTOR('',#19233,2.37175);
#5843=VECTOR('',#19236,2.37175);
#5844=VECTOR('',#19239,2.37175);
#5845=VECTOR('',#19242,2.37175);
#5846=VECTOR('',#19245,2.37175);
#5847=VECTOR('',#19248,2.37175);
#5848=VECTOR('',#19251,2.37175);
#5849=VECTOR('',#19254,2.37175);
#5850=VECTOR('',#19257,2.37175);
#5851=VECTOR('',#19260,2.37175);
#5852=VECTOR('',#19263,2.37175);
#5853=VECTOR('',#19266,2.37175);
#5854=VECTOR('',#19269,2.37175);
#5855=VECTOR('',#19272,2.37175);
#5856=VECTOR('',#19275,2.37175);
#5857=VECTOR('',#19278,2.37175);
#5858=VECTOR('',#19281,2.37175);
#5859=VECTOR('',#19284,10.);
#5860=VECTOR('',#19285,10.);
#5861=VECTOR('',#19286,10.);
#5862=VECTOR('',#19287,10.);
#5863=VECTOR('',#19290,10.);
#5864=VECTOR('',#19291,10.);
#5865=VECTOR('',#19292,10.);
#5866=VECTOR('',#19295,10.);
#5867=VECTOR('',#19296,10.);
#5868=VECTOR('',#19297,10.);
#5869=VECTOR('',#19300,10.);
#5870=VECTOR('',#19301,10.);
#5871=VECTOR('',#19302,10.);
#5872=VECTOR('',#19305,10.);
#5873=VECTOR('',#19306,10.);
#5874=VECTOR('',#19307,10.);
#5875=VECTOR('',#19310,10.);
#5876=VECTOR('',#19311,10.);
#5877=VECTOR('',#19338,4.);
#5878=VECTOR('',#19341,2.5);
#5879=VECTOR('',#19354,4.);
#5880=VECTOR('',#19357,2.5);
#5881=VECTOR('',#19370,4.);
#5882=VECTOR('',#19373,2.5);
#5883=VECTOR('',#19386,4.);
#5884=VECTOR('',#19389,2.5);
#5885=VECTOR('',#19396,28.);
#5886=VECTOR('',#19403,50.);
#5887=VECTOR('',#19422,27.5);
#5888=VECTOR('',#19429,20.);
#5889=VECTOR('',#19436,27.5);
#5890=VECTOR('',#19455,32.5);
#5891=VECTOR('',#19458,32.5);
#5892=VECTOR('',#19465,40.);
#5893=VECTOR('',#19492,28.);
#5894=VECTOR('',#19657,32.);
#5895=VECTOR('',#19670,6.);
#5896=VECTOR('',#19677,12.);
#5897=VECTOR('',#19688,2.);
#5898=VECTOR('',#19693,2.);
#5899=VECTOR('',#19696,2.);
#5900=VECTOR('',#19699,2.);
#5901=VECTOR('',#19702,2.);
#5902=VECTOR('',#19705,2.);
#5903=VECTOR('',#19708,2.);
#5904=VECTOR('',#19711,2.);
#5905=VECTOR('',#19714,2.);
#5906=VECTOR('',#19717,2.);
#5907=VECTOR('',#19720,2.);
#5908=VECTOR('',#19723,2.);
#5909=VECTOR('',#19726,2.);
#5910=VECTOR('',#19729,2.);
#5911=VECTOR('',#19732,2.);
#5912=VECTOR('',#19735,2.);
#5913=VECTOR('',#19738,1.5555);
#5914=VECTOR('',#19743,1.5555);
#5915=VECTOR('',#19746,1.5555);
#5916=VECTOR('',#19749,1.5555);
#5917=VECTOR('',#19752,1.5555);
#5918=VECTOR('',#19755,1.5555);
#5919=VECTOR('',#19758,1.5555);
#5920=VECTOR('',#19761,1.5555);
#5921=VECTOR('',#19764,1.5555);
#5922=VECTOR('',#19767,1.5555);
#5923=VECTOR('',#19770,1.5555);
#5924=VECTOR('',#19773,1.5555);
#5925=VECTOR('',#19776,1.5555);
#5926=VECTOR('',#19779,1.5555);
#5927=VECTOR('',#19782,1.5555);
#5928=VECTOR('',#19785,1.5555);
#5929=VECTOR('',#19790,1.5);
#5930=VECTOR('',#19801,10.);
#5931=VECTOR('',#19802,10.);
#5932=VECTOR('',#19803,10.);
#5933=VECTOR('',#19804,10.);
#5934=VECTOR('',#19807,10.);
#5935=VECTOR('',#19808,10.);
#5936=VECTOR('',#19809,10.);
#5937=VECTOR('',#19812,10.);
#5938=VECTOR('',#19813,10.);
#5939=VECTOR('',#19814,10.);
#5940=VECTOR('',#19817,10.);
#5941=VECTOR('',#19818,10.);
#5942=VECTOR('',#19819,10.);
#5943=VECTOR('',#19822,10.);
#5944=VECTOR('',#19823,10.);
#5945=VECTOR('',#19824,10.);
#5946=VECTOR('',#19827,10.);
#5947=VECTOR('',#19828,10.);
#5948=VECTOR('',#19837,3.5);
#5949=VERTEX_POINT('',#19953);
#5950=VERTEX_POINT('',#19954);
#5951=VERTEX_POINT('',#19956);
#5952=VERTEX_POINT('',#19958);
#5953=VERTEX_POINT('',#19962);
#5954=VERTEX_POINT('',#19964);
#5955=VERTEX_POINT('',#19966);
#5956=VERTEX_POINT('',#19970);
#5957=VERTEX_POINT('',#19972);
#5958=VERTEX_POINT('',#19978);
#5959=VERTEX_POINT('',#19982);
#5960=VERTEX_POINT('',#19983);
#5961=VERTEX_POINT('',#19987);
#5962=VERTEX_POINT('',#19989);
#5963=VERTEX_POINT('',#19993);
#5964=VERTEX_POINT('',#19995);
#5965=VERTEX_POINT('',#19997);
#5966=VERTEX_POINT('',#19999);
#5967=VERTEX_POINT('',#20002);
#5968=VERTEX_POINT('',#20004);
#5969=VERTEX_POINT('',#20008);
#5970=VERTEX_POINT('',#20010);
#5971=VERTEX_POINT('',#20014);
#5972=VERTEX_POINT('',#20016);
#5973=VERTEX_POINT('',#20020);
#5974=VERTEX_POINT('',#20022);
#5975=VERTEX_POINT('',#20026);
#5976=VERTEX_POINT('',#20028);
#5977=VERTEX_POINT('',#20032);
#5978=VERTEX_POINT('',#20034);
#5979=VERTEX_POINT('',#20038);
#5980=VERTEX_POINT('',#20040);
#5981=VERTEX_POINT('',#20044);
#5982=VERTEX_POINT('',#20046);
#5983=VERTEX_POINT('',#20050);
#5984=VERTEX_POINT('',#20052);
#5985=VERTEX_POINT('',#20060);
#5986=VERTEX_POINT('',#20063);
#5987=VERTEX_POINT('',#20065);
#5988=VERTEX_POINT('',#20070);
#5989=VERTEX_POINT('',#20074);
#5990=VERTEX_POINT('',#20077);
#5991=VERTEX_POINT('',#20084);
#5992=VERTEX_POINT('',#20085);
#5993=VERTEX_POINT('',#20087);
#5994=VERTEX_POINT('',#20103);
#5995=VERTEX_POINT('',#20104);
#5996=VERTEX_POINT('',#20106);
#5997=VERTEX_POINT('',#20192);
#5998=VERTEX_POINT('',#20193);
#5999=VERTEX_POINT('',#20279);
#6000=VERTEX_POINT('',#20280);
#6001=VERTEX_POINT('',#20369);
#6002=VERTEX_POINT('',#20370);
#6003=VERTEX_POINT('',#20456);
#6004=VERTEX_POINT('',#20457);
#6005=VERTEX_POINT('',#20546);
#6006=VERTEX_POINT('',#20547);
#6007=VERTEX_POINT('',#20549);
#6008=VERTEX_POINT('',#20575);
#6009=VERTEX_POINT('',#20615);
#6010=VERTEX_POINT('',#20616);
#6011=VERTEX_POINT('',#20618);
#6012=VERTEX_POINT('',#20630);
#6013=VERTEX_POINT('',#20645);
#6014=VERTEX_POINT('',#20646);
#6015=VERTEX_POINT('',#20683);
#6016=VERTEX_POINT('',#20684);
#6017=VERTEX_POINT('',#20720);
#6018=VERTEX_POINT('',#20721);
#6019=VERTEX_POINT('',#20757);
#6020=VERTEX_POINT('',#20758);
#6021=VERTEX_POINT('',#20795);
#6022=VERTEX_POINT('',#20796);
#6023=VERTEX_POINT('',#20833);
#6024=VERTEX_POINT('',#20834);
#6025=VERTEX_POINT('',#20836);
#6026=VERTEX_POINT('',#20843);
#6027=VERTEX_POINT('',#20853);
#6028=VERTEX_POINT('',#20854);
#6029=VERTEX_POINT('',#20856);
#6030=VERTEX_POINT('',#20873);
#6031=VERTEX_POINT('',#20875);
#6032=VERTEX_POINT('',#20878);
#6033=VERTEX_POINT('',#20903);
#6034=VERTEX_POINT('',#20904);
#6035=VERTEX_POINT('',#20951);
#6036=VERTEX_POINT('',#20952);
#6037=VERTEX_POINT('',#20999);
#6038=VERTEX_POINT('',#21000);
#6039=VERTEX_POINT('',#21050);
#6040=VERTEX_POINT('',#21051);
#6041=VERTEX_POINT('',#21101);
#6042=VERTEX_POINT('',#21102);
#6043=VERTEX_POINT('',#21149);
#6044=VERTEX_POINT('',#21150);
#6045=VERTEX_POINT('',#21200);
#6046=VERTEX_POINT('',#21201);
#6047=VERTEX_POINT('',#21251);
#6048=VERTEX_POINT('',#21252);
#6049=VERTEX_POINT('',#21299);
#6050=VERTEX_POINT('',#21300);
#6051=VERTEX_POINT('',#21347);
#6052=VERTEX_POINT('',#21348);
#6053=VERTEX_POINT('',#21401);
#6054=VERTEX_POINT('',#21402);
#6055=VERTEX_POINT('',#21449);
#6056=VERTEX_POINT('',#21450);
#6057=VERTEX_POINT('',#21497);
#6058=VERTEX_POINT('',#21498);
#6059=VERTEX_POINT('',#21548);
#6060=VERTEX_POINT('',#21549);
#6061=VERTEX_POINT('',#21599);
#6062=VERTEX_POINT('',#21600);
#6063=VERTEX_POINT('',#21647);
#6064=VERTEX_POINT('',#21648);
#6065=VERTEX_POINT('',#21698);
#6066=VERTEX_POINT('',#21699);
#6067=VERTEX_POINT('',#21701);
#6068=VERTEX_POINT('',#21715);
#6069=VERTEX_POINT('',#21737);
#6070=VERTEX_POINT('',#21738);
#6071=VERTEX_POINT('',#21740);
#6072=VERTEX_POINT('',#21746);
#6073=VERTEX_POINT('',#21755);
#6074=VERTEX_POINT('',#21756);
#6075=VERTEX_POINT('',#21780);
#6076=VERTEX_POINT('',#21781);
#6077=VERTEX_POINT('',#21804);
#6078=VERTEX_POINT('',#21805);
#6079=VERTEX_POINT('',#21829);
#6080=VERTEX_POINT('',#21830);
#6081=VERTEX_POINT('',#21853);
#6082=VERTEX_POINT('',#21854);
#6083=VERTEX_POINT('',#21878);
#6084=VERTEX_POINT('',#21879);
#6085=VERTEX_POINT('',#21903);
#6086=VERTEX_POINT('',#21904);
#6087=VERTEX_POINT('',#21927);
#6088=VERTEX_POINT('',#21928);
#6089=VERTEX_POINT('',#21952);
#6090=VERTEX_POINT('',#21953);
#6091=VERTEX_POINT('',#21976);
#6092=VERTEX_POINT('',#21977);
#6093=VERTEX_POINT('',#22001);
#6094=VERTEX_POINT('',#22002);
#6095=VERTEX_POINT('',#22026);
#6096=VERTEX_POINT('',#22027);
#6097=VERTEX_POINT('',#22050);
#6098=VERTEX_POINT('',#22051);
#6099=VERTEX_POINT('',#22075);
#6100=VERTEX_POINT('',#22076);
#6101=VERTEX_POINT('',#22099);
#6102=VERTEX_POINT('',#22100);
#6103=VERTEX_POINT('',#22124);
#6104=VERTEX_POINT('',#22125);
#6105=VERTEX_POINT('',#22149);
#6106=VERTEX_POINT('',#22150);
#6107=VERTEX_POINT('',#22173);
#6108=VERTEX_POINT('',#22174);
#6109=VERTEX_POINT('',#22176);
#6110=VERTEX_POINT('',#22182);
#6111=VERTEX_POINT('',#22190);
#6112=VERTEX_POINT('',#22191);
#6113=VERTEX_POINT('',#22193);
#6114=VERTEX_POINT('',#22210);
#6115=VERTEX_POINT('',#22212);
#6116=VERTEX_POINT('',#22215);
#6117=VERTEX_POINT('',#22240);
#6118=VERTEX_POINT('',#22241);
#6119=VERTEX_POINT('',#22288);
#6120=VERTEX_POINT('',#22289);
#6121=VERTEX_POINT('',#22336);
#6122=VERTEX_POINT('',#22337);
#6123=VERTEX_POINT('',#22387);
#6124=VERTEX_POINT('',#22388);
#6125=VERTEX_POINT('',#22438);
#6126=VERTEX_POINT('',#22439);
#6127=VERTEX_POINT('',#22486);
#6128=VERTEX_POINT('',#22487);
#6129=VERTEX_POINT('',#22537);
#6130=VERTEX_POINT('',#22538);
#6131=VERTEX_POINT('',#22588);
#6132=VERTEX_POINT('',#22589);
#6133=VERTEX_POINT('',#22636);
#6134=VERTEX_POINT('',#22637);
#6135=VERTEX_POINT('',#22684);
#6136=VERTEX_POINT('',#22685);
#6137=VERTEX_POINT('',#22738);
#6138=VERTEX_POINT('',#22739);
#6139=VERTEX_POINT('',#22786);
#6140=VERTEX_POINT('',#22787);
#6141=VERTEX_POINT('',#22834);
#6142=VERTEX_POINT('',#22835);
#6143=VERTEX_POINT('',#22885);
#6144=VERTEX_POINT('',#22886);
#6145=VERTEX_POINT('',#22936);
#6146=VERTEX_POINT('',#22937);
#6147=VERTEX_POINT('',#22984);
#6148=VERTEX_POINT('',#22985);
#6149=VERTEX_POINT('',#23035);
#6150=VERTEX_POINT('',#23036);
#6151=VERTEX_POINT('',#23038);
#6152=VERTEX_POINT('',#23052);
#6153=VERTEX_POINT('',#23074);
#6154=VERTEX_POINT('',#23075);
#6155=VERTEX_POINT('',#23077);
#6156=VERTEX_POINT('',#23083);
#6157=VERTEX_POINT('',#23092);
#6158=VERTEX_POINT('',#23093);
#6159=VERTEX_POINT('',#23117);
#6160=VERTEX_POINT('',#23118);
#6161=VERTEX_POINT('',#23141);
#6162=VERTEX_POINT('',#23142);
#6163=VERTEX_POINT('',#23166);
#6164=VERTEX_POINT('',#23167);
#6165=VERTEX_POINT('',#23190);
#6166=VERTEX_POINT('',#23191);
#6167=VERTEX_POINT('',#23215);
#6168=VERTEX_POINT('',#23216);
#6169=VERTEX_POINT('',#23240);
#6170=VERTEX_POINT('',#23241);
#6171=VERTEX_POINT('',#23264);
#6172=VERTEX_POINT('',#23265);
#6173=VERTEX_POINT('',#23289);
#6174=VERTEX_POINT('',#23290);
#6175=VERTEX_POINT('',#23313);
#6176=VERTEX_POINT('',#23314);
#6177=VERTEX_POINT('',#23338);
#6178=VERTEX_POINT('',#23339);
#6179=VERTEX_POINT('',#23363);
#6180=VERTEX_POINT('',#23364);
#6181=VERTEX_POINT('',#23387);
#6182=VERTEX_POINT('',#23388);
#6183=VERTEX_POINT('',#23412);
#6184=VERTEX_POINT('',#23413);
#6185=VERTEX_POINT('',#23436);
#6186=VERTEX_POINT('',#23437);
#6187=VERTEX_POINT('',#23461);
#6188=VERTEX_POINT('',#23462);
#6189=VERTEX_POINT('',#23486);
#6190=VERTEX_POINT('',#23487);
#6191=VERTEX_POINT('',#23510);
#6192=VERTEX_POINT('',#23511);
#6193=VERTEX_POINT('',#23513);
#6194=VERTEX_POINT('',#23519);
#6195=VERTEX_POINT('',#23527);
#6196=VERTEX_POINT('',#23528);
#6197=VERTEX_POINT('',#23530);
#6198=VERTEX_POINT('',#23547);
#6199=VERTEX_POINT('',#23549);
#6200=VERTEX_POINT('',#23552);
#6201=VERTEX_POINT('',#23577);
#6202=VERTEX_POINT('',#23578);
#6203=VERTEX_POINT('',#23625);
#6204=VERTEX_POINT('',#23626);
#6205=VERTEX_POINT('',#23673);
#6206=VERTEX_POINT('',#23674);
#6207=VERTEX_POINT('',#23724);
#6208=VERTEX_POINT('',#23725);
#6209=VERTEX_POINT('',#23775);
#6210=VERTEX_POINT('',#23776);
#6211=VERTEX_POINT('',#23823);
#6212=VERTEX_POINT('',#23824);
#6213=VERTEX_POINT('',#23874);
#6214=VERTEX_POINT('',#23875);
#6215=VERTEX_POINT('',#23925);
#6216=VERTEX_POINT('',#23926);
#6217=VERTEX_POINT('',#23973);
#6218=VERTEX_POINT('',#23974);
#6219=VERTEX_POINT('',#24021);
#6220=VERTEX_POINT('',#24022);
#6221=VERTEX_POINT('',#24075);
#6222=VERTEX_POINT('',#24076);
#6223=VERTEX_POINT('',#24123);
#6224=VERTEX_POINT('',#24124);
#6225=VERTEX_POINT('',#24171);
#6226=VERTEX_POINT('',#24172);
#6227=VERTEX_POINT('',#24222);
#6228=VERTEX_POINT('',#24223);
#6229=VERTEX_POINT('',#24273);
#6230=VERTEX_POINT('',#24274);
#6231=VERTEX_POINT('',#24321);
#6232=VERTEX_POINT('',#24322);
#6233=VERTEX_POINT('',#24372);
#6234=VERTEX_POINT('',#24373);
#6235=VERTEX_POINT('',#24375);
#6236=VERTEX_POINT('',#24389);
#6237=VERTEX_POINT('',#24411);
#6238=VERTEX_POINT('',#24412);
#6239=VERTEX_POINT('',#24414);
#6240=VERTEX_POINT('',#24420);
#6241=VERTEX_POINT('',#24429);
#6242=VERTEX_POINT('',#24430);
#6243=VERTEX_POINT('',#24454);
#6244=VERTEX_POINT('',#24455);
#6245=VERTEX_POINT('',#24478);
#6246=VERTEX_POINT('',#24479);
#6247=VERTEX_POINT('',#24503);
#6248=VERTEX_POINT('',#24504);
#6249=VERTEX_POINT('',#24527);
#6250=VERTEX_POINT('',#24528);
#6251=VERTEX_POINT('',#24552);
#6252=VERTEX_POINT('',#24553);
#6253=VERTEX_POINT('',#24577);
#6254=VERTEX_POINT('',#24578);
#6255=VERTEX_POINT('',#24601);
#6256=VERTEX_POINT('',#24602);
#6257=VERTEX_POINT('',#24626);
#6258=VERTEX_POINT('',#24627);
#6259=VERTEX_POINT('',#24650);
#6260=VERTEX_POINT('',#24651);
#6261=VERTEX_POINT('',#24675);
#6262=VERTEX_POINT('',#24676);
#6263=VERTEX_POINT('',#24700);
#6264=VERTEX_POINT('',#24701);
#6265=VERTEX_POINT('',#24724);
#6266=VERTEX_POINT('',#24725);
#6267=VERTEX_POINT('',#24749);
#6268=VERTEX_POINT('',#24750);
#6269=VERTEX_POINT('',#24773);
#6270=VERTEX_POINT('',#24774);
#6271=VERTEX_POINT('',#24798);
#6272=VERTEX_POINT('',#24799);
#6273=VERTEX_POINT('',#24823);
#6274=VERTEX_POINT('',#24824);
#6275=VERTEX_POINT('',#24847);
#6276=VERTEX_POINT('',#24848);
#6277=VERTEX_POINT('',#24850);
#6278=VERTEX_POINT('',#24856);
#6279=VERTEX_POINT('',#24864);
#6280=VERTEX_POINT('',#24865);
#6281=VERTEX_POINT('',#24867);
#6282=VERTEX_POINT('',#24884);
#6283=VERTEX_POINT('',#24886);
#6284=VERTEX_POINT('',#24889);
#6285=VERTEX_POINT('',#24914);
#6286=VERTEX_POINT('',#24915);
#6287=VERTEX_POINT('',#24962);
#6288=VERTEX_POINT('',#24963);
#6289=VERTEX_POINT('',#25010);
#6290=VERTEX_POINT('',#25011);
#6291=VERTEX_POINT('',#25061);
#6292=VERTEX_POINT('',#25062);
#6293=VERTEX_POINT('',#25112);
#6294=VERTEX_POINT('',#25113);
#6295=VERTEX_POINT('',#25160);
#6296=VERTEX_POINT('',#25161);
#6297=VERTEX_POINT('',#25211);
#6298=VERTEX_POINT('',#25212);
#6299=VERTEX_POINT('',#25262);
#6300=VERTEX_POINT('',#25263);
#6301=VERTEX_POINT('',#25310);
#6302=VERTEX_POINT('',#25311);
#6303=VERTEX_POINT('',#25358);
#6304=VERTEX_POINT('',#25359);
#6305=VERTEX_POINT('',#25412);
#6306=VERTEX_POINT('',#25413);
#6307=VERTEX_POINT('',#25460);
#6308=VERTEX_POINT('',#25461);
#6309=VERTEX_POINT('',#25508);
#6310=VERTEX_POINT('',#25509);
#6311=VERTEX_POINT('',#25559);
#6312=VERTEX_POINT('',#25560);
#6313=VERTEX_POINT('',#25610);
#6314=VERTEX_POINT('',#25611);
#6315=VERTEX_POINT('',#25658);
#6316=VERTEX_POINT('',#25659);
#6317=VERTEX_POINT('',#25709);
#6318=VERTEX_POINT('',#25710);
#6319=VERTEX_POINT('',#25712);
#6320=VERTEX_POINT('',#25726);
#6321=VERTEX_POINT('',#25748);
#6322=VERTEX_POINT('',#25749);
#6323=VERTEX_POINT('',#25751);
#6324=VERTEX_POINT('',#25757);
#6325=VERTEX_POINT('',#25766);
#6326=VERTEX_POINT('',#25767);
#6327=VERTEX_POINT('',#25791);
#6328=VERTEX_POINT('',#25792);
#6329=VERTEX_POINT('',#25815);
#6330=VERTEX_POINT('',#25816);
#6331=VERTEX_POINT('',#25840);
#6332=VERTEX_POINT('',#25841);
#6333=VERTEX_POINT('',#25864);
#6334=VERTEX_POINT('',#25865);
#6335=VERTEX_POINT('',#25889);
#6336=VERTEX_POINT('',#25890);
#6337=VERTEX_POINT('',#25914);
#6338=VERTEX_POINT('',#25915);
#6339=VERTEX_POINT('',#25938);
#6340=VERTEX_POINT('',#25939);
#6341=VERTEX_POINT('',#25963);
#6342=VERTEX_POINT('',#25964);
#6343=VERTEX_POINT('',#25987);
#6344=VERTEX_POINT('',#25988);
#6345=VERTEX_POINT('',#26012);
#6346=VERTEX_POINT('',#26013);
#6347=VERTEX_POINT('',#26037);
#6348=VERTEX_POINT('',#26038);
#6349=VERTEX_POINT('',#26061);
#6350=VERTEX_POINT('',#26062);
#6351=VERTEX_POINT('',#26086);
#6352=VERTEX_POINT('',#26087);
#6353=VERTEX_POINT('',#26110);
#6354=VERTEX_POINT('',#26111);
#6355=VERTEX_POINT('',#26135);
#6356=VERTEX_POINT('',#26136);
#6357=VERTEX_POINT('',#26160);
#6358=VERTEX_POINT('',#26161);
#6359=VERTEX_POINT('',#26184);
#6360=VERTEX_POINT('',#26185);
#6361=VERTEX_POINT('',#26187);
#6362=VERTEX_POINT('',#26193);
#6363=VERTEX_POINT('',#26201);
#6364=VERTEX_POINT('',#26202);
#6365=VERTEX_POINT('',#26204);
#6366=VERTEX_POINT('',#26221);
#6367=VERTEX_POINT('',#26223);
#6368=VERTEX_POINT('',#26226);
#6369=VERTEX_POINT('',#26251);
#6370=VERTEX_POINT('',#26252);
#6371=VERTEX_POINT('',#26299);
#6372=VERTEX_POINT('',#26300);
#6373=VERTEX_POINT('',#26347);
#6374=VERTEX_POINT('',#26348);
#6375=VERTEX_POINT('',#26398);
#6376=VERTEX_POINT('',#26399);
#6377=VERTEX_POINT('',#26449);
#6378=VERTEX_POINT('',#26450);
#6379=VERTEX_POINT('',#26497);
#6380=VERTEX_POINT('',#26498);
#6381=VERTEX_POINT('',#26548);
#6382=VERTEX_POINT('',#26549);
#6383=VERTEX_POINT('',#26599);
#6384=VERTEX_POINT('',#26600);
#6385=VERTEX_POINT('',#26647);
#6386=VERTEX_POINT('',#26648);
#6387=VERTEX_POINT('',#26695);
#6388=VERTEX_POINT('',#26696);
#6389=VERTEX_POINT('',#26749);
#6390=VERTEX_POINT('',#26750);
#6391=VERTEX_POINT('',#26797);
#6392=VERTEX_POINT('',#26798);
#6393=VERTEX_POINT('',#26845);
#6394=VERTEX_POINT('',#26846);
#6395=VERTEX_POINT('',#26896);
#6396=VERTEX_POINT('',#26897);
#6397=VERTEX_POINT('',#26947);
#6398=VERTEX_POINT('',#26948);
#6399=VERTEX_POINT('',#26995);
#6400=VERTEX_POINT('',#26996);
#6401=VERTEX_POINT('',#27046);
#6402=VERTEX_POINT('',#27047);
#6403=VERTEX_POINT('',#27049);
#6404=VERTEX_POINT('',#27063);
#6405=VERTEX_POINT('',#27085);
#6406=VERTEX_POINT('',#27086);
#6407=VERTEX_POINT('',#27088);
#6408=VERTEX_POINT('',#27094);
#6409=VERTEX_POINT('',#27103);
#6410=VERTEX_POINT('',#27104);
#6411=VERTEX_POINT('',#27128);
#6412=VERTEX_POINT('',#27129);
#6413=VERTEX_POINT('',#27152);
#6414=VERTEX_POINT('',#27153);
#6415=VERTEX_POINT('',#27177);
#6416=VERTEX_POINT('',#27178);
#6417=VERTEX_POINT('',#27201);
#6418=VERTEX_POINT('',#27202);
#6419=VERTEX_POINT('',#27226);
#6420=VERTEX_POINT('',#27227);
#6421=VERTEX_POINT('',#27251);
#6422=VERTEX_POINT('',#27252);
#6423=VERTEX_POINT('',#27275);
#6424=VERTEX_POINT('',#27276);
#6425=VERTEX_POINT('',#27300);
#6426=VERTEX_POINT('',#27301);
#6427=VERTEX_POINT('',#27324);
#6428=VERTEX_POINT('',#27325);
#6429=VERTEX_POINT('',#27349);
#6430=VERTEX_POINT('',#27350);
#6431=VERTEX_POINT('',#27374);
#6432=VERTEX_POINT('',#27375);
#6433=VERTEX_POINT('',#27398);
#6434=VERTEX_POINT('',#27399);
#6435=VERTEX_POINT('',#27423);
#6436=VERTEX_POINT('',#27424);
#6437=VERTEX_POINT('',#27447);
#6438=VERTEX_POINT('',#27448);
#6439=VERTEX_POINT('',#27472);
#6440=VERTEX_POINT('',#27473);
#6441=VERTEX_POINT('',#27497);
#6442=VERTEX_POINT('',#27498);
#6443=VERTEX_POINT('',#27521);
#6444=VERTEX_POINT('',#27522);
#6445=VERTEX_POINT('',#27524);
#6446=VERTEX_POINT('',#27530);
#6447=VERTEX_POINT('',#27538);
#6448=VERTEX_POINT('',#27539);
#6449=VERTEX_POINT('',#27541);
#6450=VERTEX_POINT('',#27558);
#6451=VERTEX_POINT('',#27560);
#6452=VERTEX_POINT('',#27563);
#6453=VERTEX_POINT('',#27588);
#6454=VERTEX_POINT('',#27589);
#6455=VERTEX_POINT('',#27636);
#6456=VERTEX_POINT('',#27637);
#6457=VERTEX_POINT('',#27684);
#6458=VERTEX_POINT('',#27685);
#6459=VERTEX_POINT('',#27735);
#6460=VERTEX_POINT('',#27736);
#6461=VERTEX_POINT('',#27786);
#6462=VERTEX_POINT('',#27787);
#6463=VERTEX_POINT('',#27834);
#6464=VERTEX_POINT('',#27835);
#6465=VERTEX_POINT('',#27885);
#6466=VERTEX_POINT('',#27886);
#6467=VERTEX_POINT('',#27936);
#6468=VERTEX_POINT('',#27937);
#6469=VERTEX_POINT('',#27984);
#6470=VERTEX_POINT('',#27985);
#6471=VERTEX_POINT('',#28032);
#6472=VERTEX_POINT('',#28033);
#6473=VERTEX_POINT('',#28086);
#6474=VERTEX_POINT('',#28087);
#6475=VERTEX_POINT('',#28134);
#6476=VERTEX_POINT('',#28135);
#6477=VERTEX_POINT('',#28182);
#6478=VERTEX_POINT('',#28183);
#6479=VERTEX_POINT('',#28233);
#6480=VERTEX_POINT('',#28234);
#6481=VERTEX_POINT('',#28284);
#6482=VERTEX_POINT('',#28285);
#6483=VERTEX_POINT('',#28332);
#6484=VERTEX_POINT('',#28333);
#6485=VERTEX_POINT('',#28383);
#6486=VERTEX_POINT('',#28384);
#6487=VERTEX_POINT('',#28386);
#6488=VERTEX_POINT('',#28400);
#6489=VERTEX_POINT('',#28422);
#6490=VERTEX_POINT('',#28423);
#6491=VERTEX_POINT('',#28425);
#6492=VERTEX_POINT('',#28431);
#6493=VERTEX_POINT('',#28440);
#6494=VERTEX_POINT('',#28441);
#6495=VERTEX_POINT('',#28465);
#6496=VERTEX_POINT('',#28466);
#6497=VERTEX_POINT('',#28489);
#6498=VERTEX_POINT('',#28490);
#6499=VERTEX_POINT('',#28514);
#6500=VERTEX_POINT('',#28515);
#6501=VERTEX_POINT('',#28538);
#6502=VERTEX_POINT('',#28539);
#6503=VERTEX_POINT('',#28563);
#6504=VERTEX_POINT('',#28564);
#6505=VERTEX_POINT('',#28588);
#6506=VERTEX_POINT('',#28589);
#6507=VERTEX_POINT('',#28612);
#6508=VERTEX_POINT('',#28613);
#6509=VERTEX_POINT('',#28637);
#6510=VERTEX_POINT('',#28638);
#6511=VERTEX_POINT('',#28661);
#6512=VERTEX_POINT('',#28662);
#6513=VERTEX_POINT('',#28686);
#6514=VERTEX_POINT('',#28687);
#6515=VERTEX_POINT('',#28711);
#6516=VERTEX_POINT('',#28712);
#6517=VERTEX_POINT('',#28735);
#6518=VERTEX_POINT('',#28736);
#6519=VERTEX_POINT('',#28760);
#6520=VERTEX_POINT('',#28761);
#6521=VERTEX_POINT('',#28784);
#6522=VERTEX_POINT('',#28785);
#6523=VERTEX_POINT('',#28809);
#6524=VERTEX_POINT('',#28810);
#6525=VERTEX_POINT('',#28834);
#6526=VERTEX_POINT('',#28835);
#6527=VERTEX_POINT('',#28858);
#6528=VERTEX_POINT('',#28859);
#6529=VERTEX_POINT('',#28861);
#6530=VERTEX_POINT('',#28867);
#6531=VERTEX_POINT('',#28875);
#6532=VERTEX_POINT('',#28876);
#6533=VERTEX_POINT('',#28878);
#6534=VERTEX_POINT('',#28895);
#6535=VERTEX_POINT('',#28897);
#6536=VERTEX_POINT('',#28900);
#6537=VERTEX_POINT('',#28925);
#6538=VERTEX_POINT('',#28926);
#6539=VERTEX_POINT('',#28973);
#6540=VERTEX_POINT('',#28974);
#6541=VERTEX_POINT('',#29021);
#6542=VERTEX_POINT('',#29022);
#6543=VERTEX_POINT('',#29072);
#6544=VERTEX_POINT('',#29073);
#6545=VERTEX_POINT('',#29123);
#6546=VERTEX_POINT('',#29124);
#6547=VERTEX_POINT('',#29171);
#6548=VERTEX_POINT('',#29172);
#6549=VERTEX_POINT('',#29222);
#6550=VERTEX_POINT('',#29223);
#6551=VERTEX_POINT('',#29273);
#6552=VERTEX_POINT('',#29274);
#6553=VERTEX_POINT('',#29321);
#6554=VERTEX_POINT('',#29322);
#6555=VERTEX_POINT('',#29369);
#6556=VERTEX_POINT('',#29370);
#6557=VERTEX_POINT('',#29423);
#6558=VERTEX_POINT('',#29424);
#6559=VERTEX_POINT('',#29471);
#6560=VERTEX_POINT('',#29472);
#6561=VERTEX_POINT('',#29519);
#6562=VERTEX_POINT('',#29520);
#6563=VERTEX_POINT('',#29570);
#6564=VERTEX_POINT('',#29571);
#6565=VERTEX_POINT('',#29621);
#6566=VERTEX_POINT('',#29622);
#6567=VERTEX_POINT('',#29669);
#6568=VERTEX_POINT('',#29670);
#6569=VERTEX_POINT('',#29720);
#6570=VERTEX_POINT('',#29721);
#6571=VERTEX_POINT('',#29723);
#6572=VERTEX_POINT('',#29737);
#6573=VERTEX_POINT('',#29759);
#6574=VERTEX_POINT('',#29760);
#6575=VERTEX_POINT('',#29762);
#6576=VERTEX_POINT('',#29768);
#6577=VERTEX_POINT('',#29777);
#6578=VERTEX_POINT('',#29778);
#6579=VERTEX_POINT('',#29802);
#6580=VERTEX_POINT('',#29803);
#6581=VERTEX_POINT('',#29826);
#6582=VERTEX_POINT('',#29827);
#6583=VERTEX_POINT('',#29851);
#6584=VERTEX_POINT('',#29852);
#6585=VERTEX_POINT('',#29875);
#6586=VERTEX_POINT('',#29876);
#6587=VERTEX_POINT('',#29900);
#6588=VERTEX_POINT('',#29901);
#6589=VERTEX_POINT('',#29925);
#6590=VERTEX_POINT('',#29926);
#6591=VERTEX_POINT('',#29949);
#6592=VERTEX_POINT('',#29950);
#6593=VERTEX_POINT('',#29974);
#6594=VERTEX_POINT('',#29975);
#6595=VERTEX_POINT('',#29998);
#6596=VERTEX_POINT('',#29999);
#6597=VERTEX_POINT('',#30023);
#6598=VERTEX_POINT('',#30024);
#6599=VERTEX_POINT('',#30048);
#6600=VERTEX_POINT('',#30049);
#6601=VERTEX_POINT('',#30072);
#6602=VERTEX_POINT('',#30073);
#6603=VERTEX_POINT('',#30097);
#6604=VERTEX_POINT('',#30098);
#6605=VERTEX_POINT('',#30121);
#6606=VERTEX_POINT('',#30122);
#6607=VERTEX_POINT('',#30146);
#6608=VERTEX_POINT('',#30147);
#6609=VERTEX_POINT('',#30171);
#6610=VERTEX_POINT('',#30172);
#6611=VERTEX_POINT('',#30195);
#6612=VERTEX_POINT('',#30196);
#6613=VERTEX_POINT('',#30198);
#6614=VERTEX_POINT('',#30204);
#6615=VERTEX_POINT('',#30212);
#6616=VERTEX_POINT('',#30213);
#6617=VERTEX_POINT('',#30215);
#6618=VERTEX_POINT('',#30232);
#6619=VERTEX_POINT('',#30234);
#6620=VERTEX_POINT('',#30237);
#6621=VERTEX_POINT('',#30262);
#6622=VERTEX_POINT('',#30263);
#6623=VERTEX_POINT('',#30310);
#6624=VERTEX_POINT('',#30311);
#6625=VERTEX_POINT('',#30358);
#6626=VERTEX_POINT('',#30359);
#6627=VERTEX_POINT('',#30409);
#6628=VERTEX_POINT('',#30410);
#6629=VERTEX_POINT('',#30460);
#6630=VERTEX_POINT('',#30461);
#6631=VERTEX_POINT('',#30508);
#6632=VERTEX_POINT('',#30509);
#6633=VERTEX_POINT('',#30559);
#6634=VERTEX_POINT('',#30560);
#6635=VERTEX_POINT('',#30610);
#6636=VERTEX_POINT('',#30611);
#6637=VERTEX_POINT('',#30658);
#6638=VERTEX_POINT('',#30659);
#6639=VERTEX_POINT('',#30706);
#6640=VERTEX_POINT('',#30707);
#6641=VERTEX_POINT('',#30760);
#6642=VERTEX_POINT('',#30761);
#6643=VERTEX_POINT('',#30808);
#6644=VERTEX_POINT('',#30809);
#6645=VERTEX_POINT('',#30856);
#6646=VERTEX_POINT('',#30857);
#6647=VERTEX_POINT('',#30907);
#6648=VERTEX_POINT('',#30908);
#6649=VERTEX_POINT('',#30958);
#6650=VERTEX_POINT('',#30959);
#6651=VERTEX_POINT('',#31006);
#6652=VERTEX_POINT('',#31007);
#6653=VERTEX_POINT('',#31057);
#6654=VERTEX_POINT('',#31058);
#6655=VERTEX_POINT('',#31060);
#6656=VERTEX_POINT('',#31074);
#6657=VERTEX_POINT('',#31096);
#6658=VERTEX_POINT('',#31097);
#6659=VERTEX_POINT('',#31099);
#6660=VERTEX_POINT('',#31105);
#6661=VERTEX_POINT('',#31114);
#6662=VERTEX_POINT('',#31115);
#6663=VERTEX_POINT('',#31139);
#6664=VERTEX_POINT('',#31140);
#6665=VERTEX_POINT('',#31163);
#6666=VERTEX_POINT('',#31164);
#6667=VERTEX_POINT('',#31188);
#6668=VERTEX_POINT('',#31189);
#6669=VERTEX_POINT('',#31212);
#6670=VERTEX_POINT('',#31213);
#6671=VERTEX_POINT('',#31237);
#6672=VERTEX_POINT('',#31238);
#6673=VERTEX_POINT('',#31262);
#6674=VERTEX_POINT('',#31263);
#6675=VERTEX_POINT('',#31286);
#6676=VERTEX_POINT('',#31287);
#6677=VERTEX_POINT('',#31311);
#6678=VERTEX_POINT('',#31312);
#6679=VERTEX_POINT('',#31335);
#6680=VERTEX_POINT('',#31336);
#6681=VERTEX_POINT('',#31360);
#6682=VERTEX_POINT('',#31361);
#6683=VERTEX_POINT('',#31385);
#6684=VERTEX_POINT('',#31386);
#6685=VERTEX_POINT('',#31409);
#6686=VERTEX_POINT('',#31410);
#6687=VERTEX_POINT('',#31434);
#6688=VERTEX_POINT('',#31435);
#6689=VERTEX_POINT('',#31458);
#6690=VERTEX_POINT('',#31459);
#6691=VERTEX_POINT('',#31483);
#6692=VERTEX_POINT('',#31484);
#6693=VERTEX_POINT('',#31508);
#6694=VERTEX_POINT('',#31509);
#6695=VERTEX_POINT('',#31532);
#6696=VERTEX_POINT('',#31533);
#6697=VERTEX_POINT('',#31535);
#6698=VERTEX_POINT('',#31541);
#6699=VERTEX_POINT('',#42653);
#6700=VERTEX_POINT('',#42654);
#6701=VERTEX_POINT('',#42656);
#6702=VERTEX_POINT('',#42658);
#6703=VERTEX_POINT('',#42662);
#6704=VERTEX_POINT('',#42664);
#6705=VERTEX_POINT('',#42668);
#6706=VERTEX_POINT('',#42669);
#6707=VERTEX_POINT('',#42675);
#6708=VERTEX_POINT('',#44019);
#6709=VERTEX_POINT('',#44020);
#6710=VERTEX_POINT('',#44022);
#6711=VERTEX_POINT('',#44024);
#6712=VERTEX_POINT('',#44029);
#6713=VERTEX_POINT('',#44031);
#6714=VERTEX_POINT('',#44035);
#6715=VERTEX_POINT('',#44037);
#6716=VERTEX_POINT('',#44045);
#6717=VERTEX_POINT('',#44047);
#6718=VERTEX_POINT('',#44050);
#6719=VERTEX_POINT('',#44052);
#6720=VERTEX_POINT('',#44057);
#6721=VERTEX_POINT('',#44061);
#6722=VERTEX_POINT('',#44064);
#6723=VERTEX_POINT('',#44066);
#6724=VERTEX_POINT('',#44073);
#6725=VERTEX_POINT('',#44081);
#6726=VERTEX_POINT('',#44082);
#6727=VERTEX_POINT('',#44084);
#6728=VERTEX_POINT('',#44089);
#6729=VERTEX_POINT('',#44091);
#6730=VERTEX_POINT('',#44104);
#6731=VERTEX_POINT('',#44105);
#6732=VERTEX_POINT('',#44155);
#6733=VERTEX_POINT('',#44156);
#6734=VERTEX_POINT('',#44206);
#6735=VERTEX_POINT('',#44207);
#6736=VERTEX_POINT('',#44254);
#6737=VERTEX_POINT('',#44255);
#6738=VERTEX_POINT('',#44305);
#6739=VERTEX_POINT('',#44306);
#6740=VERTEX_POINT('',#44356);
#6741=VERTEX_POINT('',#44357);
#6742=VERTEX_POINT('',#44404);
#6743=VERTEX_POINT('',#44405);
#6744=VERTEX_POINT('',#44455);
#6745=VERTEX_POINT('',#44456);
#6746=VERTEX_POINT('',#44506);
#6747=VERTEX_POINT('',#44507);
#6748=VERTEX_POINT('',#44554);
#6749=VERTEX_POINT('',#44555);
#6750=VERTEX_POINT('',#44605);
#6751=VERTEX_POINT('',#44606);
#6752=VERTEX_POINT('',#44653);
#6753=VERTEX_POINT('',#44654);
#6754=VERTEX_POINT('',#44704);
#6755=VERTEX_POINT('',#44705);
#6756=VERTEX_POINT('',#44755);
#6757=VERTEX_POINT('',#44756);
#6758=VERTEX_POINT('',#44803);
#6759=VERTEX_POINT('',#44804);
#6760=VERTEX_POINT('',#44854);
#6761=VERTEX_POINT('',#44855);
#6762=VERTEX_POINT('',#44905);
#6763=VERTEX_POINT('',#44906);
#6764=VERTEX_POINT('',#44908);
#6765=VERTEX_POINT('',#44922);
#6766=VERTEX_POINT('',#44959);
#6767=VERTEX_POINT('',#44960);
#6768=VERTEX_POINT('',#44962);
#6769=VERTEX_POINT('',#44971);
#6770=VERTEX_POINT('',#44973);
#6771=VERTEX_POINT('',#44985);
#6772=VERTEX_POINT('',#44986);
#6773=VERTEX_POINT('',#45009);
#6774=VERTEX_POINT('',#45010);
#6775=VERTEX_POINT('',#45034);
#6776=VERTEX_POINT('',#45035);
#6777=VERTEX_POINT('',#45059);
#6778=VERTEX_POINT('',#45060);
#6779=VERTEX_POINT('',#45083);
#6780=VERTEX_POINT('',#45084);
#6781=VERTEX_POINT('',#45108);
#6782=VERTEX_POINT('',#45109);
#6783=VERTEX_POINT('',#45133);
#6784=VERTEX_POINT('',#45134);
#6785=VERTEX_POINT('',#45157);
#6786=VERTEX_POINT('',#45158);
#6787=VERTEX_POINT('',#45182);
#6788=VERTEX_POINT('',#45183);
#6789=VERTEX_POINT('',#45207);
#6790=VERTEX_POINT('',#45208);
#6791=VERTEX_POINT('',#45231);
#6792=VERTEX_POINT('',#45232);
#6793=VERTEX_POINT('',#45255);
#6794=VERTEX_POINT('',#45256);
#6795=VERTEX_POINT('',#45281);
#6796=VERTEX_POINT('',#45282);
#6797=VERTEX_POINT('',#45305);
#6798=VERTEX_POINT('',#45306);
#6799=VERTEX_POINT('',#45329);
#6800=VERTEX_POINT('',#45330);
#6801=VERTEX_POINT('',#45355);
#6802=VERTEX_POINT('',#45356);
#6803=VERTEX_POINT('',#45379);
#6804=VERTEX_POINT('',#45380);
#6805=VERTEX_POINT('',#45382);
#6806=VERTEX_POINT('',#45387);
#6807=VERTEX_POINT('',#45398);
#6808=VERTEX_POINT('',#45410);
#6809=VERTEX_POINT('',#45412);
#6810=VERTEX_POINT('',#45416);
#6811=VERTEX_POINT('',#45419);
#6812=VERTEX_POINT('',#45422);
#6813=VERTEX_POINT('',#45426);
#6814=VERTEX_POINT('',#45427);
#6815=VERTEX_POINT('',#45429);
#6816=VERTEX_POINT('',#45431);
#6817=VERTEX_POINT('',#45435);
#6818=VERTEX_POINT('',#45437);
#6819=VERTEX_POINT('',#45441);
#6820=VERTEX_POINT('',#45445);
#6821=VERTEX_POINT('',#45449);
#6822=VERTEX_POINT('',#46717);
#6823=VERTEX_POINT('',#46720);
#6824=VERTEX_POINT('',#46725);
#6825=VERTEX_POINT('',#46730);
#6826=VERTEX_POINT('',#46732);
#6827=VERTEX_POINT('',#46735);
#6828=VERTEX_POINT('',#46737);
#6829=VERTEX_POINT('',#46742);
#6830=VERTEX_POINT('',#46746);
#6831=VERTEX_POINT('',#46749);
#6832=VERTEX_POINT('',#46757);
#6833=VERTEX_POINT('',#46759);
#6834=VERTEX_POINT('',#46763);
#6835=VERTEX_POINT('',#46765);
#6836=VERTEX_POINT('',#46772);
#6837=VERTEX_POINT('',#46774);
#6838=VERTEX_POINT('',#46778);
#6839=VERTEX_POINT('',#46780);
#6840=VERTEX_POINT('',#46787);
#6841=VERTEX_POINT('',#46788);
#6842=VERTEX_POINT('',#46790);
#6843=VERTEX_POINT('',#46792);
#6844=VERTEX_POINT('',#46796);
#6845=VERTEX_POINT('',#46797);
#6846=VERTEX_POINT('',#46799);
#6847=VERTEX_POINT('',#46801);
#6848=VERTEX_POINT('',#46814);
#6849=VERTEX_POINT('',#46815);
#6850=VERTEX_POINT('',#46817);
#6851=VERTEX_POINT('',#46819);
#6852=VERTEX_POINT('',#46823);
#6853=VERTEX_POINT('',#46825);
#6854=VERTEX_POINT('',#46829);
#6855=VERTEX_POINT('',#46831);
#6856=VERTEX_POINT('',#46841);
#6857=VERTEX_POINT('',#46842);
#6858=VERTEX_POINT('',#46844);
#6859=VERTEX_POINT('',#46864);
#6860=VERTEX_POINT('',#46883);
#6861=VERTEX_POINT('',#46884);
#6862=VERTEX_POINT('',#46931);
#6863=VERTEX_POINT('',#46932);
#6864=VERTEX_POINT('',#46982);
#6865=VERTEX_POINT('',#46983);
#6866=VERTEX_POINT('',#47033);
#6867=VERTEX_POINT('',#47034);
#6868=VERTEX_POINT('',#47081);
#6869=VERTEX_POINT('',#47082);
#6870=VERTEX_POINT('',#47129);
#6871=VERTEX_POINT('',#47130);
#6872=VERTEX_POINT('',#47183);
#6873=VERTEX_POINT('',#47184);
#6874=VERTEX_POINT('',#47231);
#6875=VERTEX_POINT('',#47232);
#6876=VERTEX_POINT('',#47279);
#6877=VERTEX_POINT('',#47280);
#6878=VERTEX_POINT('',#47330);
#6879=VERTEX_POINT('',#47331);
#6880=VERTEX_POINT('',#47381);
#6881=VERTEX_POINT('',#47382);
#6882=VERTEX_POINT('',#47429);
#6883=VERTEX_POINT('',#47430);
#6884=VERTEX_POINT('',#47477);
#6885=VERTEX_POINT('',#47478);
#6886=VERTEX_POINT('',#47531);
#6887=VERTEX_POINT('',#47532);
#6888=VERTEX_POINT('',#47579);
#6889=VERTEX_POINT('',#47580);
#6890=VERTEX_POINT('',#47627);
#6891=VERTEX_POINT('',#47628);
#6892=VERTEX_POINT('',#47678);
#6893=VERTEX_POINT('',#47679);
#6894=VERTEX_POINT('',#47729);
#6895=VERTEX_POINT('',#47730);
#6896=VERTEX_POINT('',#47777);
#6897=VERTEX_POINT('',#47778);
#6898=VERTEX_POINT('',#47825);
#6899=VERTEX_POINT('',#47826);
#6900=VERTEX_POINT('',#47879);
#6901=VERTEX_POINT('',#47880);
#6902=VERTEX_POINT('',#47927);
#6903=VERTEX_POINT('',#47928);
#6904=VERTEX_POINT('',#47975);
#6905=VERTEX_POINT('',#47976);
#6906=VERTEX_POINT('',#48026);
#6907=VERTEX_POINT('',#48027);
#6908=VERTEX_POINT('',#48077);
#6909=VERTEX_POINT('',#48078);
#6910=VERTEX_POINT('',#48125);
#6911=VERTEX_POINT('',#48126);
#6912=VERTEX_POINT('',#48173);
#6913=VERTEX_POINT('',#48174);
#6914=VERTEX_POINT('',#48227);
#6915=VERTEX_POINT('',#48228);
#6916=VERTEX_POINT('',#48275);
#6917=VERTEX_POINT('',#48276);
#6918=VERTEX_POINT('',#48323);
#6919=VERTEX_POINT('',#48324);
#6920=VERTEX_POINT('',#48374);
#6921=VERTEX_POINT('',#48375);
#6922=VERTEX_POINT('',#48425);
#6923=VERTEX_POINT('',#48426);
#6924=VERTEX_POINT('',#48473);
#6925=VERTEX_POINT('',#48474);
#6926=VERTEX_POINT('',#48521);
#6927=VERTEX_POINT('',#48522);
#6928=VERTEX_POINT('',#48575);
#6929=VERTEX_POINT('',#48576);
#6930=VERTEX_POINT('',#48623);
#6931=VERTEX_POINT('',#48624);
#6932=VERTEX_POINT('',#48671);
#6933=VERTEX_POINT('',#48672);
#6934=VERTEX_POINT('',#48722);
#6935=VERTEX_POINT('',#48723);
#6936=VERTEX_POINT('',#48773);
#6937=VERTEX_POINT('',#48774);
#6938=VERTEX_POINT('',#48821);
#6939=VERTEX_POINT('',#48822);
#6940=VERTEX_POINT('',#48869);
#6941=VERTEX_POINT('',#48870);
#6942=VERTEX_POINT('',#48923);
#6943=VERTEX_POINT('',#48924);
#6944=VERTEX_POINT('',#48971);
#6945=VERTEX_POINT('',#48972);
#6946=VERTEX_POINT('',#49019);
#6947=VERTEX_POINT('',#49020);
#6948=VERTEX_POINT('',#49070);
#6949=VERTEX_POINT('',#49071);
#6950=VERTEX_POINT('',#49121);
#6951=VERTEX_POINT('',#49122);
#6952=VERTEX_POINT('',#49169);
#6953=VERTEX_POINT('',#49170);
#6954=VERTEX_POINT('',#49217);
#6955=VERTEX_POINT('',#49218);
#6956=VERTEX_POINT('',#49271);
#6957=VERTEX_POINT('',#49272);
#6958=VERTEX_POINT('',#49319);
#6959=VERTEX_POINT('',#49320);
#6960=VERTEX_POINT('',#49367);
#6961=VERTEX_POINT('',#49368);
#6962=VERTEX_POINT('',#49418);
#6963=VERTEX_POINT('',#49419);
#6964=VERTEX_POINT('',#49466);
#6965=VERTEX_POINT('',#49467);
#6966=VERTEX_POINT('',#49514);
#6967=VERTEX_POINT('',#49515);
#6968=VERTEX_POINT('',#49562);
#6969=VERTEX_POINT('',#49563);
#6970=VERTEX_POINT('',#49616);
#6971=VERTEX_POINT('',#49617);
#6972=VERTEX_POINT('',#49664);
#6973=VERTEX_POINT('',#49665);
#6974=VERTEX_POINT('',#49712);
#6975=VERTEX_POINT('',#49713);
#6976=VERTEX_POINT('',#49766);
#6977=VERTEX_POINT('',#49767);
#6978=VERTEX_POINT('',#49814);
#6979=VERTEX_POINT('',#49815);
#6980=VERTEX_POINT('',#49862);
#6981=VERTEX_POINT('',#49863);
#6982=VERTEX_POINT('',#49910);
#6983=VERTEX_POINT('',#49911);
#6984=VERTEX_POINT('',#49964);
#6985=VERTEX_POINT('',#49965);
#6986=VERTEX_POINT('',#50012);
#6987=VERTEX_POINT('',#50013);
#6988=VERTEX_POINT('',#50060);
#6989=VERTEX_POINT('',#50061);
#6990=VERTEX_POINT('',#50114);
#6991=VERTEX_POINT('',#50115);
#6992=VERTEX_POINT('',#50162);
#6993=VERTEX_POINT('',#50163);
#6994=VERTEX_POINT('',#50210);
#6995=VERTEX_POINT('',#50211);
#6996=VERTEX_POINT('',#50258);
#6997=VERTEX_POINT('',#50259);
#6998=VERTEX_POINT('',#50312);
#6999=VERTEX_POINT('',#50313);
#7000=VERTEX_POINT('',#50360);
#7001=VERTEX_POINT('',#50361);
#7002=VERTEX_POINT('',#50408);
#7003=VERTEX_POINT('',#50409);
#7004=VERTEX_POINT('',#50462);
#7005=VERTEX_POINT('',#50463);
#7006=VERTEX_POINT('',#50510);
#7007=VERTEX_POINT('',#50511);
#7008=VERTEX_POINT('',#50558);
#7009=VERTEX_POINT('',#50559);
#7010=VERTEX_POINT('',#50606);
#7011=VERTEX_POINT('',#50607);
#7012=VERTEX_POINT('',#50660);
#7013=VERTEX_POINT('',#50661);
#7014=VERTEX_POINT('',#50708);
#7015=VERTEX_POINT('',#50710);
#7016=VERTEX_POINT('',#50712);
#7017=VERTEX_POINT('',#50714);
#7018=VERTEX_POINT('',#50734);
#7019=VERTEX_POINT('',#50736);
#7020=VERTEX_POINT('',#50758);
#7021=VERTEX_POINT('',#50759);
#7022=VERTEX_POINT('',#50761);
#7023=VERTEX_POINT('',#50772);
#7024=VERTEX_POINT('',#50782);
#7025=VERTEX_POINT('',#50783);
#7026=VERTEX_POINT('',#50807);
#7027=VERTEX_POINT('',#50808);
#7028=VERTEX_POINT('',#50831);
#7029=VERTEX_POINT('',#50832);
#7030=VERTEX_POINT('',#50856);
#7031=VERTEX_POINT('',#50857);
#7032=VERTEX_POINT('',#50881);
#7033=VERTEX_POINT('',#50882);
#7034=VERTEX_POINT('',#50905);
#7035=VERTEX_POINT('',#50906);
#7036=VERTEX_POINT('',#50929);
#7037=VERTEX_POINT('',#50930);
#7038=VERTEX_POINT('',#50954);
#7039=VERTEX_POINT('',#50955);
#7040=VERTEX_POINT('',#50979);
#7041=VERTEX_POINT('',#50980);
#7042=VERTEX_POINT('',#51003);
#7043=VERTEX_POINT('',#51004);
#7044=VERTEX_POINT('',#51028);
#7045=VERTEX_POINT('',#51029);
#7046=VERTEX_POINT('',#51053);
#7047=VERTEX_POINT('',#51054);
#7048=VERTEX_POINT('',#51077);
#7049=VERTEX_POINT('',#51078);
#7050=VERTEX_POINT('',#51101);
#7051=VERTEX_POINT('',#51102);
#7052=VERTEX_POINT('',#51126);
#7053=VERTEX_POINT('',#51127);
#7054=VERTEX_POINT('',#51151);
#7055=VERTEX_POINT('',#51152);
#7056=VERTEX_POINT('',#51175);
#7057=VERTEX_POINT('',#51176);
#7058=VERTEX_POINT('',#51200);
#7059=VERTEX_POINT('',#51201);
#7060=VERTEX_POINT('',#51225);
#7061=VERTEX_POINT('',#51226);
#7062=VERTEX_POINT('',#51249);
#7063=VERTEX_POINT('',#51250);
#7064=VERTEX_POINT('',#51273);
#7065=VERTEX_POINT('',#51274);
#7066=VERTEX_POINT('',#51298);
#7067=VERTEX_POINT('',#51299);
#7068=VERTEX_POINT('',#51323);
#7069=VERTEX_POINT('',#51324);
#7070=VERTEX_POINT('',#51347);
#7071=VERTEX_POINT('',#51348);
#7072=VERTEX_POINT('',#51372);
#7073=VERTEX_POINT('',#51373);
#7074=VERTEX_POINT('',#51409);
#7075=VERTEX_POINT('',#51410);
#7076=VERTEX_POINT('',#51445);
#7077=VERTEX_POINT('',#51446);
#7078=VERTEX_POINT('',#51470);
#7079=VERTEX_POINT('',#51471);
#7080=VERTEX_POINT('',#51494);
#7081=VERTEX_POINT('',#51495);
#7082=VERTEX_POINT('',#51519);
#7083=VERTEX_POINT('',#51520);
#7084=VERTEX_POINT('',#51543);
#7085=VERTEX_POINT('',#51544);
#7086=VERTEX_POINT('',#51568);
#7087=VERTEX_POINT('',#51569);
#7088=VERTEX_POINT('',#51593);
#7089=VERTEX_POINT('',#51594);
#7090=VERTEX_POINT('',#51617);
#7091=VERTEX_POINT('',#51618);
#7092=VERTEX_POINT('',#51642);
#7093=VERTEX_POINT('',#51643);
#7094=VERTEX_POINT('',#51666);
#7095=VERTEX_POINT('',#51667);
#7096=VERTEX_POINT('',#51691);
#7097=VERTEX_POINT('',#51692);
#7098=VERTEX_POINT('',#51715);
#7099=VERTEX_POINT('',#51716);
#7100=VERTEX_POINT('',#51740);
#7101=VERTEX_POINT('',#51741);
#7102=VERTEX_POINT('',#51765);
#7103=VERTEX_POINT('',#51766);
#7104=VERTEX_POINT('',#51789);
#7105=VERTEX_POINT('',#51790);
#7106=VERTEX_POINT('',#51814);
#7107=VERTEX_POINT('',#51815);
#7108=VERTEX_POINT('',#51838);
#7109=VERTEX_POINT('',#51839);
#7110=VERTEX_POINT('',#51863);
#7111=VERTEX_POINT('',#51864);
#7112=VERTEX_POINT('',#51887);
#7113=VERTEX_POINT('',#51888);
#7114=VERTEX_POINT('',#51912);
#7115=VERTEX_POINT('',#51913);
#7116=VERTEX_POINT('',#51937);
#7117=VERTEX_POINT('',#51938);
#7118=VERTEX_POINT('',#51961);
#7119=VERTEX_POINT('',#51962);
#7120=VERTEX_POINT('',#51986);
#7121=VERTEX_POINT('',#51987);
#7122=VERTEX_POINT('',#52010);
#7123=VERTEX_POINT('',#52011);
#7124=VERTEX_POINT('',#52035);
#7125=VERTEX_POINT('',#52036);
#7126=VERTEX_POINT('',#52059);
#7127=VERTEX_POINT('',#52060);
#7128=VERTEX_POINT('',#52084);
#7129=VERTEX_POINT('',#52085);
#7130=VERTEX_POINT('',#52109);
#7131=VERTEX_POINT('',#52110);
#7132=VERTEX_POINT('',#52133);
#7133=VERTEX_POINT('',#52134);
#7134=VERTEX_POINT('',#52158);
#7135=VERTEX_POINT('',#52159);
#7136=VERTEX_POINT('',#52182);
#7137=VERTEX_POINT('',#52183);
#7138=VERTEX_POINT('',#52207);
#7139=VERTEX_POINT('',#52208);
#7140=VERTEX_POINT('',#52231);
#7141=VERTEX_POINT('',#52232);
#7142=VERTEX_POINT('',#52256);
#7143=VERTEX_POINT('',#52257);
#7144=VERTEX_POINT('',#52281);
#7145=VERTEX_POINT('',#52282);
#7146=VERTEX_POINT('',#52305);
#7147=VERTEX_POINT('',#52306);
#7148=VERTEX_POINT('',#52330);
#7149=VERTEX_POINT('',#52331);
#7150=VERTEX_POINT('',#52354);
#7151=VERTEX_POINT('',#52355);
#7152=VERTEX_POINT('',#52379);
#7153=VERTEX_POINT('',#52380);
#7154=VERTEX_POINT('',#52403);
#7155=VERTEX_POINT('',#52404);
#7156=VERTEX_POINT('',#52428);
#7157=VERTEX_POINT('',#52429);
#7158=VERTEX_POINT('',#52453);
#7159=VERTEX_POINT('',#52454);
#7160=VERTEX_POINT('',#52477);
#7161=VERTEX_POINT('',#52478);
#7162=VERTEX_POINT('',#52502);
#7163=VERTEX_POINT('',#52503);
#7164=VERTEX_POINT('',#52526);
#7165=VERTEX_POINT('',#52527);
#7166=VERTEX_POINT('',#52551);
#7167=VERTEX_POINT('',#52552);
#7168=VERTEX_POINT('',#52575);
#7169=VERTEX_POINT('',#52576);
#7170=VERTEX_POINT('',#52600);
#7171=VERTEX_POINT('',#52601);
#7172=VERTEX_POINT('',#52625);
#7173=VERTEX_POINT('',#52626);
#7174=VERTEX_POINT('',#52649);
#7175=VERTEX_POINT('',#52650);
#7176=VERTEX_POINT('',#52674);
#7177=VERTEX_POINT('',#52675);
#7178=VERTEX_POINT('',#52698);
#7179=VERTEX_POINT('',#52699);
#7180=VERTEX_POINT('',#52723);
#7181=VERTEX_POINT('',#52724);
#7182=VERTEX_POINT('',#52747);
#7183=VERTEX_POINT('',#52821);
#7184=VERTEX_POINT('',#53104);
#7185=VERTEX_POINT('',#53112);
#7186=VERTEX_POINT('',#53122);
#7187=VERTEX_POINT('',#53124);
#7188=VERTEX_POINT('',#53129);
#7189=VERTEX_POINT('',#53132);
#7190=VERTEX_POINT('',#57498);
#7191=VERTEX_POINT('',#57500);
#7192=VERTEX_POINT('',#57504);
#7193=VERTEX_POINT('',#57506);
#7194=VERTEX_POINT('',#57510);
#7195=VERTEX_POINT('',#57512);
#7196=VERTEX_POINT('',#57516);
#7197=VERTEX_POINT('',#57518);
#7198=VERTEX_POINT('',#57522);
#7199=VERTEX_POINT('',#57524);
#7200=VERTEX_POINT('',#57528);
#7201=VERTEX_POINT('',#57530);
#7202=VERTEX_POINT('',#57534);
#7203=VERTEX_POINT('',#57536);
#7204=VERTEX_POINT('',#57539);
#7205=VERTEX_POINT('',#57544);
#7206=VERTEX_POINT('',#57550);
#7207=VERTEX_POINT('',#57552);
#7208=VERTEX_POINT('',#57556);
#7209=VERTEX_POINT('',#57558);
#7210=VERTEX_POINT('',#57565);
#7211=VERTEX_POINT('',#57566);
#7212=VERTEX_POINT('',#57568);
#7213=VERTEX_POINT('',#57570);
#7214=VERTEX_POINT('',#57574);
#7215=VERTEX_POINT('',#57575);
#7216=VERTEX_POINT('',#57577);
#7217=VERTEX_POINT('',#57579);
#7218=VERTEX_POINT('',#57592);
#7219=VERTEX_POINT('',#57593);
#7220=VERTEX_POINT('',#57595);
#7221=VERTEX_POINT('',#57606);
#7222=VERTEX_POINT('',#57616);
#7223=VERTEX_POINT('',#57617);
#7224=VERTEX_POINT('',#57664);
#7225=VERTEX_POINT('',#57665);
#7226=VERTEX_POINT('',#57712);
#7227=VERTEX_POINT('',#57713);
#7228=VERTEX_POINT('',#57766);
#7229=VERTEX_POINT('',#57767);
#7230=VERTEX_POINT('',#57814);
#7231=VERTEX_POINT('',#57815);
#7232=VERTEX_POINT('',#57862);
#7233=VERTEX_POINT('',#57863);
#7234=VERTEX_POINT('',#57916);
#7235=VERTEX_POINT('',#57917);
#7236=VERTEX_POINT('',#57964);
#7237=VERTEX_POINT('',#57965);
#7238=VERTEX_POINT('',#58012);
#7239=VERTEX_POINT('',#58013);
#7240=VERTEX_POINT('',#58066);
#7241=VERTEX_POINT('',#58067);
#7242=VERTEX_POINT('',#58114);
#7243=VERTEX_POINT('',#58115);
#7244=VERTEX_POINT('',#58162);
#7245=VERTEX_POINT('',#58163);
#7246=VERTEX_POINT('',#58216);
#7247=VERTEX_POINT('',#58217);
#7248=VERTEX_POINT('',#58264);
#7249=VERTEX_POINT('',#58265);
#7250=VERTEX_POINT('',#58312);
#7251=VERTEX_POINT('',#58313);
#7252=VERTEX_POINT('',#58366);
#7253=VERTEX_POINT('',#58367);
#7254=VERTEX_POINT('',#58414);
#7255=VERTEX_POINT('',#58415);
#7256=VERTEX_POINT('',#58462);
#7257=VERTEX_POINT('',#58463);
#7258=VERTEX_POINT('',#58465);
#7259=VERTEX_POINT('',#58472);
#7260=VERTEX_POINT('',#58479);
#7261=VERTEX_POINT('',#58480);
#7262=VERTEX_POINT('',#58504);
#7263=VERTEX_POINT('',#58505);
#7264=VERTEX_POINT('',#58528);
#7265=VERTEX_POINT('',#58529);
#7266=VERTEX_POINT('',#58553);
#7267=VERTEX_POINT('',#58554);
#7268=VERTEX_POINT('',#58578);
#7269=VERTEX_POINT('',#58579);
#7270=VERTEX_POINT('',#58602);
#7271=VERTEX_POINT('',#58603);
#7272=VERTEX_POINT('',#58627);
#7273=VERTEX_POINT('',#58628);
#7274=VERTEX_POINT('',#58652);
#7275=VERTEX_POINT('',#58653);
#7276=VERTEX_POINT('',#58676);
#7277=VERTEX_POINT('',#58677);
#7278=VERTEX_POINT('',#58701);
#7279=VERTEX_POINT('',#58702);
#7280=VERTEX_POINT('',#58726);
#7281=VERTEX_POINT('',#58727);
#7282=VERTEX_POINT('',#58750);
#7283=VERTEX_POINT('',#58751);
#7284=VERTEX_POINT('',#58775);
#7285=VERTEX_POINT('',#58776);
#7286=VERTEX_POINT('',#58800);
#7287=VERTEX_POINT('',#58801);
#7288=VERTEX_POINT('',#58824);
#7289=VERTEX_POINT('',#58825);
#7290=VERTEX_POINT('',#58849);
#7291=VERTEX_POINT('',#58850);
#7292=VERTEX_POINT('',#58874);
#7293=VERTEX_POINT('',#58875);
#7294=VERTEX_POINT('',#58898);
#7295=VERTEX_POINT('',#58899);
#7296=VERTEX_POINT('',#58901);
#7297=VERTEX_POINT('',#58903);
#7298=VERTEX_POINT('',#58907);
#7299=VERTEX_POINT('',#58909);
#7300=VERTEX_POINT('',#58913);
#7301=VERTEX_POINT('',#58915);
#7302=VERTEX_POINT('',#58919);
#7303=VERTEX_POINT('',#58921);
#7304=VERTEX_POINT('',#58925);
#7305=VERTEX_POINT('',#58927);
#7306=VERTEX_POINT('',#59410);
#7307=VERTEX_POINT('',#59521);
#7308=VERTEX_POINT('',#59623);
#7309=VERTEX_POINT('',#60109);
#7310=VERTEX_POINT('',#60314);
#7311=VERTEX_POINT('',#60316);
#7312=VERTEX_POINT('',#60319);
#7313=VERTEX_POINT('',#60323);
#7314=VERTEX_POINT('',#60327);
#7315=VERTEX_POINT('',#60329);
#7316=VERTEX_POINT('',#60332);
#7317=VERTEX_POINT('',#60336);
#7318=VERTEX_POINT('',#60340);
#7319=VERTEX_POINT('',#60342);
#7320=VERTEX_POINT('',#60345);
#7321=VERTEX_POINT('',#60349);
#7322=VERTEX_POINT('',#60353);
#7323=VERTEX_POINT('',#60355);
#7324=VERTEX_POINT('',#60358);
#7325=VERTEX_POINT('',#60362);
#7326=VERTEX_POINT('',#60366);
#7327=VERTEX_POINT('',#60368);
#7328=VERTEX_POINT('',#60372);
#7329=VERTEX_POINT('',#60374);
#7330=VERTEX_POINT('',#60381);
#7331=VERTEX_POINT('',#60383);
#7332=VERTEX_POINT('',#60387);
#7333=VERTEX_POINT('',#60391);
#7334=VERTEX_POINT('',#60393);
#7335=VERTEX_POINT('',#60397);
#7336=VERTEX_POINT('',#60404);
#7337=VERTEX_POINT('',#60406);
#7338=VERTEX_POINT('',#60410);
#7339=VERTEX_POINT('',#60414);
#7340=VERTEX_POINT('',#60418);
#7341=VERTEX_POINT('',#60420);
#7342=VERTEX_POINT('',#60427);
#7343=VERTEX_POINT('',#60428);
#7344=VERTEX_POINT('',#60432);
#7345=VERTEX_POINT('',#60433);
#7346=VERTEX_POINT('',#60460);
#7347=VERTEX_POINT('',#60462);
#7348=VERTEX_POINT('',#60475);
#7349=VERTEX_POINT('',#60477);
#7350=VERTEX_POINT('',#60494);
#7351=VERTEX_POINT('',#60496);
#7352=VERTEX_POINT('',#60498);
#7353=VERTEX_POINT('',#60511);
#7354=VERTEX_POINT('',#60513);
#7355=VERTEX_POINT('',#60536);
#7356=VERTEX_POINT('',#60538);
#7357=VERTEX_POINT('',#60561);
#7358=VERTEX_POINT('',#60563);
#7359=VERTEX_POINT('',#60586);
#7360=VERTEX_POINT('',#60588);
#7361=VERTEX_POINT('',#60595);
#7362=VERTEX_POINT('',#60616);
#7363=VERTEX_POINT('',#60618);
#7364=VERTEX_POINT('',#60631);
#7365=VERTEX_POINT('',#60646);
#7366=VERTEX_POINT('',#60648);
#7367=VERTEX_POINT('',#60661);
#7368=VERTEX_POINT('',#60675);
#7369=VERTEX_POINT('',#60677);
#7370=VERTEX_POINT('',#60698);
#7371=VERTEX_POINT('',#60705);
#7372=VERTEX_POINT('',#60707);
#7373=VERTEX_POINT('',#60730);
#7374=VERTEX_POINT('',#60732);
#7375=VERTEX_POINT('',#60755);
#7376=VERTEX_POINT('',#60757);
#7377=VERTEX_POINT('',#60780);
#7378=VERTEX_POINT('',#60795);
#7379=VERTEX_POINT('',#60799);
#7380=VERTEX_POINT('',#60827);
#7381=VERTEX_POINT('',#60830);
#7382=VERTEX_POINT('',#60834);
#7383=VERTEX_POINT('',#60861);
#7384=VERTEX_POINT('',#60863);
#7385=VERTEX_POINT('',#60867);
#7386=VERTEX_POINT('',#60871);
#7387=VERTEX_POINT('',#60872);
#7388=VERTEX_POINT('',#60904);
#7389=VERTEX_POINT('',#60907);
#7390=VERTEX_POINT('',#60911);
#7391=VERTEX_POINT('',#60912);
#7392=VERTEX_POINT('',#60944);
#7393=VERTEX_POINT('',#60947);
#7394=VERTEX_POINT('',#60951);
#7395=VERTEX_POINT('',#60952);
#7396=VERTEX_POINT('',#60982);
#7397=VERTEX_POINT('',#60985);
#7398=VERTEX_POINT('',#60989);
#7399=VERTEX_POINT('',#60990);
#7400=VERTEX_POINT('',#61022);
#7401=VERTEX_POINT('',#61025);
#7402=VERTEX_POINT('',#61029);
#7403=VERTEX_POINT('',#61030);
#7404=VERTEX_POINT('',#61062);
#7405=VERTEX_POINT('',#61065);
#7406=VERTEX_POINT('',#61067);
#7407=VERTEX_POINT('',#61071);
#7408=VERTEX_POINT('',#61099);
#7409=VERTEX_POINT('',#61102);
#7410=VERTEX_POINT('',#61106);
#7411=VERTEX_POINT('',#61134);
#7412=VERTEX_POINT('',#61137);
#7413=VERTEX_POINT('',#61141);
#7414=VERTEX_POINT('',#61169);
#7415=VERTEX_POINT('',#61172);
#7416=VERTEX_POINT('',#61176);
#7417=VERTEX_POINT('',#61204);
#7418=VERTEX_POINT('',#61207);
#7419=VERTEX_POINT('',#61215);
#7420=VERTEX_POINT('',#61217);
#7421=VERTEX_POINT('',#61221);
#7422=VERTEX_POINT('',#61223);
#7423=VERTEX_POINT('',#61230);
#7424=VERTEX_POINT('',#61231);
#7425=VERTEX_POINT('',#61233);
#7426=VERTEX_POINT('',#61244);
#7427=VERTEX_POINT('',#61254);
#7428=VERTEX_POINT('',#61255);
#7429=VERTEX_POINT('',#61302);
#7430=VERTEX_POINT('',#61303);
#7431=VERTEX_POINT('',#61350);
#7432=VERTEX_POINT('',#61351);
#7433=VERTEX_POINT('',#61404);
#7434=VERTEX_POINT('',#61405);
#7435=VERTEX_POINT('',#61452);
#7436=VERTEX_POINT('',#61453);
#7437=VERTEX_POINT('',#61500);
#7438=VERTEX_POINT('',#61501);
#7439=VERTEX_POINT('',#61548);
#7440=VERTEX_POINT('',#61549);
#7441=VERTEX_POINT('',#61602);
#7442=VERTEX_POINT('',#61603);
#7443=VERTEX_POINT('',#61650);
#7444=VERTEX_POINT('',#61651);
#7445=VERTEX_POINT('',#61698);
#7446=VERTEX_POINT('',#61699);
#7447=VERTEX_POINT('',#61752);
#7448=VERTEX_POINT('',#61753);
#7449=VERTEX_POINT('',#61800);
#7450=VERTEX_POINT('',#61801);
#7451=VERTEX_POINT('',#61848);
#7452=VERTEX_POINT('',#61849);
#7453=VERTEX_POINT('',#61899);
#7454=VERTEX_POINT('',#61900);
#7455=VERTEX_POINT('',#61950);
#7456=VERTEX_POINT('',#61951);
#7457=VERTEX_POINT('',#61998);
#7458=VERTEX_POINT('',#61999);
#7459=VERTEX_POINT('',#62001);
#7460=VERTEX_POINT('',#62010);
#7461=VERTEX_POINT('',#62020);
#7462=VERTEX_POINT('',#62021);
#7463=VERTEX_POINT('',#62044);
#7464=VERTEX_POINT('',#62045);
#7465=VERTEX_POINT('',#62068);
#7466=VERTEX_POINT('',#62069);
#7467=VERTEX_POINT('',#62094);
#7468=VERTEX_POINT('',#62095);
#7469=VERTEX_POINT('',#62118);
#7470=VERTEX_POINT('',#62119);
#7471=VERTEX_POINT('',#62142);
#7472=VERTEX_POINT('',#62143);
#7473=VERTEX_POINT('',#62167);
#7474=VERTEX_POINT('',#62168);
#7475=VERTEX_POINT('',#62192);
#7476=VERTEX_POINT('',#62193);
#7477=VERTEX_POINT('',#62216);
#7478=VERTEX_POINT('',#62217);
#7479=VERTEX_POINT('',#62241);
#7480=VERTEX_POINT('',#62242);
#7481=VERTEX_POINT('',#62266);
#7482=VERTEX_POINT('',#62267);
#7483=VERTEX_POINT('',#62290);
#7484=VERTEX_POINT('',#62291);
#7485=VERTEX_POINT('',#62314);
#7486=VERTEX_POINT('',#62315);
#7487=VERTEX_POINT('',#62339);
#7488=VERTEX_POINT('',#62340);
#7489=VERTEX_POINT('',#62364);
#7490=VERTEX_POINT('',#62365);
#7491=VERTEX_POINT('',#62388);
#7492=VERTEX_POINT('',#62516);
#7493=VERTEX_POINT('',#62575);
#7494=VERTEX_POINT('',#62680);
#7495=VERTEX_POINT('',#63107);
#7496=VERTEX_POINT('',#63215);
#7497=VERTEX_POINT('',#63761);
#7498=VERTEX_POINT('',#63762);
#7499=VERTEX_POINT('',#63764);
#7500=VERTEX_POINT('',#63766);
#7501=VERTEX_POINT('',#63770);
#7502=VERTEX_POINT('',#63772);
#7503=VERTEX_POINT('',#63776);
#7504=VERTEX_POINT('',#63778);
#7505=VERTEX_POINT('',#63782);
#7506=VERTEX_POINT('',#63784);
#7507=VERTEX_POINT('',#63788);
#7508=VERTEX_POINT('',#63790);
#7509=VERTEX_POINT('',#63798);
#7510=VERTEX_POINT('',#63801);
#7511=EDGE_CURVE('',#5949,#5950,#4423,.T.);
#7512=EDGE_CURVE('',#5949,#5951,#4424,.T.);
#7513=EDGE_CURVE('',#5952,#5951,#4425,.T.);
#7514=EDGE_CURVE('',#5952,#5950,#4426,.T.);
#7515=EDGE_CURVE('',#5950,#5953,#2380,.T.);
#7516=EDGE_CURVE('',#5954,#5952,#4427,.T.);
#7517=EDGE_CURVE('',#5955,#5954,#4428,.T.);
#7518=EDGE_CURVE('',#5953,#5955,#2381,.T.);
#7519=EDGE_CURVE('',#5955,#5956,#4429,.T.);
#7520=EDGE_CURVE('',#5954,#5957,#4430,.T.);
#7521=EDGE_CURVE('',#5957,#5956,#4431,.T.);
#7522=EDGE_CURVE('',#5951,#5957,#4432,.T.);
#7523=EDGE_CURVE('',#5956,#5958,#2382,.T.);
#7524=EDGE_CURVE('',#5958,#5949,#2383,.T.);
#7525=EDGE_CURVE('',#5959,#5960,#2384,.T.);
#7526=EDGE_CURVE('',#5960,#5959,#2385,.T.);
#7527=EDGE_CURVE('',#5961,#5959,#4433,.T.);
#7528=EDGE_CURVE('',#5961,#5962,#2386,.T.);
#7529=EDGE_CURVE('',#5960,#5962,#4434,.T.);
#7530=EDGE_CURVE('',#5962,#5963,#2387,.T.);
#7531=EDGE_CURVE('',#5963,#5964,#4435,.T.);
#7532=EDGE_CURVE('',#5965,#5964,#2388,.T.);
#7533=EDGE_CURVE('',#5965,#5966,#4436,.T.);
#7534=EDGE_CURVE('',#5966,#5966,#2389,.T.);
#7535=EDGE_CURVE('',#5967,#5965,#2390,.T.);
#7536=EDGE_CURVE('',#5967,#5968,#4437,.T.);
#7537=EDGE_CURVE('',#5968,#5961,#2391,.T.);
#7538=EDGE_CURVE('',#5969,#5969,#2392,.T.);
#7539=EDGE_CURVE('',#5969,#5970,#4438,.T.);
#7540=EDGE_CURVE('',#5970,#5970,#2393,.T.);
#7541=EDGE_CURVE('',#5971,#5971,#2394,.T.);
#7542=EDGE_CURVE('',#5971,#5972,#4439,.T.);
#7543=EDGE_CURVE('',#5972,#5972,#2395,.T.);
#7544=EDGE_CURVE('',#5973,#5973,#2396,.T.);
#7545=EDGE_CURVE('',#5973,#5974,#4440,.T.);
#7546=EDGE_CURVE('',#5974,#5974,#2397,.T.);
#7547=EDGE_CURVE('',#5975,#5975,#2398,.T.);
#7548=EDGE_CURVE('',#5975,#5976,#4441,.T.);
#7549=EDGE_CURVE('',#5976,#5976,#2399,.T.);
#7550=EDGE_CURVE('',#5977,#5977,#2400,.T.);
#7551=EDGE_CURVE('',#5977,#5978,#4442,.T.);
#7552=EDGE_CURVE('',#5978,#5978,#2401,.T.);
#7553=EDGE_CURVE('',#5979,#5979,#2402,.T.);
#7554=EDGE_CURVE('',#5979,#5980,#4443,.T.);
#7555=EDGE_CURVE('',#5980,#5980,#2403,.T.);
#7556=EDGE_CURVE('',#5981,#5967,#4444,.T.);
#7557=EDGE_CURVE('',#5982,#5981,#4445,.T.);
#7558=EDGE_CURVE('',#5982,#5968,#4446,.T.);
#7559=EDGE_CURVE('',#5983,#5982,#4447,.T.);
#7560=EDGE_CURVE('',#5984,#5981,#4448,.T.);
#7561=EDGE_CURVE('',#5983,#5984,#4449,.T.);
#7562=EDGE_CURVE('',#5963,#5983,#4450,.T.);
#7563=EDGE_CURVE('',#5964,#5984,#4451,.T.);
#7564=EDGE_CURVE('',#5985,#5985,#2404,.T.);
#7565=EDGE_CURVE('',#5986,#5986,#2405,.T.);
#7566=EDGE_CURVE('',#5987,#5987,#2406,.T.);
#7567=EDGE_CURVE('',#5985,#5986,#4452,.T.);
#7568=EDGE_CURVE('',#5987,#5988,#4453,.T.);
#7569=EDGE_CURVE('',#5988,#5988,#2407,.T.);
#7570=EDGE_CURVE('',#5989,#5989,#2408,.T.);
#7571=EDGE_CURVE('',#5989,#5953,#4454,.T.);
#7572=EDGE_CURVE('',#5958,#5990,#4455,.T.);
#7573=EDGE_CURVE('',#5990,#5990,#2409,.T.);
#7574=EDGE_CURVE('',#5991,#5992,#4456,.T.);
#7575=EDGE_CURVE('',#5993,#5992,#2410,.F.);
#7576=EDGE_CURVE('',#5993,#5991,#266,.T.);
#7577=EDGE_CURVE('',#5994,#5995,#4457,.T.);
#7578=EDGE_CURVE('',#5995,#5996,#267,.T.);
#7579=EDGE_CURVE('',#5992,#5996,#2411,.F.);
#7580=EDGE_CURVE('',#5991,#5994,#268,.T.);
#7581=EDGE_CURVE('',#5997,#5998,#4458,.T.);
#7582=EDGE_CURVE('',#5998,#5995,#269,.T.);
#7583=EDGE_CURVE('',#5994,#5997,#270,.T.);
#7584=EDGE_CURVE('',#5999,#6000,#4459,.T.);
#7585=EDGE_CURVE('',#6000,#5998,#271,.T.);
#7586=EDGE_CURVE('',#5997,#5999,#272,.T.);
#7587=EDGE_CURVE('',#6001,#6002,#4460,.T.);
#7588=EDGE_CURVE('',#6002,#6000,#273,.T.);
#7589=EDGE_CURVE('',#5999,#6001,#274,.T.);
#7590=EDGE_CURVE('',#6003,#6004,#4461,.T.);
#7591=EDGE_CURVE('',#6004,#6002,#275,.T.);
#7592=EDGE_CURVE('',#6001,#6003,#276,.T.);
#7593=EDGE_CURVE('',#6005,#6006,#4462,.T.);
#7594=EDGE_CURVE('',#6005,#6007,#277,.T.);
#7595=EDGE_CURVE('',#6008,#6007,#2412,.T.);
#7596=EDGE_CURVE('',#6008,#6006,#278,.T.);
#7597=EDGE_CURVE('',#6009,#6010,#4463,.T.);
#7598=EDGE_CURVE('',#6010,#6011,#279,.T.);
#7599=EDGE_CURVE('',#6012,#6011,#2413,.T.);
#7600=EDGE_CURVE('',#6009,#6012,#280,.T.);
#7601=EDGE_CURVE('',#6013,#6014,#4464,.T.);
#7602=EDGE_CURVE('',#6014,#6010,#281,.T.);
#7603=EDGE_CURVE('',#6013,#6009,#282,.T.);
#7604=EDGE_CURVE('',#6015,#6016,#4465,.T.);
#7605=EDGE_CURVE('',#6016,#6014,#283,.T.);
#7606=EDGE_CURVE('',#6015,#6013,#284,.T.);
#7607=EDGE_CURVE('',#6017,#6018,#4466,.T.);
#7608=EDGE_CURVE('',#6018,#6016,#285,.T.);
#7609=EDGE_CURVE('',#6017,#6015,#286,.T.);
#7610=EDGE_CURVE('',#6019,#6020,#4467,.T.);
#7611=EDGE_CURVE('',#6020,#6018,#287,.T.);
#7612=EDGE_CURVE('',#6019,#6017,#288,.T.);
#7613=EDGE_CURVE('',#6021,#6022,#4468,.T.);
#7614=EDGE_CURVE('',#6022,#6020,#289,.T.);
#7615=EDGE_CURVE('',#6021,#6019,#290,.T.);
#7616=EDGE_CURVE('',#6023,#6024,#4469,.T.);
#7617=EDGE_CURVE('',#6025,#6023,#291,.T.);
#7618=EDGE_CURVE('',#6026,#6025,#2414,.T.);
#7619=EDGE_CURVE('',#6026,#6024,#292,.T.);
#7620=EDGE_CURVE('',#6027,#6028,#4470,.T.);
#7621=EDGE_CURVE('',#6028,#6029,#293,.T.);
#7622=EDGE_CURVE('',#6029,#6030,#2415,.T.);
#7623=EDGE_CURVE('',#6030,#6031,#4471,.T.);
#7624=EDGE_CURVE('',#6031,#6031,#2416,.F.);
#7625=EDGE_CURVE('',#6030,#6032,#2417,.T.);
#7626=EDGE_CURVE('',#6032,#6027,#294,.T.);
#7627=EDGE_CURVE('',#6033,#6034,#4472,.T.);
#7628=EDGE_CURVE('',#6034,#6028,#295,.T.);
#7629=EDGE_CURVE('',#6027,#6033,#296,.T.);
#7630=EDGE_CURVE('',#6035,#6036,#4473,.T.);
#7631=EDGE_CURVE('',#6036,#6034,#297,.T.);
#7632=EDGE_CURVE('',#6033,#6035,#298,.T.);
#7633=EDGE_CURVE('',#6037,#6038,#4474,.T.);
#7634=EDGE_CURVE('',#6038,#6036,#299,.T.);
#7635=EDGE_CURVE('',#6035,#6037,#300,.T.);
#7636=EDGE_CURVE('',#6039,#6040,#4475,.T.);
#7637=EDGE_CURVE('',#6040,#6038,#301,.T.);
#7638=EDGE_CURVE('',#6037,#6039,#302,.T.);
#7639=EDGE_CURVE('',#6041,#6042,#4476,.T.);
#7640=EDGE_CURVE('',#6042,#6040,#303,.T.);
#7641=EDGE_CURVE('',#6039,#6041,#304,.T.);
#7642=EDGE_CURVE('',#6043,#6044,#4477,.T.);
#7643=EDGE_CURVE('',#6044,#6042,#305,.T.);
#7644=EDGE_CURVE('',#6041,#6043,#306,.T.);
#7645=EDGE_CURVE('',#6045,#6046,#4478,.T.);
#7646=EDGE_CURVE('',#6046,#6044,#307,.T.);
#7647=EDGE_CURVE('',#6043,#6045,#308,.T.);
#7648=EDGE_CURVE('',#6047,#6048,#4479,.T.);
#7649=EDGE_CURVE('',#6048,#6046,#309,.T.);
#7650=EDGE_CURVE('',#6045,#6047,#310,.T.);
#7651=EDGE_CURVE('',#6049,#6050,#4480,.T.);
#7652=EDGE_CURVE('',#6050,#6048,#311,.T.);
#7653=EDGE_CURVE('',#6047,#6049,#312,.T.);
#7654=EDGE_CURVE('',#6051,#6052,#4481,.T.);
#7655=EDGE_CURVE('',#6052,#6050,#313,.T.);
#7656=EDGE_CURVE('',#6049,#6051,#314,.T.);
#7657=EDGE_CURVE('',#6053,#6054,#4482,.T.);
#7658=EDGE_CURVE('',#6054,#6052,#315,.T.);
#7659=EDGE_CURVE('',#6051,#6053,#316,.T.);
#7660=EDGE_CURVE('',#6055,#6056,#4483,.T.);
#7661=EDGE_CURVE('',#6056,#6054,#317,.T.);
#7662=EDGE_CURVE('',#6053,#6055,#318,.T.);
#7663=EDGE_CURVE('',#6057,#6058,#4484,.T.);
#7664=EDGE_CURVE('',#6058,#6056,#319,.T.);
#7665=EDGE_CURVE('',#6055,#6057,#320,.T.);
#7666=EDGE_CURVE('',#6059,#6060,#4485,.T.);
#7667=EDGE_CURVE('',#6060,#6058,#321,.T.);
#7668=EDGE_CURVE('',#6057,#6059,#322,.T.);
#7669=EDGE_CURVE('',#6061,#6062,#4486,.T.);
#7670=EDGE_CURVE('',#6062,#6060,#323,.T.);
#7671=EDGE_CURVE('',#6059,#6061,#324,.T.);
#7672=EDGE_CURVE('',#6063,#6064,#4487,.T.);
#7673=EDGE_CURVE('',#6064,#6062,#325,.T.);
#7674=EDGE_CURVE('',#6061,#6063,#326,.T.);
#7675=EDGE_CURVE('',#6065,#6066,#4488,.T.);
#7676=EDGE_CURVE('',#6065,#6067,#327,.T.);
#7677=EDGE_CURVE('',#6068,#6067,#2418,.F.);
#7678=EDGE_CURVE('',#6068,#6066,#328,.T.);
#7679=EDGE_CURVE('',#6069,#6070,#4489,.T.);
#7680=EDGE_CURVE('',#6070,#6071,#329,.T.);
#7681=EDGE_CURVE('',#6072,#6071,#2419,.T.);
#7682=EDGE_CURVE('',#6069,#6072,#330,.T.);
#7683=EDGE_CURVE('',#6073,#6074,#4490,.T.);
#7684=EDGE_CURVE('',#6074,#6070,#331,.T.);
#7685=EDGE_CURVE('',#6073,#6069,#332,.T.);
#7686=EDGE_CURVE('',#6075,#6076,#4491,.T.);
#7687=EDGE_CURVE('',#6076,#6074,#333,.T.);
#7688=EDGE_CURVE('',#6075,#6073,#334,.T.);
#7689=EDGE_CURVE('',#6077,#6078,#4492,.T.);
#7690=EDGE_CURVE('',#6078,#6076,#335,.T.);
#7691=EDGE_CURVE('',#6077,#6075,#336,.T.);
#7692=EDGE_CURVE('',#6079,#6080,#4493,.T.);
#7693=EDGE_CURVE('',#6080,#6078,#337,.T.);
#7694=EDGE_CURVE('',#6079,#6077,#338,.T.);
#7695=EDGE_CURVE('',#6081,#6082,#4494,.T.);
#7696=EDGE_CURVE('',#6082,#6080,#339,.T.);
#7697=EDGE_CURVE('',#6081,#6079,#340,.T.);
#7698=EDGE_CURVE('',#6083,#6084,#4495,.T.);
#7699=EDGE_CURVE('',#6084,#6082,#341,.T.);
#7700=EDGE_CURVE('',#6083,#6081,#342,.T.);
#7701=EDGE_CURVE('',#6085,#6086,#4496,.T.);
#7702=EDGE_CURVE('',#6086,#6084,#343,.T.);
#7703=EDGE_CURVE('',#6085,#6083,#344,.T.);
#7704=EDGE_CURVE('',#6087,#6088,#4497,.T.);
#7705=EDGE_CURVE('',#6088,#6086,#345,.T.);
#7706=EDGE_CURVE('',#6087,#6085,#346,.T.);
#7707=EDGE_CURVE('',#6089,#6090,#4498,.T.);
#7708=EDGE_CURVE('',#6090,#6088,#347,.T.);
#7709=EDGE_CURVE('',#6089,#6087,#348,.T.);
#7710=EDGE_CURVE('',#6091,#6092,#4499,.T.);
#7711=EDGE_CURVE('',#6092,#6090,#349,.T.);
#7712=EDGE_CURVE('',#6091,#6089,#350,.T.);
#7713=EDGE_CURVE('',#6093,#6094,#4500,.T.);
#7714=EDGE_CURVE('',#6094,#6092,#351,.T.);
#7715=EDGE_CURVE('',#6093,#6091,#352,.T.);
#7716=EDGE_CURVE('',#6095,#6096,#4501,.T.);
#7717=EDGE_CURVE('',#6096,#6094,#353,.T.);
#7718=EDGE_CURVE('',#6095,#6093,#354,.T.);
#7719=EDGE_CURVE('',#6097,#6098,#4502,.T.);
#7720=EDGE_CURVE('',#6098,#6096,#355,.T.);
#7721=EDGE_CURVE('',#6097,#6095,#356,.T.);
#7722=EDGE_CURVE('',#6099,#6100,#4503,.T.);
#7723=EDGE_CURVE('',#6100,#6098,#357,.T.);
#7724=EDGE_CURVE('',#6099,#6097,#358,.T.);
#7725=EDGE_CURVE('',#6101,#6102,#4504,.T.);
#7726=EDGE_CURVE('',#6102,#6100,#359,.T.);
#7727=EDGE_CURVE('',#6101,#6099,#360,.T.);
#7728=EDGE_CURVE('',#6103,#6104,#4505,.T.);
#7729=EDGE_CURVE('',#6104,#6102,#361,.T.);
#7730=EDGE_CURVE('',#6103,#6101,#362,.T.);
#7731=EDGE_CURVE('',#6105,#6106,#4506,.T.);
#7732=EDGE_CURVE('',#6106,#6104,#363,.T.);
#7733=EDGE_CURVE('',#6105,#6103,#364,.T.);
#7734=EDGE_CURVE('',#6107,#6108,#4507,.T.);
#7735=EDGE_CURVE('',#6109,#6107,#365,.T.);
#7736=EDGE_CURVE('',#6110,#6109,#2420,.T.);
#7737=EDGE_CURVE('',#6110,#6108,#366,.T.);
#7738=EDGE_CURVE('',#6111,#6112,#4508,.T.);
#7739=EDGE_CURVE('',#6112,#6113,#367,.T.);
#7740=EDGE_CURVE('',#6113,#6114,#2421,.T.);
#7741=EDGE_CURVE('',#6114,#6115,#4509,.T.);
#7742=EDGE_CURVE('',#6115,#6115,#2422,.F.);
#7743=EDGE_CURVE('',#6114,#6116,#2423,.T.);
#7744=EDGE_CURVE('',#6116,#6111,#368,.T.);
#7745=EDGE_CURVE('',#6117,#6118,#4510,.T.);
#7746=EDGE_CURVE('',#6118,#6112,#369,.T.);
#7747=EDGE_CURVE('',#6111,#6117,#370,.T.);
#7748=EDGE_CURVE('',#6119,#6120,#4511,.T.);
#7749=EDGE_CURVE('',#6120,#6118,#371,.T.);
#7750=EDGE_CURVE('',#6117,#6119,#372,.T.);
#7751=EDGE_CURVE('',#6121,#6122,#4512,.T.);
#7752=EDGE_CURVE('',#6122,#6120,#373,.T.);
#7753=EDGE_CURVE('',#6119,#6121,#374,.T.);
#7754=EDGE_CURVE('',#6123,#6124,#4513,.T.);
#7755=EDGE_CURVE('',#6124,#6122,#375,.T.);
#7756=EDGE_CURVE('',#6121,#6123,#376,.T.);
#7757=EDGE_CURVE('',#6125,#6126,#4514,.T.);
#7758=EDGE_CURVE('',#6126,#6124,#377,.T.);
#7759=EDGE_CURVE('',#6123,#6125,#378,.T.);
#7760=EDGE_CURVE('',#6127,#6128,#4515,.T.);
#7761=EDGE_CURVE('',#6128,#6126,#379,.T.);
#7762=EDGE_CURVE('',#6125,#6127,#380,.T.);
#7763=EDGE_CURVE('',#6129,#6130,#4516,.T.);
#7764=EDGE_CURVE('',#6130,#6128,#381,.T.);
#7765=EDGE_CURVE('',#6127,#6129,#382,.T.);
#7766=EDGE_CURVE('',#6131,#6132,#4517,.T.);
#7767=EDGE_CURVE('',#6132,#6130,#383,.T.);
#7768=EDGE_CURVE('',#6129,#6131,#384,.T.);
#7769=EDGE_CURVE('',#6133,#6134,#4518,.T.);
#7770=EDGE_CURVE('',#6134,#6132,#385,.T.);
#7771=EDGE_CURVE('',#6131,#6133,#386,.T.);
#7772=EDGE_CURVE('',#6135,#6136,#4519,.T.);
#7773=EDGE_CURVE('',#6136,#6134,#387,.T.);
#7774=EDGE_CURVE('',#6133,#6135,#388,.T.);
#7775=EDGE_CURVE('',#6137,#6138,#4520,.T.);
#7776=EDGE_CURVE('',#6138,#6136,#389,.T.);
#7777=EDGE_CURVE('',#6135,#6137,#390,.T.);
#7778=EDGE_CURVE('',#6139,#6140,#4521,.T.);
#7779=EDGE_CURVE('',#6140,#6138,#391,.T.);
#7780=EDGE_CURVE('',#6137,#6139,#392,.T.);
#7781=EDGE_CURVE('',#6141,#6142,#4522,.T.);
#7782=EDGE_CURVE('',#6142,#6140,#393,.T.);
#7783=EDGE_CURVE('',#6139,#6141,#394,.T.);
#7784=EDGE_CURVE('',#6143,#6144,#4523,.T.);
#7785=EDGE_CURVE('',#6144,#6142,#395,.T.);
#7786=EDGE_CURVE('',#6141,#6143,#396,.T.);
#7787=EDGE_CURVE('',#6145,#6146,#4524,.T.);
#7788=EDGE_CURVE('',#6146,#6144,#397,.T.);
#7789=EDGE_CURVE('',#6143,#6145,#398,.T.);
#7790=EDGE_CURVE('',#6147,#6148,#4525,.T.);
#7791=EDGE_CURVE('',#6148,#6146,#399,.T.);
#7792=EDGE_CURVE('',#6145,#6147,#400,.T.);
#7793=EDGE_CURVE('',#6149,#6150,#4526,.T.);
#7794=EDGE_CURVE('',#6149,#6151,#401,.T.);
#7795=EDGE_CURVE('',#6152,#6151,#2424,.F.);
#7796=EDGE_CURVE('',#6152,#6150,#402,.T.);
#7797=EDGE_CURVE('',#6153,#6154,#4527,.T.);
#7798=EDGE_CURVE('',#6154,#6155,#403,.T.);
#7799=EDGE_CURVE('',#6156,#6155,#2425,.T.);
#7800=EDGE_CURVE('',#6153,#6156,#404,.T.);
#7801=EDGE_CURVE('',#6157,#6158,#4528,.T.);
#7802=EDGE_CURVE('',#6158,#6154,#405,.T.);
#7803=EDGE_CURVE('',#6157,#6153,#406,.T.);
#7804=EDGE_CURVE('',#6159,#6160,#4529,.T.);
#7805=EDGE_CURVE('',#6160,#6158,#407,.T.);
#7806=EDGE_CURVE('',#6159,#6157,#408,.T.);
#7807=EDGE_CURVE('',#6161,#6162,#4530,.T.);
#7808=EDGE_CURVE('',#6162,#6160,#409,.T.);
#7809=EDGE_CURVE('',#6161,#6159,#410,.T.);
#7810=EDGE_CURVE('',#6163,#6164,#4531,.T.);
#7811=EDGE_CURVE('',#6164,#6162,#411,.T.);
#7812=EDGE_CURVE('',#6163,#6161,#412,.T.);
#7813=EDGE_CURVE('',#6165,#6166,#4532,.T.);
#7814=EDGE_CURVE('',#6166,#6164,#413,.T.);
#7815=EDGE_CURVE('',#6165,#6163,#414,.T.);
#7816=EDGE_CURVE('',#6167,#6168,#4533,.T.);
#7817=EDGE_CURVE('',#6168,#6166,#415,.T.);
#7818=EDGE_CURVE('',#6167,#6165,#416,.T.);
#7819=EDGE_CURVE('',#6169,#6170,#4534,.T.);
#7820=EDGE_CURVE('',#6170,#6168,#417,.T.);
#7821=EDGE_CURVE('',#6169,#6167,#418,.T.);
#7822=EDGE_CURVE('',#6171,#6172,#4535,.T.);
#7823=EDGE_CURVE('',#6172,#6170,#419,.T.);
#7824=EDGE_CURVE('',#6171,#6169,#420,.T.);
#7825=EDGE_CURVE('',#6173,#6174,#4536,.T.);
#7826=EDGE_CURVE('',#6174,#6172,#421,.T.);
#7827=EDGE_CURVE('',#6173,#6171,#422,.T.);
#7828=EDGE_CURVE('',#6175,#6176,#4537,.T.);
#7829=EDGE_CURVE('',#6176,#6174,#423,.T.);
#7830=EDGE_CURVE('',#6175,#6173,#424,.T.);
#7831=EDGE_CURVE('',#6177,#6178,#4538,.T.);
#7832=EDGE_CURVE('',#6178,#6176,#425,.T.);
#7833=EDGE_CURVE('',#6177,#6175,#426,.T.);
#7834=EDGE_CURVE('',#6179,#6180,#4539,.T.);
#7835=EDGE_CURVE('',#6180,#6178,#427,.T.);
#7836=EDGE_CURVE('',#6179,#6177,#428,.T.);
#7837=EDGE_CURVE('',#6181,#6182,#4540,.T.);
#7838=EDGE_CURVE('',#6182,#6180,#429,.T.);
#7839=EDGE_CURVE('',#6181,#6179,#430,.T.);
#7840=EDGE_CURVE('',#6183,#6184,#4541,.T.);
#7841=EDGE_CURVE('',#6184,#6182,#431,.T.);
#7842=EDGE_CURVE('',#6183,#6181,#432,.T.);
#7843=EDGE_CURVE('',#6185,#6186,#4542,.T.);
#7844=EDGE_CURVE('',#6186,#6184,#433,.T.);
#7845=EDGE_CURVE('',#6185,#6183,#434,.T.);
#7846=EDGE_CURVE('',#6187,#6188,#4543,.T.);
#7847=EDGE_CURVE('',#6188,#6186,#435,.T.);
#7848=EDGE_CURVE('',#6187,#6185,#436,.T.);
#7849=EDGE_CURVE('',#6189,#6190,#4544,.T.);
#7850=EDGE_CURVE('',#6190,#6188,#437,.T.);
#7851=EDGE_CURVE('',#6189,#6187,#438,.T.);
#7852=EDGE_CURVE('',#6191,#6192,#4545,.T.);
#7853=EDGE_CURVE('',#6193,#6191,#439,.T.);
#7854=EDGE_CURVE('',#6194,#6193,#2426,.T.);
#7855=EDGE_CURVE('',#6194,#6192,#440,.T.);
#7856=EDGE_CURVE('',#6195,#6196,#4546,.T.);
#7857=EDGE_CURVE('',#6196,#6197,#441,.T.);
#7858=EDGE_CURVE('',#6197,#6198,#2427,.T.);
#7859=EDGE_CURVE('',#6198,#6199,#4547,.T.);
#7860=EDGE_CURVE('',#6199,#6199,#2428,.F.);
#7861=EDGE_CURVE('',#6198,#6200,#2429,.T.);
#7862=EDGE_CURVE('',#6200,#6195,#442,.T.);
#7863=EDGE_CURVE('',#6201,#6202,#4548,.T.);
#7864=EDGE_CURVE('',#6202,#6196,#443,.T.);
#7865=EDGE_CURVE('',#6195,#6201,#444,.T.);
#7866=EDGE_CURVE('',#6203,#6204,#4549,.T.);
#7867=EDGE_CURVE('',#6204,#6202,#445,.T.);
#7868=EDGE_CURVE('',#6201,#6203,#446,.T.);
#7869=EDGE_CURVE('',#6205,#6206,#4550,.T.);
#7870=EDGE_CURVE('',#6206,#6204,#447,.T.);
#7871=EDGE_CURVE('',#6203,#6205,#448,.T.);
#7872=EDGE_CURVE('',#6207,#6208,#4551,.T.);
#7873=EDGE_CURVE('',#6208,#6206,#449,.T.);
#7874=EDGE_CURVE('',#6205,#6207,#450,.T.);
#7875=EDGE_CURVE('',#6209,#6210,#4552,.T.);
#7876=EDGE_CURVE('',#6210,#6208,#451,.T.);
#7877=EDGE_CURVE('',#6207,#6209,#452,.T.);
#7878=EDGE_CURVE('',#6211,#6212,#4553,.T.);
#7879=EDGE_CURVE('',#6212,#6210,#453,.T.);
#7880=EDGE_CURVE('',#6209,#6211,#454,.T.);
#7881=EDGE_CURVE('',#6213,#6214,#4554,.T.);
#7882=EDGE_CURVE('',#6214,#6212,#455,.T.);
#7883=EDGE_CURVE('',#6211,#6213,#456,.T.);
#7884=EDGE_CURVE('',#6215,#6216,#4555,.T.);
#7885=EDGE_CURVE('',#6216,#6214,#457,.T.);
#7886=EDGE_CURVE('',#6213,#6215,#458,.T.);
#7887=EDGE_CURVE('',#6217,#6218,#4556,.T.);
#7888=EDGE_CURVE('',#6218,#6216,#459,.T.);
#7889=EDGE_CURVE('',#6215,#6217,#460,.T.);
#7890=EDGE_CURVE('',#6219,#6220,#4557,.T.);
#7891=EDGE_CURVE('',#6220,#6218,#461,.T.);
#7892=EDGE_CURVE('',#6217,#6219,#462,.T.);
#7893=EDGE_CURVE('',#6221,#6222,#4558,.T.);
#7894=EDGE_CURVE('',#6222,#6220,#463,.T.);
#7895=EDGE_CURVE('',#6219,#6221,#464,.T.);
#7896=EDGE_CURVE('',#6223,#6224,#4559,.T.);
#7897=EDGE_CURVE('',#6224,#6222,#465,.T.);
#7898=EDGE_CURVE('',#6221,#6223,#466,.T.);
#7899=EDGE_CURVE('',#6225,#6226,#4560,.T.);
#7900=EDGE_CURVE('',#6226,#6224,#467,.T.);
#7901=EDGE_CURVE('',#6223,#6225,#468,.T.);
#7902=EDGE_CURVE('',#6227,#6228,#4561,.T.);
#7903=EDGE_CURVE('',#6228,#6226,#469,.T.);
#7904=EDGE_CURVE('',#6225,#6227,#470,.T.);
#7905=EDGE_CURVE('',#6229,#6230,#4562,.T.);
#7906=EDGE_CURVE('',#6230,#6228,#471,.T.);
#7907=EDGE_CURVE('',#6227,#6229,#472,.T.);
#7908=EDGE_CURVE('',#6231,#6232,#4563,.T.);
#7909=EDGE_CURVE('',#6232,#6230,#473,.T.);
#7910=EDGE_CURVE('',#6229,#6231,#474,.T.);
#7911=EDGE_CURVE('',#6233,#6234,#4564,.T.);
#7912=EDGE_CURVE('',#6233,#6235,#475,.T.);
#7913=EDGE_CURVE('',#6236,#6235,#2430,.F.);
#7914=EDGE_CURVE('',#6236,#6234,#476,.T.);
#7915=EDGE_CURVE('',#6237,#6238,#4565,.T.);
#7916=EDGE_CURVE('',#6238,#6239,#477,.T.);
#7917=EDGE_CURVE('',#6240,#6239,#2431,.T.);
#7918=EDGE_CURVE('',#6237,#6240,#478,.T.);
#7919=EDGE_CURVE('',#6241,#6242,#4566,.T.);
#7920=EDGE_CURVE('',#6242,#6238,#479,.T.);
#7921=EDGE_CURVE('',#6241,#6237,#480,.T.);
#7922=EDGE_CURVE('',#6243,#6244,#4567,.T.);
#7923=EDGE_CURVE('',#6244,#6242,#481,.T.);
#7924=EDGE_CURVE('',#6243,#6241,#482,.T.);
#7925=EDGE_CURVE('',#6245,#6246,#4568,.T.);
#7926=EDGE_CURVE('',#6246,#6244,#483,.T.);
#7927=EDGE_CURVE('',#6245,#6243,#484,.T.);
#7928=EDGE_CURVE('',#6247,#6248,#4569,.T.);
#7929=EDGE_CURVE('',#6248,#6246,#485,.T.);
#7930=EDGE_CURVE('',#6247,#6245,#486,.T.);
#7931=EDGE_CURVE('',#6249,#6250,#4570,.T.);
#7932=EDGE_CURVE('',#6250,#6248,#487,.T.);
#7933=EDGE_CURVE('',#6249,#6247,#488,.T.);
#7934=EDGE_CURVE('',#6251,#6252,#4571,.T.);
#7935=EDGE_CURVE('',#6252,#6250,#489,.T.);
#7936=EDGE_CURVE('',#6251,#6249,#490,.T.);
#7937=EDGE_CURVE('',#6253,#6254,#4572,.T.);
#7938=EDGE_CURVE('',#6254,#6252,#491,.T.);
#7939=EDGE_CURVE('',#6253,#6251,#492,.T.);
#7940=EDGE_CURVE('',#6255,#6256,#4573,.T.);
#7941=EDGE_CURVE('',#6256,#6254,#493,.T.);
#7942=EDGE_CURVE('',#6255,#6253,#494,.T.);
#7943=EDGE_CURVE('',#6257,#6258,#4574,.T.);
#7944=EDGE_CURVE('',#6258,#6256,#495,.T.);
#7945=EDGE_CURVE('',#6257,#6255,#496,.T.);
#7946=EDGE_CURVE('',#6259,#6260,#4575,.T.);
#7947=EDGE_CURVE('',#6260,#6258,#497,.T.);
#7948=EDGE_CURVE('',#6259,#6257,#498,.T.);
#7949=EDGE_CURVE('',#6261,#6262,#4576,.T.);
#7950=EDGE_CURVE('',#6262,#6260,#499,.T.);
#7951=EDGE_CURVE('',#6261,#6259,#500,.T.);
#7952=EDGE_CURVE('',#6263,#6264,#4577,.T.);
#7953=EDGE_CURVE('',#6264,#6262,#501,.T.);
#7954=EDGE_CURVE('',#6263,#6261,#502,.T.);
#7955=EDGE_CURVE('',#6265,#6266,#4578,.T.);
#7956=EDGE_CURVE('',#6266,#6264,#503,.T.);
#7957=EDGE_CURVE('',#6265,#6263,#504,.T.);
#7958=EDGE_CURVE('',#6267,#6268,#4579,.T.);
#7959=EDGE_CURVE('',#6268,#6266,#505,.T.);
#7960=EDGE_CURVE('',#6267,#6265,#506,.T.);
#7961=EDGE_CURVE('',#6269,#6270,#4580,.T.);
#7962=EDGE_CURVE('',#6270,#6268,#507,.T.);
#7963=EDGE_CURVE('',#6269,#6267,#508,.T.);
#7964=EDGE_CURVE('',#6271,#6272,#4581,.T.);
#7965=EDGE_CURVE('',#6272,#6270,#509,.T.);
#7966=EDGE_CURVE('',#6271,#6269,#510,.T.);
#7967=EDGE_CURVE('',#6273,#6274,#4582,.T.);
#7968=EDGE_CURVE('',#6274,#6272,#511,.T.);
#7969=EDGE_CURVE('',#6273,#6271,#512,.T.);
#7970=EDGE_CURVE('',#6275,#6276,#4583,.T.);
#7971=EDGE_CURVE('',#6277,#6275,#513,.T.);
#7972=EDGE_CURVE('',#6278,#6277,#2432,.T.);
#7973=EDGE_CURVE('',#6278,#6276,#514,.T.);
#7974=EDGE_CURVE('',#6279,#6280,#4584,.T.);
#7975=EDGE_CURVE('',#6280,#6281,#515,.T.);
#7976=EDGE_CURVE('',#6281,#6282,#2433,.T.);
#7977=EDGE_CURVE('',#6282,#6283,#4585,.T.);
#7978=EDGE_CURVE('',#6283,#6283,#2434,.F.);
#7979=EDGE_CURVE('',#6282,#6284,#2435,.T.);
#7980=EDGE_CURVE('',#6284,#6279,#516,.T.);
#7981=EDGE_CURVE('',#6285,#6286,#4586,.T.);
#7982=EDGE_CURVE('',#6286,#6280,#517,.T.);
#7983=EDGE_CURVE('',#6279,#6285,#518,.T.);
#7984=EDGE_CURVE('',#6287,#6288,#4587,.T.);
#7985=EDGE_CURVE('',#6288,#6286,#519,.T.);
#7986=EDGE_CURVE('',#6285,#6287,#520,.T.);
#7987=EDGE_CURVE('',#6289,#6290,#4588,.T.);
#7988=EDGE_CURVE('',#6290,#6288,#521,.T.);
#7989=EDGE_CURVE('',#6287,#6289,#522,.T.);
#7990=EDGE_CURVE('',#6291,#6292,#4589,.T.);
#7991=EDGE_CURVE('',#6292,#6290,#523,.T.);
#7992=EDGE_CURVE('',#6289,#6291,#524,.T.);
#7993=EDGE_CURVE('',#6293,#6294,#4590,.T.);
#7994=EDGE_CURVE('',#6294,#6292,#525,.T.);
#7995=EDGE_CURVE('',#6291,#6293,#526,.T.);
#7996=EDGE_CURVE('',#6295,#6296,#4591,.T.);
#7997=EDGE_CURVE('',#6296,#6294,#527,.T.);
#7998=EDGE_CURVE('',#6293,#6295,#528,.T.);
#7999=EDGE_CURVE('',#6297,#6298,#4592,.T.);
#8000=EDGE_CURVE('',#6298,#6296,#529,.T.);
#8001=EDGE_CURVE('',#6295,#6297,#530,.T.);
#8002=EDGE_CURVE('',#6299,#6300,#4593,.T.);
#8003=EDGE_CURVE('',#6300,#6298,#531,.T.);
#8004=EDGE_CURVE('',#6297,#6299,#532,.T.);
#8005=EDGE_CURVE('',#6301,#6302,#4594,.T.);
#8006=EDGE_CURVE('',#6302,#6300,#533,.T.);
#8007=EDGE_CURVE('',#6299,#6301,#534,.T.);
#8008=EDGE_CURVE('',#6303,#6304,#4595,.T.);
#8009=EDGE_CURVE('',#6304,#6302,#535,.T.);
#8010=EDGE_CURVE('',#6301,#6303,#536,.T.);
#8011=EDGE_CURVE('',#6305,#6306,#4596,.T.);
#8012=EDGE_CURVE('',#6306,#6304,#537,.T.);
#8013=EDGE_CURVE('',#6303,#6305,#538,.T.);
#8014=EDGE_CURVE('',#6307,#6308,#4597,.T.);
#8015=EDGE_CURVE('',#6308,#6306,#539,.T.);
#8016=EDGE_CURVE('',#6305,#6307,#540,.T.);
#8017=EDGE_CURVE('',#6309,#6310,#4598,.T.);
#8018=EDGE_CURVE('',#6310,#6308,#541,.T.);
#8019=EDGE_CURVE('',#6307,#6309,#542,.T.);
#8020=EDGE_CURVE('',#6311,#6312,#4599,.T.);
#8021=EDGE_CURVE('',#6312,#6310,#543,.T.);
#8022=EDGE_CURVE('',#6309,#6311,#544,.T.);
#8023=EDGE_CURVE('',#6313,#6314,#4600,.T.);
#8024=EDGE_CURVE('',#6314,#6312,#545,.T.);
#8025=EDGE_CURVE('',#6311,#6313,#546,.T.);
#8026=EDGE_CURVE('',#6315,#6316,#4601,.T.);
#8027=EDGE_CURVE('',#6316,#6314,#547,.T.);
#8028=EDGE_CURVE('',#6313,#6315,#548,.T.);
#8029=EDGE_CURVE('',#6317,#6318,#4602,.T.);
#8030=EDGE_CURVE('',#6317,#6319,#549,.T.);
#8031=EDGE_CURVE('',#6320,#6319,#2436,.F.);
#8032=EDGE_CURVE('',#6320,#6318,#550,.T.);
#8033=EDGE_CURVE('',#6321,#6322,#4603,.T.);
#8034=EDGE_CURVE('',#6322,#6323,#551,.T.);
#8035=EDGE_CURVE('',#6324,#6323,#2437,.T.);
#8036=EDGE_CURVE('',#6321,#6324,#552,.T.);
#8037=EDGE_CURVE('',#6325,#6326,#4604,.T.);
#8038=EDGE_CURVE('',#6326,#6322,#553,.T.);
#8039=EDGE_CURVE('',#6325,#6321,#554,.T.);
#8040=EDGE_CURVE('',#6327,#6328,#4605,.T.);
#8041=EDGE_CURVE('',#6328,#6326,#555,.T.);
#8042=EDGE_CURVE('',#6327,#6325,#556,.T.);
#8043=EDGE_CURVE('',#6329,#6330,#4606,.T.);
#8044=EDGE_CURVE('',#6330,#6328,#557,.T.);
#8045=EDGE_CURVE('',#6329,#6327,#558,.T.);
#8046=EDGE_CURVE('',#6331,#6332,#4607,.T.);
#8047=EDGE_CURVE('',#6332,#6330,#559,.T.);
#8048=EDGE_CURVE('',#6331,#6329,#560,.T.);
#8049=EDGE_CURVE('',#6333,#6334,#4608,.T.);
#8050=EDGE_CURVE('',#6334,#6332,#561,.T.);
#8051=EDGE_CURVE('',#6333,#6331,#562,.T.);
#8052=EDGE_CURVE('',#6335,#6336,#4609,.T.);
#8053=EDGE_CURVE('',#6336,#6334,#563,.T.);
#8054=EDGE_CURVE('',#6335,#6333,#564,.T.);
#8055=EDGE_CURVE('',#6337,#6338,#4610,.T.);
#8056=EDGE_CURVE('',#6338,#6336,#565,.T.);
#8057=EDGE_CURVE('',#6337,#6335,#566,.T.);
#8058=EDGE_CURVE('',#6339,#6340,#4611,.T.);
#8059=EDGE_CURVE('',#6340,#6338,#567,.T.);
#8060=EDGE_CURVE('',#6339,#6337,#568,.T.);
#8061=EDGE_CURVE('',#6341,#6342,#4612,.T.);
#8062=EDGE_CURVE('',#6342,#6340,#569,.T.);
#8063=EDGE_CURVE('',#6341,#6339,#570,.T.);
#8064=EDGE_CURVE('',#6343,#6344,#4613,.T.);
#8065=EDGE_CURVE('',#6344,#6342,#571,.T.);
#8066=EDGE_CURVE('',#6343,#6341,#572,.T.);
#8067=EDGE_CURVE('',#6345,#6346,#4614,.T.);
#8068=EDGE_CURVE('',#6346,#6344,#573,.T.);
#8069=EDGE_CURVE('',#6345,#6343,#574,.T.);
#8070=EDGE_CURVE('',#6347,#6348,#4615,.T.);
#8071=EDGE_CURVE('',#6348,#6346,#575,.T.);
#8072=EDGE_CURVE('',#6347,#6345,#576,.T.);
#8073=EDGE_CURVE('',#6349,#6350,#4616,.T.);
#8074=EDGE_CURVE('',#6350,#6348,#577,.T.);
#8075=EDGE_CURVE('',#6349,#6347,#578,.T.);
#8076=EDGE_CURVE('',#6351,#6352,#4617,.T.);
#8077=EDGE_CURVE('',#6352,#6350,#579,.T.);
#8078=EDGE_CURVE('',#6351,#6349,#580,.T.);
#8079=EDGE_CURVE('',#6353,#6354,#4618,.T.);
#8080=EDGE_CURVE('',#6354,#6352,#581,.T.);
#8081=EDGE_CURVE('',#6353,#6351,#582,.T.);
#8082=EDGE_CURVE('',#6355,#6356,#4619,.T.);
#8083=EDGE_CURVE('',#6356,#6354,#583,.T.);
#8084=EDGE_CURVE('',#6355,#6353,#584,.T.);
#8085=EDGE_CURVE('',#6357,#6358,#4620,.T.);
#8086=EDGE_CURVE('',#6358,#6356,#585,.T.);
#8087=EDGE_CURVE('',#6357,#6355,#586,.T.);
#8088=EDGE_CURVE('',#6359,#6360,#4621,.T.);
#8089=EDGE_CURVE('',#6361,#6359,#587,.T.);
#8090=EDGE_CURVE('',#6362,#6361,#2438,.T.);
#8091=EDGE_CURVE('',#6362,#6360,#588,.T.);
#8092=EDGE_CURVE('',#6363,#6364,#4622,.T.);
#8093=EDGE_CURVE('',#6364,#6365,#589,.T.);
#8094=EDGE_CURVE('',#6365,#6366,#2439,.T.);
#8095=EDGE_CURVE('',#6366,#6367,#4623,.T.);
#8096=EDGE_CURVE('',#6367,#6367,#2440,.F.);
#8097=EDGE_CURVE('',#6366,#6368,#2441,.T.);
#8098=EDGE_CURVE('',#6368,#6363,#590,.T.);
#8099=EDGE_CURVE('',#6369,#6370,#4624,.T.);
#8100=EDGE_CURVE('',#6370,#6364,#591,.T.);
#8101=EDGE_CURVE('',#6363,#6369,#592,.T.);
#8102=EDGE_CURVE('',#6371,#6372,#4625,.T.);
#8103=EDGE_CURVE('',#6372,#6370,#593,.T.);
#8104=EDGE_CURVE('',#6369,#6371,#594,.T.);
#8105=EDGE_CURVE('',#6373,#6374,#4626,.T.);
#8106=EDGE_CURVE('',#6374,#6372,#595,.T.);
#8107=EDGE_CURVE('',#6371,#6373,#596,.T.);
#8108=EDGE_CURVE('',#6375,#6376,#4627,.T.);
#8109=EDGE_CURVE('',#6376,#6374,#597,.T.);
#8110=EDGE_CURVE('',#6373,#6375,#598,.T.);
#8111=EDGE_CURVE('',#6377,#6378,#4628,.T.);
#8112=EDGE_CURVE('',#6378,#6376,#599,.T.);
#8113=EDGE_CURVE('',#6375,#6377,#600,.T.);
#8114=EDGE_CURVE('',#6379,#6380,#4629,.T.);
#8115=EDGE_CURVE('',#6380,#6378,#601,.T.);
#8116=EDGE_CURVE('',#6377,#6379,#602,.T.);
#8117=EDGE_CURVE('',#6381,#6382,#4630,.T.);
#8118=EDGE_CURVE('',#6382,#6380,#603,.T.);
#8119=EDGE_CURVE('',#6379,#6381,#604,.T.);
#8120=EDGE_CURVE('',#6383,#6384,#4631,.T.);
#8121=EDGE_CURVE('',#6384,#6382,#605,.T.);
#8122=EDGE_CURVE('',#6381,#6383,#606,.T.);
#8123=EDGE_CURVE('',#6385,#6386,#4632,.T.);
#8124=EDGE_CURVE('',#6386,#6384,#607,.T.);
#8125=EDGE_CURVE('',#6383,#6385,#608,.T.);
#8126=EDGE_CURVE('',#6387,#6388,#4633,.T.);
#8127=EDGE_CURVE('',#6388,#6386,#609,.T.);
#8128=EDGE_CURVE('',#6385,#6387,#610,.T.);
#8129=EDGE_CURVE('',#6389,#6390,#4634,.T.);
#8130=EDGE_CURVE('',#6390,#6388,#611,.T.);
#8131=EDGE_CURVE('',#6387,#6389,#612,.T.);
#8132=EDGE_CURVE('',#6391,#6392,#4635,.T.);
#8133=EDGE_CURVE('',#6392,#6390,#613,.T.);
#8134=EDGE_CURVE('',#6389,#6391,#614,.T.);
#8135=EDGE_CURVE('',#6393,#6394,#4636,.T.);
#8136=EDGE_CURVE('',#6394,#6392,#615,.T.);
#8137=EDGE_CURVE('',#6391,#6393,#616,.T.);
#8138=EDGE_CURVE('',#6395,#6396,#4637,.T.);
#8139=EDGE_CURVE('',#6396,#6394,#617,.T.);
#8140=EDGE_CURVE('',#6393,#6395,#618,.T.);
#8141=EDGE_CURVE('',#6397,#6398,#4638,.T.);
#8142=EDGE_CURVE('',#6398,#6396,#619,.T.);
#8143=EDGE_CURVE('',#6395,#6397,#620,.T.);
#8144=EDGE_CURVE('',#6399,#6400,#4639,.T.);
#8145=EDGE_CURVE('',#6400,#6398,#621,.T.);
#8146=EDGE_CURVE('',#6397,#6399,#622,.T.);
#8147=EDGE_CURVE('',#6401,#6402,#4640,.T.);
#8148=EDGE_CURVE('',#6401,#6403,#623,.T.);
#8149=EDGE_CURVE('',#6404,#6403,#2442,.T.);
#8150=EDGE_CURVE('',#6404,#6402,#624,.T.);
#8151=EDGE_CURVE('',#6405,#6406,#4641,.T.);
#8152=EDGE_CURVE('',#6406,#6407,#625,.T.);
#8153=EDGE_CURVE('',#6408,#6407,#2443,.T.);
#8154=EDGE_CURVE('',#6405,#6408,#626,.T.);
#8155=EDGE_CURVE('',#6409,#6410,#4642,.T.);
#8156=EDGE_CURVE('',#6410,#6406,#627,.T.);
#8157=EDGE_CURVE('',#6409,#6405,#628,.T.);
#8158=EDGE_CURVE('',#6411,#6412,#4643,.T.);
#8159=EDGE_CURVE('',#6412,#6410,#629,.T.);
#8160=EDGE_CURVE('',#6411,#6409,#630,.T.);
#8161=EDGE_CURVE('',#6413,#6414,#4644,.T.);
#8162=EDGE_CURVE('',#6414,#6412,#631,.T.);
#8163=EDGE_CURVE('',#6413,#6411,#632,.T.);
#8164=EDGE_CURVE('',#6415,#6416,#4645,.T.);
#8165=EDGE_CURVE('',#6416,#6414,#633,.T.);
#8166=EDGE_CURVE('',#6415,#6413,#634,.T.);
#8167=EDGE_CURVE('',#6417,#6418,#4646,.T.);
#8168=EDGE_CURVE('',#6418,#6416,#635,.T.);
#8169=EDGE_CURVE('',#6417,#6415,#636,.T.);
#8170=EDGE_CURVE('',#6419,#6420,#4647,.T.);
#8171=EDGE_CURVE('',#6420,#6418,#637,.T.);
#8172=EDGE_CURVE('',#6419,#6417,#638,.T.);
#8173=EDGE_CURVE('',#6421,#6422,#4648,.T.);
#8174=EDGE_CURVE('',#6422,#6420,#639,.T.);
#8175=EDGE_CURVE('',#6421,#6419,#640,.T.);
#8176=EDGE_CURVE('',#6423,#6424,#4649,.T.);
#8177=EDGE_CURVE('',#6424,#6422,#641,.T.);
#8178=EDGE_CURVE('',#6423,#6421,#642,.T.);
#8179=EDGE_CURVE('',#6425,#6426,#4650,.T.);
#8180=EDGE_CURVE('',#6426,#6424,#643,.T.);
#8181=EDGE_CURVE('',#6425,#6423,#644,.T.);
#8182=EDGE_CURVE('',#6427,#6428,#4651,.T.);
#8183=EDGE_CURVE('',#6428,#6426,#645,.T.);
#8184=EDGE_CURVE('',#6427,#6425,#646,.T.);
#8185=EDGE_CURVE('',#6429,#6430,#4652,.T.);
#8186=EDGE_CURVE('',#6430,#6428,#647,.T.);
#8187=EDGE_CURVE('',#6429,#6427,#648,.T.);
#8188=EDGE_CURVE('',#6431,#6432,#4653,.T.);
#8189=EDGE_CURVE('',#6432,#6430,#649,.T.);
#8190=EDGE_CURVE('',#6431,#6429,#650,.T.);
#8191=EDGE_CURVE('',#6433,#6434,#4654,.T.);
#8192=EDGE_CURVE('',#6434,#6432,#651,.T.);
#8193=EDGE_CURVE('',#6433,#6431,#652,.T.);
#8194=EDGE_CURVE('',#6435,#6436,#4655,.T.);
#8195=EDGE_CURVE('',#6436,#6434,#653,.T.);
#8196=EDGE_CURVE('',#6435,#6433,#654,.T.);
#8197=EDGE_CURVE('',#6437,#6438,#4656,.T.);
#8198=EDGE_CURVE('',#6438,#6436,#655,.T.);
#8199=EDGE_CURVE('',#6437,#6435,#656,.T.);
#8200=EDGE_CURVE('',#6439,#6440,#4657,.T.);
#8201=EDGE_CURVE('',#6440,#6438,#657,.T.);
#8202=EDGE_CURVE('',#6439,#6437,#658,.T.);
#8203=EDGE_CURVE('',#6441,#6442,#4658,.T.);
#8204=EDGE_CURVE('',#6442,#6440,#659,.T.);
#8205=EDGE_CURVE('',#6441,#6439,#660,.T.);
#8206=EDGE_CURVE('',#6443,#6444,#4659,.T.);
#8207=EDGE_CURVE('',#6445,#6443,#661,.T.);
#8208=EDGE_CURVE('',#6446,#6445,#2444,.T.);
#8209=EDGE_CURVE('',#6446,#6444,#662,.T.);
#8210=EDGE_CURVE('',#6447,#6448,#4660,.T.);
#8211=EDGE_CURVE('',#6448,#6449,#663,.T.);
#8212=EDGE_CURVE('',#6449,#6450,#2445,.T.);
#8213=EDGE_CURVE('',#6450,#6451,#4661,.T.);
#8214=EDGE_CURVE('',#6451,#6451,#2446,.F.);
#8215=EDGE_CURVE('',#6450,#6452,#2447,.T.);
#8216=EDGE_CURVE('',#6452,#6447,#664,.T.);
#8217=EDGE_CURVE('',#6453,#6454,#4662,.T.);
#8218=EDGE_CURVE('',#6454,#6448,#665,.T.);
#8219=EDGE_CURVE('',#6447,#6453,#666,.T.);
#8220=EDGE_CURVE('',#6455,#6456,#4663,.T.);
#8221=EDGE_CURVE('',#6456,#6454,#667,.T.);
#8222=EDGE_CURVE('',#6453,#6455,#668,.T.);
#8223=EDGE_CURVE('',#6457,#6458,#4664,.T.);
#8224=EDGE_CURVE('',#6458,#6456,#669,.T.);
#8225=EDGE_CURVE('',#6455,#6457,#670,.T.);
#8226=EDGE_CURVE('',#6459,#6460,#4665,.T.);
#8227=EDGE_CURVE('',#6460,#6458,#671,.T.);
#8228=EDGE_CURVE('',#6457,#6459,#672,.T.);
#8229=EDGE_CURVE('',#6461,#6462,#4666,.T.);
#8230=EDGE_CURVE('',#6462,#6460,#673,.T.);
#8231=EDGE_CURVE('',#6459,#6461,#674,.T.);
#8232=EDGE_CURVE('',#6463,#6464,#4667,.T.);
#8233=EDGE_CURVE('',#6464,#6462,#675,.T.);
#8234=EDGE_CURVE('',#6461,#6463,#676,.T.);
#8235=EDGE_CURVE('',#6465,#6466,#4668,.T.);
#8236=EDGE_CURVE('',#6466,#6464,#677,.T.);
#8237=EDGE_CURVE('',#6463,#6465,#678,.T.);
#8238=EDGE_CURVE('',#6467,#6468,#4669,.T.);
#8239=EDGE_CURVE('',#6468,#6466,#679,.T.);
#8240=EDGE_CURVE('',#6465,#6467,#680,.T.);
#8241=EDGE_CURVE('',#6469,#6470,#4670,.T.);
#8242=EDGE_CURVE('',#6470,#6468,#681,.T.);
#8243=EDGE_CURVE('',#6467,#6469,#682,.T.);
#8244=EDGE_CURVE('',#6471,#6472,#4671,.T.);
#8245=EDGE_CURVE('',#6472,#6470,#683,.T.);
#8246=EDGE_CURVE('',#6469,#6471,#684,.T.);
#8247=EDGE_CURVE('',#6473,#6474,#4672,.T.);
#8248=EDGE_CURVE('',#6474,#6472,#685,.T.);
#8249=EDGE_CURVE('',#6471,#6473,#686,.T.);
#8250=EDGE_CURVE('',#6475,#6476,#4673,.T.);
#8251=EDGE_CURVE('',#6476,#6474,#687,.T.);
#8252=EDGE_CURVE('',#6473,#6475,#688,.T.);
#8253=EDGE_CURVE('',#6477,#6478,#4674,.T.);
#8254=EDGE_CURVE('',#6478,#6476,#689,.T.);
#8255=EDGE_CURVE('',#6475,#6477,#690,.T.);
#8256=EDGE_CURVE('',#6479,#6480,#4675,.T.);
#8257=EDGE_CURVE('',#6480,#6478,#691,.T.);
#8258=EDGE_CURVE('',#6477,#6479,#692,.T.);
#8259=EDGE_CURVE('',#6481,#6482,#4676,.T.);
#8260=EDGE_CURVE('',#6482,#6480,#693,.T.);
#8261=EDGE_CURVE('',#6479,#6481,#694,.T.);
#8262=EDGE_CURVE('',#6483,#6484,#4677,.T.);
#8263=EDGE_CURVE('',#6484,#6482,#695,.T.);
#8264=EDGE_CURVE('',#6481,#6483,#696,.T.);
#8265=EDGE_CURVE('',#6485,#6486,#4678,.T.);
#8266=EDGE_CURVE('',#6485,#6487,#697,.T.);
#8267=EDGE_CURVE('',#6488,#6487,#2448,.T.);
#8268=EDGE_CURVE('',#6488,#6486,#698,.T.);
#8269=EDGE_CURVE('',#6489,#6490,#4679,.T.);
#8270=EDGE_CURVE('',#6490,#6491,#699,.T.);
#8271=EDGE_CURVE('',#6492,#6491,#2449,.T.);
#8272=EDGE_CURVE('',#6489,#6492,#700,.T.);
#8273=EDGE_CURVE('',#6493,#6494,#4680,.T.);
#8274=EDGE_CURVE('',#6494,#6490,#701,.T.);
#8275=EDGE_CURVE('',#6493,#6489,#702,.T.);
#8276=EDGE_CURVE('',#6495,#6496,#4681,.T.);
#8277=EDGE_CURVE('',#6496,#6494,#703,.T.);
#8278=EDGE_CURVE('',#6495,#6493,#704,.T.);
#8279=EDGE_CURVE('',#6497,#6498,#4682,.T.);
#8280=EDGE_CURVE('',#6498,#6496,#705,.T.);
#8281=EDGE_CURVE('',#6497,#6495,#706,.T.);
#8282=EDGE_CURVE('',#6499,#6500,#4683,.T.);
#8283=EDGE_CURVE('',#6500,#6498,#707,.T.);
#8284=EDGE_CURVE('',#6499,#6497,#708,.T.);
#8285=EDGE_CURVE('',#6501,#6502,#4684,.T.);
#8286=EDGE_CURVE('',#6502,#6500,#709,.T.);
#8287=EDGE_CURVE('',#6501,#6499,#710,.T.);
#8288=EDGE_CURVE('',#6503,#6504,#4685,.T.);
#8289=EDGE_CURVE('',#6504,#6502,#711,.T.);
#8290=EDGE_CURVE('',#6503,#6501,#712,.T.);
#8291=EDGE_CURVE('',#6505,#6506,#4686,.T.);
#8292=EDGE_CURVE('',#6506,#6504,#713,.T.);
#8293=EDGE_CURVE('',#6505,#6503,#714,.T.);
#8294=EDGE_CURVE('',#6507,#6508,#4687,.T.);
#8295=EDGE_CURVE('',#6508,#6506,#715,.T.);
#8296=EDGE_CURVE('',#6507,#6505,#716,.T.);
#8297=EDGE_CURVE('',#6509,#6510,#4688,.T.);
#8298=EDGE_CURVE('',#6510,#6508,#717,.T.);
#8299=EDGE_CURVE('',#6509,#6507,#718,.T.);
#8300=EDGE_CURVE('',#6511,#6512,#4689,.T.);
#8301=EDGE_CURVE('',#6512,#6510,#719,.T.);
#8302=EDGE_CURVE('',#6511,#6509,#720,.T.);
#8303=EDGE_CURVE('',#6513,#6514,#4690,.T.);
#8304=EDGE_CURVE('',#6514,#6512,#721,.T.);
#8305=EDGE_CURVE('',#6513,#6511,#722,.T.);
#8306=EDGE_CURVE('',#6515,#6516,#4691,.T.);
#8307=EDGE_CURVE('',#6516,#6514,#723,.T.);
#8308=EDGE_CURVE('',#6515,#6513,#724,.T.);
#8309=EDGE_CURVE('',#6517,#6518,#4692,.T.);
#8310=EDGE_CURVE('',#6518,#6516,#725,.T.);
#8311=EDGE_CURVE('',#6517,#6515,#726,.T.);
#8312=EDGE_CURVE('',#6519,#6520,#4693,.T.);
#8313=EDGE_CURVE('',#6520,#6518,#727,.T.);
#8314=EDGE_CURVE('',#6519,#6517,#728,.T.);
#8315=EDGE_CURVE('',#6521,#6522,#4694,.T.);
#8316=EDGE_CURVE('',#6522,#6520,#729,.T.);
#8317=EDGE_CURVE('',#6521,#6519,#730,.T.);
#8318=EDGE_CURVE('',#6523,#6524,#4695,.T.);
#8319=EDGE_CURVE('',#6524,#6522,#731,.T.);
#8320=EDGE_CURVE('',#6523,#6521,#732,.T.);
#8321=EDGE_CURVE('',#6525,#6526,#4696,.T.);
#8322=EDGE_CURVE('',#6526,#6524,#733,.T.);
#8323=EDGE_CURVE('',#6525,#6523,#734,.T.);
#8324=EDGE_CURVE('',#6527,#6528,#4697,.T.);
#8325=EDGE_CURVE('',#6529,#6527,#735,.T.);
#8326=EDGE_CURVE('',#6530,#6529,#2450,.T.);
#8327=EDGE_CURVE('',#6530,#6528,#736,.T.);
#8328=EDGE_CURVE('',#6531,#6532,#4698,.T.);
#8329=EDGE_CURVE('',#6532,#6533,#737,.T.);
#8330=EDGE_CURVE('',#6533,#6534,#2451,.T.);
#8331=EDGE_CURVE('',#6534,#6535,#4699,.T.);
#8332=EDGE_CURVE('',#6535,#6535,#2452,.F.);
#8333=EDGE_CURVE('',#6534,#6536,#2453,.T.);
#8334=EDGE_CURVE('',#6536,#6531,#738,.T.);
#8335=EDGE_CURVE('',#6537,#6538,#4700,.T.);
#8336=EDGE_CURVE('',#6538,#6532,#739,.T.);
#8337=EDGE_CURVE('',#6531,#6537,#740,.T.);
#8338=EDGE_CURVE('',#6539,#6540,#4701,.T.);
#8339=EDGE_CURVE('',#6540,#6538,#741,.T.);
#8340=EDGE_CURVE('',#6537,#6539,#742,.T.);
#8341=EDGE_CURVE('',#6541,#6542,#4702,.T.);
#8342=EDGE_CURVE('',#6542,#6540,#743,.T.);
#8343=EDGE_CURVE('',#6539,#6541,#744,.T.);
#8344=EDGE_CURVE('',#6543,#6544,#4703,.T.);
#8345=EDGE_CURVE('',#6544,#6542,#745,.T.);
#8346=EDGE_CURVE('',#6541,#6543,#746,.T.);
#8347=EDGE_CURVE('',#6545,#6546,#4704,.T.);
#8348=EDGE_CURVE('',#6546,#6544,#747,.T.);
#8349=EDGE_CURVE('',#6543,#6545,#748,.T.);
#8350=EDGE_CURVE('',#6547,#6548,#4705,.T.);
#8351=EDGE_CURVE('',#6548,#6546,#749,.T.);
#8352=EDGE_CURVE('',#6545,#6547,#750,.T.);
#8353=EDGE_CURVE('',#6549,#6550,#4706,.T.);
#8354=EDGE_CURVE('',#6550,#6548,#751,.T.);
#8355=EDGE_CURVE('',#6547,#6549,#752,.T.);
#8356=EDGE_CURVE('',#6551,#6552,#4707,.T.);
#8357=EDGE_CURVE('',#6552,#6550,#753,.T.);
#8358=EDGE_CURVE('',#6549,#6551,#754,.T.);
#8359=EDGE_CURVE('',#6553,#6554,#4708,.T.);
#8360=EDGE_CURVE('',#6554,#6552,#755,.T.);
#8361=EDGE_CURVE('',#6551,#6553,#756,.T.);
#8362=EDGE_CURVE('',#6555,#6556,#4709,.T.);
#8363=EDGE_CURVE('',#6556,#6554,#757,.T.);
#8364=EDGE_CURVE('',#6553,#6555,#758,.T.);
#8365=EDGE_CURVE('',#6557,#6558,#4710,.T.);
#8366=EDGE_CURVE('',#6558,#6556,#759,.T.);
#8367=EDGE_CURVE('',#6555,#6557,#760,.T.);
#8368=EDGE_CURVE('',#6559,#6560,#4711,.T.);
#8369=EDGE_CURVE('',#6560,#6558,#761,.T.);
#8370=EDGE_CURVE('',#6557,#6559,#762,.T.);
#8371=EDGE_CURVE('',#6561,#6562,#4712,.T.);
#8372=EDGE_CURVE('',#6562,#6560,#763,.T.);
#8373=EDGE_CURVE('',#6559,#6561,#764,.T.);
#8374=EDGE_CURVE('',#6563,#6564,#4713,.T.);
#8375=EDGE_CURVE('',#6564,#6562,#765,.T.);
#8376=EDGE_CURVE('',#6561,#6563,#766,.T.);
#8377=EDGE_CURVE('',#6565,#6566,#4714,.T.);
#8378=EDGE_CURVE('',#6566,#6564,#767,.T.);
#8379=EDGE_CURVE('',#6563,#6565,#768,.T.);
#8380=EDGE_CURVE('',#6567,#6568,#4715,.T.);
#8381=EDGE_CURVE('',#6568,#6566,#769,.T.);
#8382=EDGE_CURVE('',#6565,#6567,#770,.T.);
#8383=EDGE_CURVE('',#6569,#6570,#4716,.T.);
#8384=EDGE_CURVE('',#6569,#6571,#771,.T.);
#8385=EDGE_CURVE('',#6572,#6571,#2454,.T.);
#8386=EDGE_CURVE('',#6572,#6570,#772,.T.);
#8387=EDGE_CURVE('',#6573,#6574,#4717,.T.);
#8388=EDGE_CURVE('',#6574,#6575,#773,.T.);
#8389=EDGE_CURVE('',#6576,#6575,#2455,.T.);
#8390=EDGE_CURVE('',#6573,#6576,#774,.T.);
#8391=EDGE_CURVE('',#6577,#6578,#4718,.T.);
#8392=EDGE_CURVE('',#6578,#6574,#775,.T.);
#8393=EDGE_CURVE('',#6577,#6573,#776,.T.);
#8394=EDGE_CURVE('',#6579,#6580,#4719,.T.);
#8395=EDGE_CURVE('',#6580,#6578,#777,.T.);
#8396=EDGE_CURVE('',#6579,#6577,#778,.T.);
#8397=EDGE_CURVE('',#6581,#6582,#4720,.T.);
#8398=EDGE_CURVE('',#6582,#6580,#779,.T.);
#8399=EDGE_CURVE('',#6581,#6579,#780,.T.);
#8400=EDGE_CURVE('',#6583,#6584,#4721,.T.);
#8401=EDGE_CURVE('',#6584,#6582,#781,.T.);
#8402=EDGE_CURVE('',#6583,#6581,#782,.T.);
#8403=EDGE_CURVE('',#6585,#6586,#4722,.T.);
#8404=EDGE_CURVE('',#6586,#6584,#783,.T.);
#8405=EDGE_CURVE('',#6585,#6583,#784,.T.);
#8406=EDGE_CURVE('',#6587,#6588,#4723,.T.);
#8407=EDGE_CURVE('',#6588,#6586,#785,.T.);
#8408=EDGE_CURVE('',#6587,#6585,#786,.T.);
#8409=EDGE_CURVE('',#6589,#6590,#4724,.T.);
#8410=EDGE_CURVE('',#6590,#6588,#787,.T.);
#8411=EDGE_CURVE('',#6589,#6587,#788,.T.);
#8412=EDGE_CURVE('',#6591,#6592,#4725,.T.);
#8413=EDGE_CURVE('',#6592,#6590,#789,.T.);
#8414=EDGE_CURVE('',#6591,#6589,#790,.T.);
#8415=EDGE_CURVE('',#6593,#6594,#4726,.T.);
#8416=EDGE_CURVE('',#6594,#6592,#791,.T.);
#8417=EDGE_CURVE('',#6593,#6591,#792,.T.);
#8418=EDGE_CURVE('',#6595,#6596,#4727,.T.);
#8419=EDGE_CURVE('',#6596,#6594,#793,.T.);
#8420=EDGE_CURVE('',#6595,#6593,#794,.T.);
#8421=EDGE_CURVE('',#6597,#6598,#4728,.T.);
#8422=EDGE_CURVE('',#6598,#6596,#795,.T.);
#8423=EDGE_CURVE('',#6597,#6595,#796,.T.);
#8424=EDGE_CURVE('',#6599,#6600,#4729,.T.);
#8425=EDGE_CURVE('',#6600,#6598,#797,.T.);
#8426=EDGE_CURVE('',#6599,#6597,#798,.T.);
#8427=EDGE_CURVE('',#6601,#6602,#4730,.T.);
#8428=EDGE_CURVE('',#6602,#6600,#799,.T.);
#8429=EDGE_CURVE('',#6601,#6599,#800,.T.);
#8430=EDGE_CURVE('',#6603,#6604,#4731,.T.);
#8431=EDGE_CURVE('',#6604,#6602,#801,.T.);
#8432=EDGE_CURVE('',#6603,#6601,#802,.T.);
#8433=EDGE_CURVE('',#6605,#6606,#4732,.T.);
#8434=EDGE_CURVE('',#6606,#6604,#803,.T.);
#8435=EDGE_CURVE('',#6605,#6603,#804,.T.);
#8436=EDGE_CURVE('',#6607,#6608,#4733,.T.);
#8437=EDGE_CURVE('',#6608,#6606,#805,.T.);
#8438=EDGE_CURVE('',#6607,#6605,#806,.T.);
#8439=EDGE_CURVE('',#6609,#6610,#4734,.T.);
#8440=EDGE_CURVE('',#6610,#6608,#807,.T.);
#8441=EDGE_CURVE('',#6609,#6607,#808,.T.);
#8442=EDGE_CURVE('',#6611,#6612,#4735,.T.);
#8443=EDGE_CURVE('',#6613,#6611,#809,.T.);
#8444=EDGE_CURVE('',#6614,#6613,#2456,.T.);
#8445=EDGE_CURVE('',#6614,#6612,#810,.T.);
#8446=EDGE_CURVE('',#6615,#6616,#4736,.T.);
#8447=EDGE_CURVE('',#6616,#6617,#811,.T.);
#8448=EDGE_CURVE('',#6617,#6618,#2457,.T.);
#8449=EDGE_CURVE('',#6618,#6619,#4737,.T.);
#8450=EDGE_CURVE('',#6619,#6619,#2458,.F.);
#8451=EDGE_CURVE('',#6618,#6620,#2459,.T.);
#8452=EDGE_CURVE('',#6620,#6615,#812,.T.);
#8453=EDGE_CURVE('',#6621,#6622,#4738,.T.);
#8454=EDGE_CURVE('',#6622,#6616,#813,.T.);
#8455=EDGE_CURVE('',#6615,#6621,#814,.T.);
#8456=EDGE_CURVE('',#6623,#6624,#4739,.T.);
#8457=EDGE_CURVE('',#6624,#6622,#815,.T.);
#8458=EDGE_CURVE('',#6621,#6623,#816,.T.);
#8459=EDGE_CURVE('',#6625,#6626,#4740,.T.);
#8460=EDGE_CURVE('',#6626,#6624,#817,.T.);
#8461=EDGE_CURVE('',#6623,#6625,#818,.T.);
#8462=EDGE_CURVE('',#6627,#6628,#4741,.T.);
#8463=EDGE_CURVE('',#6628,#6626,#819,.T.);
#8464=EDGE_CURVE('',#6625,#6627,#820,.T.);
#8465=EDGE_CURVE('',#6629,#6630,#4742,.T.);
#8466=EDGE_CURVE('',#6630,#6628,#821,.T.);
#8467=EDGE_CURVE('',#6627,#6629,#822,.T.);
#8468=EDGE_CURVE('',#6631,#6632,#4743,.T.);
#8469=EDGE_CURVE('',#6632,#6630,#823,.T.);
#8470=EDGE_CURVE('',#6629,#6631,#824,.T.);
#8471=EDGE_CURVE('',#6633,#6634,#4744,.T.);
#8472=EDGE_CURVE('',#6634,#6632,#825,.T.);
#8473=EDGE_CURVE('',#6631,#6633,#826,.T.);
#8474=EDGE_CURVE('',#6635,#6636,#4745,.T.);
#8475=EDGE_CURVE('',#6636,#6634,#827,.T.);
#8476=EDGE_CURVE('',#6633,#6635,#828,.T.);
#8477=EDGE_CURVE('',#6637,#6638,#4746,.T.);
#8478=EDGE_CURVE('',#6638,#6636,#829,.T.);
#8479=EDGE_CURVE('',#6635,#6637,#830,.T.);
#8480=EDGE_CURVE('',#6639,#6640,#4747,.T.);
#8481=EDGE_CURVE('',#6640,#6638,#831,.T.);
#8482=EDGE_CURVE('',#6637,#6639,#832,.T.);
#8483=EDGE_CURVE('',#6641,#6642,#4748,.T.);
#8484=EDGE_CURVE('',#6642,#6640,#833,.T.);
#8485=EDGE_CURVE('',#6639,#6641,#834,.T.);
#8486=EDGE_CURVE('',#6643,#6644,#4749,.T.);
#8487=EDGE_CURVE('',#6644,#6642,#835,.T.);
#8488=EDGE_CURVE('',#6641,#6643,#836,.T.);
#8489=EDGE_CURVE('',#6645,#6646,#4750,.T.);
#8490=EDGE_CURVE('',#6646,#6644,#837,.T.);
#8491=EDGE_CURVE('',#6643,#6645,#838,.T.);
#8492=EDGE_CURVE('',#6647,#6648,#4751,.T.);
#8493=EDGE_CURVE('',#6648,#6646,#839,.T.);
#8494=EDGE_CURVE('',#6645,#6647,#840,.T.);
#8495=EDGE_CURVE('',#6649,#6650,#4752,.T.);
#8496=EDGE_CURVE('',#6650,#6648,#841,.T.);
#8497=EDGE_CURVE('',#6647,#6649,#842,.T.);
#8498=EDGE_CURVE('',#6651,#6652,#4753,.T.);
#8499=EDGE_CURVE('',#6652,#6650,#843,.T.);
#8500=EDGE_CURVE('',#6649,#6651,#844,.T.);
#8501=EDGE_CURVE('',#6653,#6654,#4754,.T.);
#8502=EDGE_CURVE('',#6653,#6655,#845,.T.);
#8503=EDGE_CURVE('',#6656,#6655,#2460,.T.);
#8504=EDGE_CURVE('',#6656,#6654,#846,.T.);
#8505=EDGE_CURVE('',#6657,#6658,#4755,.T.);
#8506=EDGE_CURVE('',#6658,#6659,#847,.T.);
#8507=EDGE_CURVE('',#6660,#6659,#2461,.T.);
#8508=EDGE_CURVE('',#6657,#6660,#848,.T.);
#8509=EDGE_CURVE('',#6661,#6662,#4756,.T.);
#8510=EDGE_CURVE('',#6662,#6658,#849,.T.);
#8511=EDGE_CURVE('',#6661,#6657,#850,.T.);
#8512=EDGE_CURVE('',#6663,#6664,#4757,.T.);
#8513=EDGE_CURVE('',#6664,#6662,#851,.T.);
#8514=EDGE_CURVE('',#6663,#6661,#852,.T.);
#8515=EDGE_CURVE('',#6665,#6666,#4758,.T.);
#8516=EDGE_CURVE('',#6666,#6664,#853,.T.);
#8517=EDGE_CURVE('',#6665,#6663,#854,.T.);
#8518=EDGE_CURVE('',#6667,#6668,#4759,.T.);
#8519=EDGE_CURVE('',#6668,#6666,#855,.T.);
#8520=EDGE_CURVE('',#6667,#6665,#856,.T.);
#8521=EDGE_CURVE('',#6669,#6670,#4760,.T.);
#8522=EDGE_CURVE('',#6670,#6668,#857,.T.);
#8523=EDGE_CURVE('',#6669,#6667,#858,.T.);
#8524=EDGE_CURVE('',#6671,#6672,#4761,.T.);
#8525=EDGE_CURVE('',#6672,#6670,#859,.T.);
#8526=EDGE_CURVE('',#6671,#6669,#860,.T.);
#8527=EDGE_CURVE('',#6673,#6674,#4762,.T.);
#8528=EDGE_CURVE('',#6674,#6672,#861,.T.);
#8529=EDGE_CURVE('',#6673,#6671,#862,.T.);
#8530=EDGE_CURVE('',#6675,#6676,#4763,.T.);
#8531=EDGE_CURVE('',#6676,#6674,#863,.T.);
#8532=EDGE_CURVE('',#6675,#6673,#864,.T.);
#8533=EDGE_CURVE('',#6677,#6678,#4764,.T.);
#8534=EDGE_CURVE('',#6678,#6676,#865,.T.);
#8535=EDGE_CURVE('',#6677,#6675,#866,.T.);
#8536=EDGE_CURVE('',#6679,#6680,#4765,.T.);
#8537=EDGE_CURVE('',#6680,#6678,#867,.T.);
#8538=EDGE_CURVE('',#6679,#6677,#868,.T.);
#8539=EDGE_CURVE('',#6681,#6682,#4766,.T.);
#8540=EDGE_CURVE('',#6682,#6680,#869,.T.);
#8541=EDGE_CURVE('',#6681,#6679,#870,.T.);
#8542=EDGE_CURVE('',#6683,#6684,#4767,.T.);
#8543=EDGE_CURVE('',#6684,#6682,#871,.T.);
#8544=EDGE_CURVE('',#6683,#6681,#872,.T.);
#8545=EDGE_CURVE('',#6685,#6686,#4768,.T.);
#8546=EDGE_CURVE('',#6686,#6684,#873,.T.);
#8547=EDGE_CURVE('',#6685,#6683,#874,.T.);
#8548=EDGE_CURVE('',#6687,#6688,#4769,.T.);
#8549=EDGE_CURVE('',#6688,#6686,#875,.T.);
#8550=EDGE_CURVE('',#6687,#6685,#876,.T.);
#8551=EDGE_CURVE('',#6689,#6690,#4770,.T.);
#8552=EDGE_CURVE('',#6690,#6688,#877,.T.);
#8553=EDGE_CURVE('',#6689,#6687,#878,.T.);
#8554=EDGE_CURVE('',#6691,#6692,#4771,.T.);
#8555=EDGE_CURVE('',#6692,#6690,#879,.T.);
#8556=EDGE_CURVE('',#6691,#6689,#880,.T.);
#8557=EDGE_CURVE('',#6693,#6694,#4772,.T.);
#8558=EDGE_CURVE('',#6694,#6692,#881,.T.);
#8559=EDGE_CURVE('',#6693,#6691,#882,.T.);
#8560=EDGE_CURVE('',#6695,#6696,#4773,.T.);
#8561=EDGE_CURVE('',#6697,#6695,#883,.T.);
#8562=EDGE_CURVE('',#6698,#6697,#2462,.T.);
#8563=EDGE_CURVE('',#6698,#6696,#884,.T.);
#8564=EDGE_CURVE('',#6617,#6660,#885,.T.);
#8565=EDGE_CURVE('',#6659,#6620,#886,.T.);
#8566=EDGE_CURVE('',#6696,#6694,#887,.T.);
#8567=EDGE_CURVE('',#6695,#6693,#888,.T.);
#8568=EDGE_CURVE('',#6655,#6698,#889,.T.);
#8569=EDGE_CURVE('',#6651,#6653,#890,.T.);
#8570=EDGE_CURVE('',#6654,#6652,#891,.T.);
#8571=EDGE_CURVE('',#6697,#6656,#892,.T.);
#8572=EDGE_CURVE('',#6533,#6576,#893,.T.);
#8573=EDGE_CURVE('',#6575,#6536,#894,.T.);
#8574=EDGE_CURVE('',#6612,#6610,#895,.T.);
#8575=EDGE_CURVE('',#6611,#6609,#896,.T.);
#8576=EDGE_CURVE('',#6571,#6614,#897,.T.);
#8577=EDGE_CURVE('',#6567,#6569,#898,.T.);
#8578=EDGE_CURVE('',#6570,#6568,#899,.T.);
#8579=EDGE_CURVE('',#6613,#6572,#900,.T.);
#8580=EDGE_CURVE('',#6449,#6492,#901,.T.);
#8581=EDGE_CURVE('',#6491,#6452,#902,.T.);
#8582=EDGE_CURVE('',#6528,#6526,#903,.T.);
#8583=EDGE_CURVE('',#6527,#6525,#904,.T.);
#8584=EDGE_CURVE('',#6487,#6530,#905,.T.);
#8585=EDGE_CURVE('',#6483,#6485,#906,.T.);
#8586=EDGE_CURVE('',#6486,#6484,#907,.T.);
#8587=EDGE_CURVE('',#6529,#6488,#908,.T.);
#8588=EDGE_CURVE('',#6365,#6408,#909,.T.);
#8589=EDGE_CURVE('',#6407,#6368,#910,.T.);
#8590=EDGE_CURVE('',#6444,#6442,#911,.T.);
#8591=EDGE_CURVE('',#6443,#6441,#912,.T.);
#8592=EDGE_CURVE('',#6403,#6446,#913,.T.);
#8593=EDGE_CURVE('',#6399,#6401,#914,.T.);
#8594=EDGE_CURVE('',#6402,#6400,#915,.T.);
#8595=EDGE_CURVE('',#6445,#6404,#916,.T.);
#8596=EDGE_CURVE('',#6281,#6324,#917,.T.);
#8597=EDGE_CURVE('',#6323,#6284,#918,.T.);
#8598=EDGE_CURVE('',#6360,#6358,#919,.T.);
#8599=EDGE_CURVE('',#6359,#6357,#920,.T.);
#8600=EDGE_CURVE('',#6319,#6362,#921,.T.);
#8601=EDGE_CURVE('',#6315,#6317,#922,.T.);
#8602=EDGE_CURVE('',#6318,#6316,#923,.T.);
#8603=EDGE_CURVE('',#6361,#6320,#924,.T.);
#8604=EDGE_CURVE('',#6197,#6240,#925,.T.);
#8605=EDGE_CURVE('',#6239,#6200,#926,.T.);
#8606=EDGE_CURVE('',#6276,#6274,#927,.T.);
#8607=EDGE_CURVE('',#6275,#6273,#928,.T.);
#8608=EDGE_CURVE('',#6235,#6278,#929,.T.);
#8609=EDGE_CURVE('',#6231,#6233,#930,.T.);
#8610=EDGE_CURVE('',#6234,#6232,#931,.T.);
#8611=EDGE_CURVE('',#6277,#6236,#932,.T.);
#8612=EDGE_CURVE('',#6113,#6156,#933,.T.);
#8613=EDGE_CURVE('',#6155,#6116,#934,.T.);
#8614=EDGE_CURVE('',#6192,#6190,#935,.T.);
#8615=EDGE_CURVE('',#6191,#6189,#936,.T.);
#8616=EDGE_CURVE('',#6151,#6194,#937,.T.);
#8617=EDGE_CURVE('',#6147,#6149,#938,.T.);
#8618=EDGE_CURVE('',#6150,#6148,#939,.T.);
#8619=EDGE_CURVE('',#6193,#6152,#940,.T.);
#8620=EDGE_CURVE('',#6029,#6072,#941,.T.);
#8621=EDGE_CURVE('',#6071,#6032,#942,.T.);
#8622=EDGE_CURVE('',#6108,#6106,#943,.T.);
#8623=EDGE_CURVE('',#6107,#6105,#944,.T.);
#8624=EDGE_CURVE('',#6067,#6110,#945,.T.);
#8625=EDGE_CURVE('',#6063,#6065,#946,.T.);
#8626=EDGE_CURVE('',#6066,#6064,#947,.T.);
#8627=EDGE_CURVE('',#6109,#6068,#948,.T.);
#8628=EDGE_CURVE('',#6699,#6700,#4774,.T.);
#8629=EDGE_CURVE('',#6701,#6699,#4775,.T.);
#8630=EDGE_CURVE('',#6701,#6702,#4776,.T.);
#8631=EDGE_CURVE('',#6700,#6702,#4777,.T.);
#8632=EDGE_CURVE('',#6703,#6701,#4778,.T.);
#8633=EDGE_CURVE('',#6703,#6704,#4779,.T.);
#8634=EDGE_CURVE('',#6702,#6704,#4780,.T.);
#8635=EDGE_CURVE('',#6705,#6706,#4781,.T.);
#8636=EDGE_CURVE('',#6704,#6705,#4782,.T.);
#8637=EDGE_CURVE('',#6706,#6703,#4783,.T.);
#8638=EDGE_CURVE('',#6700,#6705,#2463,.T.);
#8639=EDGE_CURVE('',#6707,#6707,#2464,.T.);
#8640=EDGE_CURVE('',#6024,#6022,#949,.T.);
#8641=EDGE_CURVE('',#6023,#6021,#950,.T.);
#8642=EDGE_CURVE('',#6011,#5993,#951,.T.);
#8643=EDGE_CURVE('',#6007,#6026,#952,.T.);
#8644=EDGE_CURVE('',#6003,#6005,#953,.T.);
#8645=EDGE_CURVE('',#5996,#6012,#954,.T.);
#8646=EDGE_CURVE('',#6006,#6004,#955,.T.);
#8647=EDGE_CURVE('',#6025,#6008,#956,.T.);
#8648=EDGE_CURVE('',#6708,#6709,#2465,.T.);
#8649=EDGE_CURVE('',#6708,#6710,#4784,.T.);
#8650=EDGE_CURVE('',#6710,#6711,#4785,.T.);
#8651=EDGE_CURVE('',#6711,#6709,#4786,.T.);
#8652=EDGE_CURVE('',#6712,#6708,#4787,.T.);
#8653=EDGE_CURVE('',#6712,#6713,#4788,.T.);
#8654=EDGE_CURVE('',#6713,#6710,#4789,.T.);
#8655=EDGE_CURVE('',#6709,#6714,#4790,.T.);
#8656=EDGE_CURVE('',#6715,#6711,#4791,.T.);
#8657=EDGE_CURVE('',#6715,#6714,#4792,.T.);
#8658=EDGE_CURVE('',#6713,#6715,#4793,.T.);
#8659=EDGE_CURVE('',#6714,#6712,#2466,.T.);
#8660=EDGE_CURVE('',#6716,#6716,#2467,.T.);
#8661=EDGE_CURVE('',#6717,#6717,#2468,.T.);
#8662=EDGE_CURVE('',#6718,#6718,#2469,.T.);
#8663=EDGE_CURVE('',#6719,#6719,#2470,.T.);
#8664=EDGE_CURVE('',#6717,#6719,#4794,.T.);
#8665=EDGE_CURVE('',#6718,#6720,#4795,.T.);
#8666=EDGE_CURVE('',#6720,#6720,#2471,.T.);
#8667=EDGE_CURVE('',#6721,#6721,#2472,.T.);
#8668=EDGE_CURVE('',#6722,#6722,#2473,.T.);
#8669=EDGE_CURVE('',#6723,#6723,#2474,.T.);
#8670=EDGE_CURVE('',#6721,#6723,#4796,.T.);
#8671=EDGE_CURVE('',#6722,#6707,#4797,.T.);
#8672=EDGE_CURVE('',#6724,#6724,#2475,.T.);
#8673=EDGE_CURVE('',#6724,#6716,#4798,.T.);
#8674=EDGE_CURVE('',#6699,#6706,#2476,.T.);
#8675=EDGE_CURVE('',#6725,#6726,#4799,.T.);
#8676=EDGE_CURVE('',#6726,#6727,#957,.T.);
#8677=EDGE_CURVE('',#6727,#6728,#2477,.F.);
#8678=EDGE_CURVE('',#6728,#6729,#2478,.F.);
#8679=EDGE_CURVE('',#6729,#6725,#958,.T.);
#8680=EDGE_CURVE('',#6730,#6731,#4800,.T.);
#8681=EDGE_CURVE('',#6731,#6726,#959,.T.);
#8682=EDGE_CURVE('',#6725,#6730,#960,.T.);
#8683=EDGE_CURVE('',#6732,#6733,#4801,.T.);
#8684=EDGE_CURVE('',#6733,#6731,#961,.T.);
#8685=EDGE_CURVE('',#6730,#6732,#962,.T.);
#8686=EDGE_CURVE('',#6734,#6735,#4802,.T.);
#8687=EDGE_CURVE('',#6735,#6733,#963,.T.);
#8688=EDGE_CURVE('',#6732,#6734,#964,.T.);
#8689=EDGE_CURVE('',#6736,#6737,#4803,.T.);
#8690=EDGE_CURVE('',#6737,#6735,#965,.T.);
#8691=EDGE_CURVE('',#6734,#6736,#966,.T.);
#8692=EDGE_CURVE('',#6738,#6739,#4804,.T.);
#8693=EDGE_CURVE('',#6739,#6737,#967,.T.);
#8694=EDGE_CURVE('',#6736,#6738,#968,.T.);
#8695=EDGE_CURVE('',#6740,#6741,#4805,.T.);
#8696=EDGE_CURVE('',#6741,#6739,#969,.T.);
#8697=EDGE_CURVE('',#6738,#6740,#970,.T.);
#8698=EDGE_CURVE('',#6742,#6743,#4806,.T.);
#8699=EDGE_CURVE('',#6743,#6741,#971,.T.);
#8700=EDGE_CURVE('',#6740,#6742,#972,.T.);
#8701=EDGE_CURVE('',#6744,#6745,#4807,.T.);
#8702=EDGE_CURVE('',#6745,#6743,#973,.T.);
#8703=EDGE_CURVE('',#6742,#6744,#974,.T.);
#8704=EDGE_CURVE('',#6746,#6747,#4808,.T.);
#8705=EDGE_CURVE('',#6747,#6745,#975,.T.);
#8706=EDGE_CURVE('',#6744,#6746,#976,.T.);
#8707=EDGE_CURVE('',#6748,#6749,#4809,.T.);
#8708=EDGE_CURVE('',#6749,#6747,#977,.T.);
#8709=EDGE_CURVE('',#6746,#6748,#978,.T.);
#8710=EDGE_CURVE('',#6750,#6751,#4810,.T.);
#8711=EDGE_CURVE('',#6751,#6749,#979,.T.);
#8712=EDGE_CURVE('',#6748,#6750,#980,.T.);
#8713=EDGE_CURVE('',#6752,#6753,#4811,.T.);
#8714=EDGE_CURVE('',#6753,#6751,#981,.T.);
#8715=EDGE_CURVE('',#6750,#6752,#982,.T.);
#8716=EDGE_CURVE('',#6754,#6755,#4812,.T.);
#8717=EDGE_CURVE('',#6755,#6753,#983,.T.);
#8718=EDGE_CURVE('',#6752,#6754,#984,.T.);
#8719=EDGE_CURVE('',#6756,#6757,#4813,.T.);
#8720=EDGE_CURVE('',#6757,#6755,#985,.T.);
#8721=EDGE_CURVE('',#6754,#6756,#986,.T.);
#8722=EDGE_CURVE('',#6758,#6759,#4814,.T.);
#8723=EDGE_CURVE('',#6759,#6757,#987,.T.);
#8724=EDGE_CURVE('',#6756,#6758,#988,.T.);
#8725=EDGE_CURVE('',#6760,#6761,#4815,.T.);
#8726=EDGE_CURVE('',#6761,#6759,#989,.T.);
#8727=EDGE_CURVE('',#6758,#6760,#990,.T.);
#8728=EDGE_CURVE('',#6762,#6763,#4816,.T.);
#8729=EDGE_CURVE('',#6762,#6764,#991,.T.);
#8730=EDGE_CURVE('',#6765,#6764,#992,.T.);
#8731=EDGE_CURVE('',#6765,#6763,#993,.T.);
#8732=EDGE_CURVE('',#6766,#6767,#4817,.T.);
#8733=EDGE_CURVE('',#6767,#6768,#994,.T.);
#8734=EDGE_CURVE('',#6769,#6768,#2479,.T.);
#8735=EDGE_CURVE('',#6770,#6769,#2480,.T.);
#8736=EDGE_CURVE('',#6766,#6770,#995,.T.);
#8737=EDGE_CURVE('',#6771,#6772,#4818,.T.);
#8738=EDGE_CURVE('',#6772,#6767,#996,.T.);
#8739=EDGE_CURVE('',#6771,#6766,#997,.T.);
#8740=EDGE_CURVE('',#6773,#6774,#4819,.T.);
#8741=EDGE_CURVE('',#6774,#6772,#998,.T.);
#8742=EDGE_CURVE('',#6773,#6771,#999,.T.);
#8743=EDGE_CURVE('',#6775,#6776,#4820,.T.);
#8744=EDGE_CURVE('',#6776,#6774,#1000,.T.);
#8745=EDGE_CURVE('',#6775,#6773,#1001,.T.);
#8746=EDGE_CURVE('',#6777,#6778,#4821,.T.);
#8747=EDGE_CURVE('',#6778,#6776,#1002,.T.);
#8748=EDGE_CURVE('',#6777,#6775,#1003,.T.);
#8749=EDGE_CURVE('',#6779,#6780,#4822,.T.);
#8750=EDGE_CURVE('',#6780,#6778,#1004,.T.);
#8751=EDGE_CURVE('',#6779,#6777,#1005,.T.);
#8752=EDGE_CURVE('',#6781,#6782,#4823,.T.);
#8753=EDGE_CURVE('',#6782,#6780,#1006,.T.);
#8754=EDGE_CURVE('',#6781,#6779,#1007,.T.);
#8755=EDGE_CURVE('',#6783,#6784,#4824,.T.);
#8756=EDGE_CURVE('',#6784,#6782,#1008,.T.);
#8757=EDGE_CURVE('',#6783,#6781,#1009,.T.);
#8758=EDGE_CURVE('',#6785,#6786,#4825,.T.);
#8759=EDGE_CURVE('',#6786,#6784,#1010,.T.);
#8760=EDGE_CURVE('',#6785,#6783,#1011,.T.);
#8761=EDGE_CURVE('',#6787,#6788,#4826,.T.);
#8762=EDGE_CURVE('',#6788,#6786,#1012,.T.);
#8763=EDGE_CURVE('',#6787,#6785,#1013,.T.);
#8764=EDGE_CURVE('',#6789,#6790,#4827,.T.);
#8765=EDGE_CURVE('',#6790,#6788,#1014,.T.);
#8766=EDGE_CURVE('',#6789,#6787,#1015,.T.);
#8767=EDGE_CURVE('',#6791,#6792,#4828,.T.);
#8768=EDGE_CURVE('',#6792,#6790,#1016,.T.);
#8769=EDGE_CURVE('',#6791,#6789,#1017,.T.);
#8770=EDGE_CURVE('',#6793,#6794,#4829,.T.);
#8771=EDGE_CURVE('',#6794,#6792,#1018,.T.);
#8772=EDGE_CURVE('',#6793,#6791,#1019,.T.);
#8773=EDGE_CURVE('',#6795,#6796,#4830,.T.);
#8774=EDGE_CURVE('',#6796,#6794,#1020,.T.);
#8775=EDGE_CURVE('',#6795,#6793,#1021,.T.);
#8776=EDGE_CURVE('',#6797,#6798,#4831,.T.);
#8777=EDGE_CURVE('',#6798,#6796,#1022,.T.);
#8778=EDGE_CURVE('',#6797,#6795,#1023,.T.);
#8779=EDGE_CURVE('',#6799,#6800,#4832,.T.);
#8780=EDGE_CURVE('',#6800,#6798,#1024,.T.);
#8781=EDGE_CURVE('',#6799,#6797,#1025,.T.);
#8782=EDGE_CURVE('',#6801,#6802,#4833,.T.);
#8783=EDGE_CURVE('',#6802,#6800,#1026,.T.);
#8784=EDGE_CURVE('',#6801,#6799,#1027,.T.);
#8785=EDGE_CURVE('',#6803,#6804,#4834,.T.);
#8786=EDGE_CURVE('',#6805,#6803,#1028,.T.);
#8787=EDGE_CURVE('',#6806,#6805,#1029,.T.);
#8788=EDGE_CURVE('',#6807,#6806,#1030,.T.);
#8789=EDGE_CURVE('',#6807,#6804,#1031,.T.);
#8790=EDGE_CURVE('',#6808,#6808,#2481,.T.);
#8791=EDGE_CURVE('',#6808,#6809,#4835,.T.);
#8792=EDGE_CURVE('',#6809,#6809,#2482,.T.);
#8793=EDGE_CURVE('',#6810,#6810,#2483,.T.);
#8794=EDGE_CURVE('',#6811,#6811,#2484,.T.);
#8795=EDGE_CURVE('',#6812,#6812,#2485,.T.);
#8796=EDGE_CURVE('',#6812,#6811,#4836,.T.);
#8797=EDGE_CURVE('',#6813,#6814,#4837,.T.);
#8798=EDGE_CURVE('',#6815,#6813,#4838,.T.);
#8799=EDGE_CURVE('',#6816,#6815,#4839,.T.);
#8800=EDGE_CURVE('',#6814,#6816,#4840,.T.);
#8801=EDGE_CURVE('',#6817,#6816,#4841,.T.);
#8802=EDGE_CURVE('',#6815,#6818,#4842,.T.);
#8803=EDGE_CURVE('',#6818,#6817,#4843,.T.);
#8804=EDGE_CURVE('',#6814,#6819,#2486,.T.);
#8805=EDGE_CURVE('',#6817,#6819,#4844,.T.);
#8806=EDGE_CURVE('',#6819,#6820,#4845,.T.);
#8807=EDGE_CURVE('',#6820,#6818,#4846,.T.);
#8808=EDGE_CURVE('',#6813,#6821,#2487,.T.);
#8809=EDGE_CURVE('',#6821,#6820,#2488,.T.);
#8810=EDGE_CURVE('',#6764,#6807,#1032,.T.);
#8811=EDGE_CURVE('',#6760,#6762,#1033,.T.);
#8812=EDGE_CURVE('',#6768,#6729,#1034,.T.);
#8813=EDGE_CURVE('',#6804,#6802,#1035,.T.);
#8814=EDGE_CURVE('',#6803,#6801,#1036,.T.);
#8815=EDGE_CURVE('',#6805,#6765,#1037,.T.);
#8816=EDGE_CURVE('',#6727,#6770,#1038,.T.);
#8817=EDGE_CURVE('',#6763,#6761,#1039,.T.);
#8818=EDGE_CURVE('',#6728,#6769,#4847,.T.);
#8819=EDGE_CURVE('',#6728,#6769,#4848,.T.);
#8820=EDGE_CURVE('',#6822,#6822,#2489,.T.);
#8821=EDGE_CURVE('',#6822,#6769,#4849,.T.);
#8822=EDGE_CURVE('',#6728,#6823,#4850,.T.);
#8823=EDGE_CURVE('',#6823,#6823,#2490,.T.);
#8824=EDGE_CURVE('',#6824,#6824,#2491,.T.);
#8825=EDGE_CURVE('',#6824,#6821,#4851,.T.);
#8826=EDGE_CURVE('',#6825,#6825,#2492,.T.);
#8827=EDGE_CURVE('',#6826,#6826,#2493,.T.);
#8828=EDGE_CURVE('',#6827,#6827,#2494,.T.);
#8829=EDGE_CURVE('',#6828,#6828,#2495,.T.);
#8830=EDGE_CURVE('',#6825,#6827,#4852,.T.);
#8831=EDGE_CURVE('',#6828,#6829,#4853,.T.);
#8832=EDGE_CURVE('',#6829,#6829,#2496,.T.);
#8833=EDGE_CURVE('',#6830,#6830,#2497,.T.);
#8834=EDGE_CURVE('',#6830,#6831,#4854,.T.);
#8835=EDGE_CURVE('',#6831,#6831,#2498,.T.);
#8836=EDGE_CURVE('',#6810,#6826,#4855,.T.);
#8837=EDGE_CURVE('',#6832,#6832,#2499,.T.);
#8838=EDGE_CURVE('',#6832,#6833,#4856,.T.);
#8839=EDGE_CURVE('',#6833,#6833,#2500,.T.);
#8840=EDGE_CURVE('',#6834,#6834,#2501,.T.);
#8841=EDGE_CURVE('',#6834,#6835,#4857,.T.);
#8842=EDGE_CURVE('',#6835,#6835,#2502,.T.);
#8843=EDGE_CURVE('',#6836,#6836,#2503,.T.);
#8844=EDGE_CURVE('',#6836,#6837,#4858,.T.);
#8845=EDGE_CURVE('',#6837,#6837,#2504,.T.);
#8846=EDGE_CURVE('',#6838,#6838,#2505,.T.);
#8847=EDGE_CURVE('',#6838,#6839,#4859,.T.);
#8848=EDGE_CURVE('',#6839,#6839,#2506,.T.);
#8849=EDGE_CURVE('',#6840,#6841,#4860,.T.);
#8850=EDGE_CURVE('',#6842,#6840,#4861,.T.);
#8851=EDGE_CURVE('',#6843,#6842,#4862,.T.);
#8852=EDGE_CURVE('',#6841,#6843,#4863,.T.);
#8853=EDGE_CURVE('',#6844,#6845,#4864,.T.);
#8854=EDGE_CURVE('',#6846,#6844,#4865,.T.);
#8855=EDGE_CURVE('',#6847,#6846,#4866,.T.);
#8856=EDGE_CURVE('',#6845,#6847,#4867,.T.);
#8857=EDGE_CURVE('',#6842,#6847,#2507,.T.);
#8858=EDGE_CURVE('',#6845,#6840,#2508,.T.);
#8859=EDGE_CURVE('',#6844,#6841,#2509,.T.);
#8860=EDGE_CURVE('',#6843,#6846,#2510,.T.);
#8861=EDGE_CURVE('',#6848,#6849,#4868,.T.);
#8862=EDGE_CURVE('',#6849,#6850,#4869,.T.);
#8863=EDGE_CURVE('',#6851,#6850,#4870,.T.);
#8864=EDGE_CURVE('',#6848,#6851,#4871,.T.);
#8865=EDGE_CURVE('',#6852,#6848,#4872,.T.);
#8866=EDGE_CURVE('',#6853,#6851,#4873,.T.);
#8867=EDGE_CURVE('',#6852,#6853,#4874,.T.);
#8868=EDGE_CURVE('',#6854,#6852,#4875,.T.);
#8869=EDGE_CURVE('',#6855,#6853,#4876,.T.);
#8870=EDGE_CURVE('',#6854,#6855,#4877,.T.);
#8871=EDGE_CURVE('',#6849,#6854,#4878,.T.);
#8872=EDGE_CURVE('',#6850,#6855,#4879,.T.);
#8873=EDGE_CURVE('',#6856,#6857,#4880,.T.);
#8874=EDGE_CURVE('',#6856,#6858,#1040,.T.);
#8875=EDGE_CURVE('',#6858,#6859,#2511,.T.);
#8876=EDGE_CURVE('',#6859,#6857,#1041,.T.);
#8877=EDGE_CURVE('',#6860,#6861,#4881,.T.);
#8878=EDGE_CURVE('',#6860,#6856,#1042,.T.);
#8879=EDGE_CURVE('',#6857,#6861,#1043,.T.);
#8880=EDGE_CURVE('',#6862,#6863,#4882,.T.);
#8881=EDGE_CURVE('',#6862,#6860,#1044,.T.);
#8882=EDGE_CURVE('',#6861,#6863,#1045,.T.);
#8883=EDGE_CURVE('',#6864,#6865,#4883,.T.);
#8884=EDGE_CURVE('',#6864,#6862,#1046,.T.);
#8885=EDGE_CURVE('',#6863,#6865,#1047,.T.);
#8886=EDGE_CURVE('',#6866,#6867,#4884,.T.);
#8887=EDGE_CURVE('',#6866,#6864,#1048,.T.);
#8888=EDGE_CURVE('',#6865,#6867,#1049,.T.);
#8889=EDGE_CURVE('',#6868,#6869,#4885,.T.);
#8890=EDGE_CURVE('',#6868,#6866,#1050,.T.);
#8891=EDGE_CURVE('',#6867,#6869,#1051,.T.);
#8892=EDGE_CURVE('',#6870,#6871,#4886,.T.);
#8893=EDGE_CURVE('',#6870,#6868,#1052,.T.);
#8894=EDGE_CURVE('',#6869,#6871,#1053,.T.);
#8895=EDGE_CURVE('',#6872,#6873,#4887,.T.);
#8896=EDGE_CURVE('',#6872,#6870,#1054,.T.);
#8897=EDGE_CURVE('',#6871,#6873,#1055,.T.);
#8898=EDGE_CURVE('',#6874,#6875,#4888,.T.);
#8899=EDGE_CURVE('',#6874,#6872,#1056,.T.);
#8900=EDGE_CURVE('',#6873,#6875,#1057,.T.);
#8901=EDGE_CURVE('',#6876,#6877,#4889,.T.);
#8902=EDGE_CURVE('',#6876,#6874,#1058,.T.);
#8903=EDGE_CURVE('',#6875,#6877,#1059,.T.);
#8904=EDGE_CURVE('',#6878,#6879,#4890,.T.);
#8905=EDGE_CURVE('',#6878,#6876,#1060,.T.);
#8906=EDGE_CURVE('',#6877,#6879,#1061,.T.);
#8907=EDGE_CURVE('',#6880,#6881,#4891,.T.);
#8908=EDGE_CURVE('',#6880,#6878,#1062,.T.);
#8909=EDGE_CURVE('',#6879,#6881,#1063,.T.);
#8910=EDGE_CURVE('',#6882,#6883,#4892,.T.);
#8911=EDGE_CURVE('',#6882,#6880,#1064,.T.);
#8912=EDGE_CURVE('',#6881,#6883,#1065,.T.);
#8913=EDGE_CURVE('',#6884,#6885,#4893,.T.);
#8914=EDGE_CURVE('',#6884,#6882,#1066,.T.);
#8915=EDGE_CURVE('',#6883,#6885,#1067,.T.);
#8916=EDGE_CURVE('',#6886,#6887,#4894,.T.);
#8917=EDGE_CURVE('',#6886,#6884,#1068,.T.);
#8918=EDGE_CURVE('',#6885,#6887,#1069,.T.);
#8919=EDGE_CURVE('',#6888,#6889,#4895,.T.);
#8920=EDGE_CURVE('',#6888,#6886,#1070,.T.);
#8921=EDGE_CURVE('',#6887,#6889,#1071,.T.);
#8922=EDGE_CURVE('',#6890,#6891,#4896,.T.);
#8923=EDGE_CURVE('',#6890,#6888,#1072,.T.);
#8924=EDGE_CURVE('',#6889,#6891,#1073,.T.);
#8925=EDGE_CURVE('',#6892,#6893,#4897,.T.);
#8926=EDGE_CURVE('',#6892,#6890,#1074,.T.);
#8927=EDGE_CURVE('',#6891,#6893,#1075,.T.);
#8928=EDGE_CURVE('',#6894,#6895,#4898,.T.);
#8929=EDGE_CURVE('',#6894,#6892,#1076,.T.);
#8930=EDGE_CURVE('',#6893,#6895,#1077,.T.);
#8931=EDGE_CURVE('',#6896,#6897,#4899,.T.);
#8932=EDGE_CURVE('',#6896,#6894,#1078,.T.);
#8933=EDGE_CURVE('',#6895,#6897,#1079,.T.);
#8934=EDGE_CURVE('',#6898,#6899,#4900,.T.);
#8935=EDGE_CURVE('',#6898,#6896,#1080,.T.);
#8936=EDGE_CURVE('',#6897,#6899,#1081,.T.);
#8937=EDGE_CURVE('',#6900,#6901,#4901,.T.);
#8938=EDGE_CURVE('',#6900,#6898,#1082,.T.);
#8939=EDGE_CURVE('',#6899,#6901,#1083,.T.);
#8940=EDGE_CURVE('',#6902,#6903,#4902,.T.);
#8941=EDGE_CURVE('',#6902,#6900,#1084,.T.);
#8942=EDGE_CURVE('',#6901,#6903,#1085,.T.);
#8943=EDGE_CURVE('',#6904,#6905,#4903,.T.);
#8944=EDGE_CURVE('',#6904,#6902,#1086,.T.);
#8945=EDGE_CURVE('',#6903,#6905,#1087,.T.);
#8946=EDGE_CURVE('',#6906,#6907,#4904,.T.);
#8947=EDGE_CURVE('',#6906,#6904,#1088,.T.);
#8948=EDGE_CURVE('',#6905,#6907,#1089,.T.);
#8949=EDGE_CURVE('',#6908,#6909,#4905,.T.);
#8950=EDGE_CURVE('',#6908,#6906,#1090,.T.);
#8951=EDGE_CURVE('',#6907,#6909,#1091,.T.);
#8952=EDGE_CURVE('',#6910,#6911,#4906,.T.);
#8953=EDGE_CURVE('',#6910,#6908,#1092,.T.);
#8954=EDGE_CURVE('',#6909,#6911,#1093,.T.);
#8955=EDGE_CURVE('',#6912,#6913,#4907,.T.);
#8956=EDGE_CURVE('',#6912,#6910,#1094,.T.);
#8957=EDGE_CURVE('',#6911,#6913,#1095,.T.);
#8958=EDGE_CURVE('',#6914,#6915,#4908,.T.);
#8959=EDGE_CURVE('',#6914,#6912,#1096,.T.);
#8960=EDGE_CURVE('',#6913,#6915,#1097,.T.);
#8961=EDGE_CURVE('',#6916,#6917,#4909,.T.);
#8962=EDGE_CURVE('',#6916,#6914,#1098,.T.);
#8963=EDGE_CURVE('',#6915,#6917,#1099,.T.);
#8964=EDGE_CURVE('',#6918,#6919,#4910,.T.);
#8965=EDGE_CURVE('',#6918,#6916,#1100,.T.);
#8966=EDGE_CURVE('',#6917,#6919,#1101,.T.);
#8967=EDGE_CURVE('',#6920,#6921,#4911,.T.);
#8968=EDGE_CURVE('',#6920,#6918,#1102,.T.);
#8969=EDGE_CURVE('',#6919,#6921,#1103,.T.);
#8970=EDGE_CURVE('',#6922,#6923,#4912,.T.);
#8971=EDGE_CURVE('',#6922,#6920,#1104,.T.);
#8972=EDGE_CURVE('',#6921,#6923,#1105,.T.);
#8973=EDGE_CURVE('',#6924,#6925,#4913,.T.);
#8974=EDGE_CURVE('',#6924,#6922,#1106,.T.);
#8975=EDGE_CURVE('',#6923,#6925,#1107,.T.);
#8976=EDGE_CURVE('',#6926,#6927,#4914,.T.);
#8977=EDGE_CURVE('',#6926,#6924,#1108,.T.);
#8978=EDGE_CURVE('',#6925,#6927,#1109,.T.);
#8979=EDGE_CURVE('',#6928,#6929,#4915,.T.);
#8980=EDGE_CURVE('',#6928,#6926,#1110,.T.);
#8981=EDGE_CURVE('',#6927,#6929,#1111,.T.);
#8982=EDGE_CURVE('',#6930,#6931,#4916,.T.);
#8983=EDGE_CURVE('',#6930,#6928,#1112,.T.);
#8984=EDGE_CURVE('',#6929,#6931,#1113,.T.);
#8985=EDGE_CURVE('',#6932,#6933,#4917,.T.);
#8986=EDGE_CURVE('',#6932,#6930,#1114,.T.);
#8987=EDGE_CURVE('',#6931,#6933,#1115,.T.);
#8988=EDGE_CURVE('',#6934,#6935,#4918,.T.);
#8989=EDGE_CURVE('',#6934,#6932,#1116,.T.);
#8990=EDGE_CURVE('',#6933,#6935,#1117,.T.);
#8991=EDGE_CURVE('',#6936,#6937,#4919,.T.);
#8992=EDGE_CURVE('',#6936,#6934,#1118,.T.);
#8993=EDGE_CURVE('',#6935,#6937,#1119,.T.);
#8994=EDGE_CURVE('',#6938,#6939,#4920,.T.);
#8995=EDGE_CURVE('',#6938,#6936,#1120,.T.);
#8996=EDGE_CURVE('',#6937,#6939,#1121,.T.);
#8997=EDGE_CURVE('',#6940,#6941,#4921,.T.);
#8998=EDGE_CURVE('',#6940,#6938,#1122,.T.);
#8999=EDGE_CURVE('',#6939,#6941,#1123,.T.);
#9000=EDGE_CURVE('',#6942,#6943,#4922,.T.);
#9001=EDGE_CURVE('',#6942,#6940,#1124,.T.);
#9002=EDGE_CURVE('',#6941,#6943,#1125,.T.);
#9003=EDGE_CURVE('',#6944,#6945,#4923,.T.);
#9004=EDGE_CURVE('',#6944,#6942,#1126,.T.);
#9005=EDGE_CURVE('',#6943,#6945,#1127,.T.);
#9006=EDGE_CURVE('',#6946,#6947,#4924,.T.);
#9007=EDGE_CURVE('',#6946,#6944,#1128,.T.);
#9008=EDGE_CURVE('',#6945,#6947,#1129,.T.);
#9009=EDGE_CURVE('',#6948,#6949,#4925,.T.);
#9010=EDGE_CURVE('',#6948,#6946,#1130,.T.);
#9011=EDGE_CURVE('',#6947,#6949,#1131,.T.);
#9012=EDGE_CURVE('',#6950,#6951,#4926,.T.);
#9013=EDGE_CURVE('',#6950,#6948,#1132,.T.);
#9014=EDGE_CURVE('',#6949,#6951,#1133,.T.);
#9015=EDGE_CURVE('',#6952,#6953,#4927,.T.);
#9016=EDGE_CURVE('',#6952,#6950,#1134,.T.);
#9017=EDGE_CURVE('',#6951,#6953,#1135,.T.);
#9018=EDGE_CURVE('',#6954,#6955,#4928,.T.);
#9019=EDGE_CURVE('',#6954,#6952,#1136,.T.);
#9020=EDGE_CURVE('',#6953,#6955,#1137,.T.);
#9021=EDGE_CURVE('',#6956,#6957,#4929,.T.);
#9022=EDGE_CURVE('',#6956,#6954,#1138,.T.);
#9023=EDGE_CURVE('',#6955,#6957,#1139,.T.);
#9024=EDGE_CURVE('',#6958,#6959,#4930,.T.);
#9025=EDGE_CURVE('',#6958,#6956,#1140,.T.);
#9026=EDGE_CURVE('',#6957,#6959,#1141,.T.);
#9027=EDGE_CURVE('',#6960,#6961,#4931,.T.);
#9028=EDGE_CURVE('',#6960,#6958,#1142,.T.);
#9029=EDGE_CURVE('',#6959,#6961,#1143,.T.);
#9030=EDGE_CURVE('',#6962,#6963,#4932,.T.);
#9031=EDGE_CURVE('',#6962,#6960,#1144,.T.);
#9032=EDGE_CURVE('',#6961,#6963,#1145,.T.);
#9033=EDGE_CURVE('',#6964,#6965,#4933,.T.);
#9034=EDGE_CURVE('',#6964,#6962,#1146,.T.);
#9035=EDGE_CURVE('',#6963,#6965,#1147,.T.);
#9036=EDGE_CURVE('',#6966,#6967,#4934,.T.);
#9037=EDGE_CURVE('',#6966,#6964,#1148,.T.);
#9038=EDGE_CURVE('',#6965,#6967,#1149,.T.);
#9039=EDGE_CURVE('',#6968,#6969,#4935,.T.);
#9040=EDGE_CURVE('',#6968,#6966,#1150,.T.);
#9041=EDGE_CURVE('',#6967,#6969,#1151,.T.);
#9042=EDGE_CURVE('',#6970,#6971,#4936,.T.);
#9043=EDGE_CURVE('',#6970,#6968,#1152,.T.);
#9044=EDGE_CURVE('',#6969,#6971,#1153,.T.);
#9045=EDGE_CURVE('',#6972,#6973,#4937,.T.);
#9046=EDGE_CURVE('',#6972,#6970,#1154,.T.);
#9047=EDGE_CURVE('',#6971,#6973,#1155,.T.);
#9048=EDGE_CURVE('',#6974,#6975,#4938,.T.);
#9049=EDGE_CURVE('',#6974,#6972,#1156,.T.);
#9050=EDGE_CURVE('',#6973,#6975,#1157,.T.);
#9051=EDGE_CURVE('',#6976,#6977,#4939,.T.);
#9052=EDGE_CURVE('',#6976,#6974,#1158,.T.);
#9053=EDGE_CURVE('',#6975,#6977,#1159,.T.);
#9054=EDGE_CURVE('',#6978,#6979,#4940,.T.);
#9055=EDGE_CURVE('',#6978,#6976,#1160,.T.);
#9056=EDGE_CURVE('',#6977,#6979,#1161,.T.);
#9057=EDGE_CURVE('',#6980,#6981,#4941,.T.);
#9058=EDGE_CURVE('',#6980,#6978,#1162,.T.);
#9059=EDGE_CURVE('',#6979,#6981,#1163,.T.);
#9060=EDGE_CURVE('',#6982,#6983,#4942,.T.);
#9061=EDGE_CURVE('',#6982,#6980,#1164,.T.);
#9062=EDGE_CURVE('',#6981,#6983,#1165,.T.);
#9063=EDGE_CURVE('',#6984,#6985,#4943,.T.);
#9064=EDGE_CURVE('',#6984,#6982,#1166,.T.);
#9065=EDGE_CURVE('',#6983,#6985,#1167,.T.);
#9066=EDGE_CURVE('',#6986,#6987,#4944,.T.);
#9067=EDGE_CURVE('',#6986,#6984,#1168,.T.);
#9068=EDGE_CURVE('',#6985,#6987,#1169,.T.);
#9069=EDGE_CURVE('',#6988,#6989,#4945,.T.);
#9070=EDGE_CURVE('',#6988,#6986,#1170,.T.);
#9071=EDGE_CURVE('',#6987,#6989,#1171,.T.);
#9072=EDGE_CURVE('',#6990,#6991,#4946,.T.);
#9073=EDGE_CURVE('',#6990,#6988,#1172,.T.);
#9074=EDGE_CURVE('',#6989,#6991,#1173,.T.);
#9075=EDGE_CURVE('',#6992,#6993,#4947,.T.);
#9076=EDGE_CURVE('',#6992,#6990,#1174,.T.);
#9077=EDGE_CURVE('',#6991,#6993,#1175,.T.);
#9078=EDGE_CURVE('',#6994,#6995,#4948,.T.);
#9079=EDGE_CURVE('',#6994,#6992,#1176,.T.);
#9080=EDGE_CURVE('',#6993,#6995,#1177,.T.);
#9081=EDGE_CURVE('',#6996,#6997,#4949,.T.);
#9082=EDGE_CURVE('',#6996,#6994,#1178,.T.);
#9083=EDGE_CURVE('',#6995,#6997,#1179,.T.);
#9084=EDGE_CURVE('',#6998,#6999,#4950,.T.);
#9085=EDGE_CURVE('',#6998,#6996,#1180,.T.);
#9086=EDGE_CURVE('',#6997,#6999,#1181,.T.);
#9087=EDGE_CURVE('',#7000,#7001,#4951,.T.);
#9088=EDGE_CURVE('',#7000,#6998,#1182,.T.);
#9089=EDGE_CURVE('',#6999,#7001,#1183,.T.);
#9090=EDGE_CURVE('',#7002,#7003,#4952,.T.);
#9091=EDGE_CURVE('',#7002,#7000,#1184,.T.);
#9092=EDGE_CURVE('',#7001,#7003,#1185,.T.);
#9093=EDGE_CURVE('',#7004,#7005,#4953,.T.);
#9094=EDGE_CURVE('',#7004,#7002,#1186,.T.);
#9095=EDGE_CURVE('',#7003,#7005,#1187,.T.);
#9096=EDGE_CURVE('',#7006,#7007,#4954,.T.);
#9097=EDGE_CURVE('',#7006,#7004,#1188,.T.);
#9098=EDGE_CURVE('',#7005,#7007,#1189,.T.);
#9099=EDGE_CURVE('',#7008,#7009,#4955,.T.);
#9100=EDGE_CURVE('',#7008,#7006,#1190,.T.);
#9101=EDGE_CURVE('',#7007,#7009,#1191,.T.);
#9102=EDGE_CURVE('',#7010,#7011,#4956,.T.);
#9103=EDGE_CURVE('',#7010,#7008,#1192,.T.);
#9104=EDGE_CURVE('',#7009,#7011,#1193,.T.);
#9105=EDGE_CURVE('',#7012,#7013,#4957,.T.);
#9106=EDGE_CURVE('',#7012,#7010,#1194,.T.);
#9107=EDGE_CURVE('',#7011,#7013,#1195,.T.);
#9108=EDGE_CURVE('',#7014,#7014,#2512,.T.);
#9109=EDGE_CURVE('',#7014,#7015,#4958,.T.);
#9110=EDGE_CURVE('',#7015,#7016,#2513,.T.);
#9111=EDGE_CURVE('',#7016,#7017,#1196,.T.);
#9112=EDGE_CURVE('',#7017,#7018,#4959,.T.);
#9113=EDGE_CURVE('',#7018,#7019,#1197,.T.);
#9114=EDGE_CURVE('',#7019,#7015,#2514,.T.);
#9115=EDGE_CURVE('',#7020,#7021,#4960,.T.);
#9116=EDGE_CURVE('',#7020,#7022,#1198,.T.);
#9117=EDGE_CURVE('',#7023,#7022,#2515,.T.);
#9118=EDGE_CURVE('',#7021,#7023,#1199,.T.);
#9119=EDGE_CURVE('',#7024,#7025,#4961,.T.);
#9120=EDGE_CURVE('',#7024,#7020,#1200,.T.);
#9121=EDGE_CURVE('',#7025,#7021,#1201,.T.);
#9122=EDGE_CURVE('',#7026,#7027,#4962,.T.);
#9123=EDGE_CURVE('',#7026,#7024,#1202,.T.);
#9124=EDGE_CURVE('',#7027,#7025,#1203,.T.);
#9125=EDGE_CURVE('',#7028,#7029,#4963,.T.);
#9126=EDGE_CURVE('',#7028,#7026,#1204,.T.);
#9127=EDGE_CURVE('',#7029,#7027,#1205,.T.);
#9128=EDGE_CURVE('',#7030,#7031,#4964,.T.);
#9129=EDGE_CURVE('',#7030,#7028,#1206,.T.);
#9130=EDGE_CURVE('',#7031,#7029,#1207,.T.);
#9131=EDGE_CURVE('',#7032,#7033,#4965,.T.);
#9132=EDGE_CURVE('',#7032,#7030,#1208,.T.);
#9133=EDGE_CURVE('',#7033,#7031,#1209,.T.);
#9134=EDGE_CURVE('',#7034,#7035,#4966,.T.);
#9135=EDGE_CURVE('',#7034,#7032,#1210,.T.);
#9136=EDGE_CURVE('',#7035,#7033,#1211,.T.);
#9137=EDGE_CURVE('',#7036,#7037,#4967,.T.);
#9138=EDGE_CURVE('',#7036,#7034,#1212,.T.);
#9139=EDGE_CURVE('',#7037,#7035,#1213,.T.);
#9140=EDGE_CURVE('',#7038,#7039,#4968,.T.);
#9141=EDGE_CURVE('',#7038,#7036,#1214,.T.);
#9142=EDGE_CURVE('',#7039,#7037,#1215,.T.);
#9143=EDGE_CURVE('',#7040,#7041,#4969,.T.);
#9144=EDGE_CURVE('',#7040,#7038,#1216,.T.);
#9145=EDGE_CURVE('',#7041,#7039,#1217,.T.);
#9146=EDGE_CURVE('',#7042,#7043,#4970,.T.);
#9147=EDGE_CURVE('',#7042,#7040,#1218,.T.);
#9148=EDGE_CURVE('',#7043,#7041,#1219,.T.);
#9149=EDGE_CURVE('',#7044,#7045,#4971,.T.);
#9150=EDGE_CURVE('',#7044,#7042,#1220,.T.);
#9151=EDGE_CURVE('',#7045,#7043,#1221,.T.);
#9152=EDGE_CURVE('',#7046,#7047,#4972,.T.);
#9153=EDGE_CURVE('',#7046,#7044,#1222,.T.);
#9154=EDGE_CURVE('',#7047,#7045,#1223,.T.);
#9155=EDGE_CURVE('',#7048,#7049,#4973,.T.);
#9156=EDGE_CURVE('',#7048,#7046,#1224,.T.);
#9157=EDGE_CURVE('',#7049,#7047,#1225,.T.);
#9158=EDGE_CURVE('',#7050,#7051,#4974,.T.);
#9159=EDGE_CURVE('',#7050,#7048,#1226,.T.);
#9160=EDGE_CURVE('',#7051,#7049,#1227,.T.);
#9161=EDGE_CURVE('',#7052,#7053,#4975,.T.);
#9162=EDGE_CURVE('',#7052,#7050,#1228,.T.);
#9163=EDGE_CURVE('',#7053,#7051,#1229,.T.);
#9164=EDGE_CURVE('',#7054,#7055,#4976,.T.);
#9165=EDGE_CURVE('',#7054,#7052,#1230,.T.);
#9166=EDGE_CURVE('',#7055,#7053,#1231,.T.);
#9167=EDGE_CURVE('',#7056,#7057,#4977,.T.);
#9168=EDGE_CURVE('',#7056,#7054,#1232,.T.);
#9169=EDGE_CURVE('',#7057,#7055,#1233,.T.);
#9170=EDGE_CURVE('',#7058,#7059,#4978,.T.);
#9171=EDGE_CURVE('',#7058,#7056,#1234,.T.);
#9172=EDGE_CURVE('',#7059,#7057,#1235,.T.);
#9173=EDGE_CURVE('',#7060,#7061,#4979,.T.);
#9174=EDGE_CURVE('',#7060,#7058,#1236,.T.);
#9175=EDGE_CURVE('',#7061,#7059,#1237,.T.);
#9176=EDGE_CURVE('',#7062,#7063,#4980,.T.);
#9177=EDGE_CURVE('',#7062,#7060,#1238,.T.);
#9178=EDGE_CURVE('',#7063,#7061,#1239,.T.);
#9179=EDGE_CURVE('',#7064,#7065,#4981,.T.);
#9180=EDGE_CURVE('',#7064,#7062,#1240,.T.);
#9181=EDGE_CURVE('',#7065,#7063,#1241,.T.);
#9182=EDGE_CURVE('',#7066,#7067,#4982,.T.);
#9183=EDGE_CURVE('',#7066,#7064,#1242,.T.);
#9184=EDGE_CURVE('',#7067,#7065,#1243,.T.);
#9185=EDGE_CURVE('',#7068,#7069,#4983,.T.);
#9186=EDGE_CURVE('',#7068,#7066,#1244,.T.);
#9187=EDGE_CURVE('',#7069,#7067,#1245,.T.);
#9188=EDGE_CURVE('',#7070,#7071,#4984,.T.);
#9189=EDGE_CURVE('',#7070,#7068,#1246,.T.);
#9190=EDGE_CURVE('',#7071,#7069,#1247,.T.);
#9191=EDGE_CURVE('',#7072,#7073,#4985,.T.);
#9192=EDGE_CURVE('',#7072,#7070,#1248,.T.);
#9193=EDGE_CURVE('',#7073,#7071,#1249,.T.);
#9194=EDGE_CURVE('',#7074,#7075,#4986,.T.);
#9195=EDGE_CURVE('',#7074,#7072,#1250,.T.);
#9196=EDGE_CURVE('',#7075,#7073,#1251,.T.);
#9197=EDGE_CURVE('',#7076,#7077,#4987,.T.);
#9198=EDGE_CURVE('',#7076,#7074,#1252,.T.);
#9199=EDGE_CURVE('',#7077,#7075,#1253,.T.);
#9200=EDGE_CURVE('',#7078,#7079,#4988,.T.);
#9201=EDGE_CURVE('',#7078,#7076,#1254,.T.);
#9202=EDGE_CURVE('',#7079,#7077,#1255,.T.);
#9203=EDGE_CURVE('',#7080,#7081,#4989,.T.);
#9204=EDGE_CURVE('',#7080,#7078,#1256,.T.);
#9205=EDGE_CURVE('',#7081,#7079,#1257,.T.);
#9206=EDGE_CURVE('',#7082,#7083,#4990,.T.);
#9207=EDGE_CURVE('',#7082,#7080,#1258,.T.);
#9208=EDGE_CURVE('',#7083,#7081,#1259,.T.);
#9209=EDGE_CURVE('',#7084,#7085,#4991,.T.);
#9210=EDGE_CURVE('',#7084,#7082,#1260,.T.);
#9211=EDGE_CURVE('',#7085,#7083,#1261,.T.);
#9212=EDGE_CURVE('',#7086,#7087,#4992,.T.);
#9213=EDGE_CURVE('',#7086,#7084,#1262,.T.);
#9214=EDGE_CURVE('',#7087,#7085,#1263,.T.);
#9215=EDGE_CURVE('',#7088,#7089,#4993,.T.);
#9216=EDGE_CURVE('',#7088,#7086,#1264,.T.);
#9217=EDGE_CURVE('',#7089,#7087,#1265,.T.);
#9218=EDGE_CURVE('',#7090,#7091,#4994,.T.);
#9219=EDGE_CURVE('',#7090,#7088,#1266,.T.);
#9220=EDGE_CURVE('',#7091,#7089,#1267,.T.);
#9221=EDGE_CURVE('',#7092,#7093,#4995,.T.);
#9222=EDGE_CURVE('',#7092,#7090,#1268,.T.);
#9223=EDGE_CURVE('',#7093,#7091,#1269,.T.);
#9224=EDGE_CURVE('',#7094,#7095,#4996,.T.);
#9225=EDGE_CURVE('',#7094,#7092,#1270,.T.);
#9226=EDGE_CURVE('',#7095,#7093,#1271,.T.);
#9227=EDGE_CURVE('',#7096,#7097,#4997,.T.);
#9228=EDGE_CURVE('',#7096,#7094,#1272,.T.);
#9229=EDGE_CURVE('',#7097,#7095,#1273,.T.);
#9230=EDGE_CURVE('',#7098,#7099,#4998,.T.);
#9231=EDGE_CURVE('',#7098,#7096,#1274,.T.);
#9232=EDGE_CURVE('',#7099,#7097,#1275,.T.);
#9233=EDGE_CURVE('',#7100,#7101,#4999,.T.);
#9234=EDGE_CURVE('',#7100,#7098,#1276,.T.);
#9235=EDGE_CURVE('',#7101,#7099,#1277,.T.);
#9236=EDGE_CURVE('',#7102,#7103,#5000,.T.);
#9237=EDGE_CURVE('',#7102,#7100,#1278,.T.);
#9238=EDGE_CURVE('',#7103,#7101,#1279,.T.);
#9239=EDGE_CURVE('',#7104,#7105,#5001,.T.);
#9240=EDGE_CURVE('',#7104,#7102,#1280,.T.);
#9241=EDGE_CURVE('',#7105,#7103,#1281,.T.);
#9242=EDGE_CURVE('',#7106,#7107,#5002,.T.);
#9243=EDGE_CURVE('',#7106,#7104,#1282,.T.);
#9244=EDGE_CURVE('',#7107,#7105,#1283,.T.);
#9245=EDGE_CURVE('',#7108,#7109,#5003,.T.);
#9246=EDGE_CURVE('',#7108,#7106,#1284,.T.);
#9247=EDGE_CURVE('',#7109,#7107,#1285,.T.);
#9248=EDGE_CURVE('',#7110,#7111,#5004,.T.);
#9249=EDGE_CURVE('',#7110,#7108,#1286,.T.);
#9250=EDGE_CURVE('',#7111,#7109,#1287,.T.);
#9251=EDGE_CURVE('',#7112,#7113,#5005,.T.);
#9252=EDGE_CURVE('',#7112,#7110,#1288,.T.);
#9253=EDGE_CURVE('',#7113,#7111,#1289,.T.);
#9254=EDGE_CURVE('',#7114,#7115,#5006,.T.);
#9255=EDGE_CURVE('',#7114,#7112,#1290,.T.);
#9256=EDGE_CURVE('',#7115,#7113,#1291,.T.);
#9257=EDGE_CURVE('',#7116,#7117,#5007,.T.);
#9258=EDGE_CURVE('',#7116,#7114,#1292,.T.);
#9259=EDGE_CURVE('',#7117,#7115,#1293,.T.);
#9260=EDGE_CURVE('',#7118,#7119,#5008,.T.);
#9261=EDGE_CURVE('',#7118,#7116,#1294,.T.);
#9262=EDGE_CURVE('',#7119,#7117,#1295,.T.);
#9263=EDGE_CURVE('',#7120,#7121,#5009,.T.);
#9264=EDGE_CURVE('',#7120,#7118,#1296,.T.);
#9265=EDGE_CURVE('',#7121,#7119,#1297,.T.);
#9266=EDGE_CURVE('',#7122,#7123,#5010,.T.);
#9267=EDGE_CURVE('',#7122,#7120,#1298,.T.);
#9268=EDGE_CURVE('',#7123,#7121,#1299,.T.);
#9269=EDGE_CURVE('',#7124,#7125,#5011,.T.);
#9270=EDGE_CURVE('',#7124,#7122,#1300,.T.);
#9271=EDGE_CURVE('',#7125,#7123,#1301,.T.);
#9272=EDGE_CURVE('',#7126,#7127,#5012,.T.);
#9273=EDGE_CURVE('',#7126,#7124,#1302,.T.);
#9274=EDGE_CURVE('',#7127,#7125,#1303,.T.);
#9275=EDGE_CURVE('',#7128,#7129,#5013,.T.);
#9276=EDGE_CURVE('',#7128,#7126,#1304,.T.);
#9277=EDGE_CURVE('',#7129,#7127,#1305,.T.);
#9278=EDGE_CURVE('',#7130,#7131,#5014,.T.);
#9279=EDGE_CURVE('',#7130,#7128,#1306,.T.);
#9280=EDGE_CURVE('',#7131,#7129,#1307,.T.);
#9281=EDGE_CURVE('',#7132,#7133,#5015,.T.);
#9282=EDGE_CURVE('',#7132,#7130,#1308,.T.);
#9283=EDGE_CURVE('',#7133,#7131,#1309,.T.);
#9284=EDGE_CURVE('',#7134,#7135,#5016,.T.);
#9285=EDGE_CURVE('',#7134,#7132,#1310,.T.);
#9286=EDGE_CURVE('',#7135,#7133,#1311,.T.);
#9287=EDGE_CURVE('',#7136,#7137,#5017,.T.);
#9288=EDGE_CURVE('',#7136,#7134,#1312,.T.);
#9289=EDGE_CURVE('',#7137,#7135,#1313,.T.);
#9290=EDGE_CURVE('',#7138,#7139,#5018,.T.);
#9291=EDGE_CURVE('',#7138,#7136,#1314,.T.);
#9292=EDGE_CURVE('',#7139,#7137,#1315,.T.);
#9293=EDGE_CURVE('',#7140,#7141,#5019,.T.);
#9294=EDGE_CURVE('',#7140,#7138,#1316,.T.);
#9295=EDGE_CURVE('',#7141,#7139,#1317,.T.);
#9296=EDGE_CURVE('',#7142,#7143,#5020,.T.);
#9297=EDGE_CURVE('',#7142,#7140,#1318,.T.);
#9298=EDGE_CURVE('',#7143,#7141,#1319,.T.);
#9299=EDGE_CURVE('',#7144,#7145,#5021,.T.);
#9300=EDGE_CURVE('',#7144,#7142,#1320,.T.);
#9301=EDGE_CURVE('',#7145,#7143,#1321,.T.);
#9302=EDGE_CURVE('',#7146,#7147,#5022,.T.);
#9303=EDGE_CURVE('',#7146,#7144,#1322,.T.);
#9304=EDGE_CURVE('',#7147,#7145,#1323,.T.);
#9305=EDGE_CURVE('',#7148,#7149,#5023,.T.);
#9306=EDGE_CURVE('',#7148,#7146,#1324,.T.);
#9307=EDGE_CURVE('',#7149,#7147,#1325,.T.);
#9308=EDGE_CURVE('',#7150,#7151,#5024,.T.);
#9309=EDGE_CURVE('',#7150,#7148,#1326,.T.);
#9310=EDGE_CURVE('',#7151,#7149,#1327,.T.);
#9311=EDGE_CURVE('',#7152,#7153,#5025,.T.);
#9312=EDGE_CURVE('',#7152,#7150,#1328,.T.);
#9313=EDGE_CURVE('',#7153,#7151,#1329,.T.);
#9314=EDGE_CURVE('',#7154,#7155,#5026,.T.);
#9315=EDGE_CURVE('',#7154,#7152,#1330,.T.);
#9316=EDGE_CURVE('',#7155,#7153,#1331,.T.);
#9317=EDGE_CURVE('',#7156,#7157,#5027,.T.);
#9318=EDGE_CURVE('',#7156,#7154,#1332,.T.);
#9319=EDGE_CURVE('',#7157,#7155,#1333,.T.);
#9320=EDGE_CURVE('',#7158,#7159,#5028,.T.);
#9321=EDGE_CURVE('',#7158,#7156,#1334,.T.);
#9322=EDGE_CURVE('',#7159,#7157,#1335,.T.);
#9323=EDGE_CURVE('',#7160,#7161,#5029,.T.);
#9324=EDGE_CURVE('',#7160,#7158,#1336,.T.);
#9325=EDGE_CURVE('',#7161,#7159,#1337,.T.);
#9326=EDGE_CURVE('',#7162,#7163,#5030,.T.);
#9327=EDGE_CURVE('',#7162,#7160,#1338,.T.);
#9328=EDGE_CURVE('',#7163,#7161,#1339,.T.);
#9329=EDGE_CURVE('',#7164,#7165,#5031,.T.);
#9330=EDGE_CURVE('',#7164,#7162,#1340,.T.);
#9331=EDGE_CURVE('',#7165,#7163,#1341,.T.);
#9332=EDGE_CURVE('',#7166,#7167,#5032,.T.);
#9333=EDGE_CURVE('',#7166,#7164,#1342,.T.);
#9334=EDGE_CURVE('',#7167,#7165,#1343,.T.);
#9335=EDGE_CURVE('',#7168,#7169,#5033,.T.);
#9336=EDGE_CURVE('',#7168,#7166,#1344,.T.);
#9337=EDGE_CURVE('',#7169,#7167,#1345,.T.);
#9338=EDGE_CURVE('',#7170,#7171,#5034,.T.);
#9339=EDGE_CURVE('',#7170,#7168,#1346,.T.);
#9340=EDGE_CURVE('',#7171,#7169,#1347,.T.);
#9341=EDGE_CURVE('',#7172,#7173,#5035,.T.);
#9342=EDGE_CURVE('',#7172,#7170,#1348,.T.);
#9343=EDGE_CURVE('',#7173,#7171,#1349,.T.);
#9344=EDGE_CURVE('',#7174,#7175,#5036,.T.);
#9345=EDGE_CURVE('',#7174,#7172,#1350,.T.);
#9346=EDGE_CURVE('',#7175,#7173,#1351,.T.);
#9347=EDGE_CURVE('',#7176,#7177,#5037,.T.);
#9348=EDGE_CURVE('',#7176,#7174,#1352,.T.);
#9349=EDGE_CURVE('',#7177,#7175,#1353,.T.);
#9350=EDGE_CURVE('',#7178,#7179,#5038,.T.);
#9351=EDGE_CURVE('',#7178,#7176,#1354,.T.);
#9352=EDGE_CURVE('',#7179,#7177,#1355,.T.);
#9353=EDGE_CURVE('',#7180,#7181,#5039,.T.);
#9354=EDGE_CURVE('',#7180,#7178,#1356,.T.);
#9355=EDGE_CURVE('',#7181,#7179,#1357,.T.);
#9356=EDGE_CURVE('',#6859,#7182,#1358,.T.);
#9357=EDGE_CURVE('',#7183,#6858,#1359,.T.);
#9358=EDGE_CURVE('',#7182,#7183,#2516,.T.);
#9359=EDGE_CURVE('',#7183,#7184,#1360,.T.);
#9360=EDGE_CURVE('',#7184,#7185,#2517,.T.);
#9361=EDGE_CURVE('',#7185,#7182,#1361,.T.);
#9362=EDGE_CURVE('',#7186,#7186,#2518,.T.);
#9363=EDGE_CURVE('',#7186,#7187,#5040,.T.);
#9364=EDGE_CURVE('',#7187,#7187,#2519,.T.);
#9365=EDGE_CURVE('',#7188,#7188,#2520,.T.);
#9366=EDGE_CURVE('',#7189,#7189,#2521,.T.);
#9367=EDGE_CURVE('',#7189,#7188,#5041,.T.);
#9368=EDGE_CURVE('',#7022,#7016,#1362,.T.);
#9369=EDGE_CURVE('',#7019,#7023,#1363,.T.);
#9370=EDGE_CURVE('',#7185,#7181,#1364,.T.);
#9371=EDGE_CURVE('',#7013,#7018,#1365,.T.);
#9372=EDGE_CURVE('',#7184,#7180,#1366,.T.);
#9373=EDGE_CURVE('',#7017,#7012,#1367,.T.);
#9374=EDGE_CURVE('',#7190,#7190,#2522,.T.);
#9375=EDGE_CURVE('',#7190,#7191,#5042,.T.);
#9376=EDGE_CURVE('',#7191,#7191,#2523,.T.);
#9377=EDGE_CURVE('',#7192,#7192,#2524,.T.);
#9378=EDGE_CURVE('',#7192,#7193,#5043,.T.);
#9379=EDGE_CURVE('',#7193,#7193,#2525,.T.);
#9380=EDGE_CURVE('',#7194,#7194,#2526,.T.);
#9381=EDGE_CURVE('',#7194,#7195,#5044,.T.);
#9382=EDGE_CURVE('',#7195,#7195,#2527,.T.);
#9383=EDGE_CURVE('',#7196,#7196,#2528,.T.);
#9384=EDGE_CURVE('',#7196,#7197,#5045,.T.);
#9385=EDGE_CURVE('',#7197,#7197,#2529,.T.);
#9386=EDGE_CURVE('',#7198,#7198,#2530,.T.);
#9387=EDGE_CURVE('',#7198,#7199,#5046,.T.);
#9388=EDGE_CURVE('',#7199,#7199,#2531,.T.);
#9389=EDGE_CURVE('',#7200,#7200,#2532,.T.);
#9390=EDGE_CURVE('',#7200,#7201,#5047,.T.);
#9391=EDGE_CURVE('',#7201,#7201,#2533,.T.);
#9392=EDGE_CURVE('',#7202,#7202,#2534,.T.);
#9393=EDGE_CURVE('',#7203,#7203,#2535,.T.);
#9394=EDGE_CURVE('',#7204,#7204,#2536,.T.);
#9395=EDGE_CURVE('',#7204,#7202,#5048,.T.);
#9396=EDGE_CURVE('',#7205,#7205,#2537,.T.);
#9397=EDGE_CURVE('',#7203,#7205,#5049,.T.);
#9398=EDGE_CURVE('',#7206,#7206,#2538,.T.);
#9399=EDGE_CURVE('',#7206,#7207,#5050,.T.);
#9400=EDGE_CURVE('',#7207,#7207,#2539,.T.);
#9401=EDGE_CURVE('',#7208,#7208,#2540,.T.);
#9402=EDGE_CURVE('',#7208,#7209,#5051,.T.);
#9403=EDGE_CURVE('',#7209,#7209,#2541,.T.);
#9404=EDGE_CURVE('',#7210,#7211,#5052,.T.);
#9405=EDGE_CURVE('',#7212,#7210,#5053,.T.);
#9406=EDGE_CURVE('',#7213,#7212,#5054,.T.);
#9407=EDGE_CURVE('',#7211,#7213,#5055,.T.);
#9408=EDGE_CURVE('',#7214,#7215,#5056,.T.);
#9409=EDGE_CURVE('',#7216,#7214,#5057,.T.);
#9410=EDGE_CURVE('',#7217,#7216,#5058,.T.);
#9411=EDGE_CURVE('',#7215,#7217,#5059,.T.);
#9412=EDGE_CURVE('',#7212,#7217,#2542,.T.);
#9413=EDGE_CURVE('',#7215,#7210,#2543,.T.);
#9414=EDGE_CURVE('',#7214,#7211,#2544,.T.);
#9415=EDGE_CURVE('',#7213,#7216,#2545,.T.);
#9416=EDGE_CURVE('',#7218,#7219,#5060,.T.);
#9417=EDGE_CURVE('',#7218,#7220,#1368,.T.);
#9418=EDGE_CURVE('',#7220,#7221,#2546,.F.);
#9419=EDGE_CURVE('',#7221,#7219,#1369,.T.);
#9420=EDGE_CURVE('',#7222,#7223,#5061,.T.);
#9421=EDGE_CURVE('',#7222,#7218,#1370,.T.);
#9422=EDGE_CURVE('',#7219,#7223,#1371,.T.);
#9423=EDGE_CURVE('',#7224,#7225,#5062,.T.);
#9424=EDGE_CURVE('',#7224,#7222,#1372,.T.);
#9425=EDGE_CURVE('',#7223,#7225,#1373,.T.);
#9426=EDGE_CURVE('',#7226,#7227,#5063,.T.);
#9427=EDGE_CURVE('',#7226,#7224,#1374,.T.);
#9428=EDGE_CURVE('',#7225,#7227,#1375,.T.);
#9429=EDGE_CURVE('',#7228,#7229,#5064,.T.);
#9430=EDGE_CURVE('',#7228,#7226,#1376,.T.);
#9431=EDGE_CURVE('',#7227,#7229,#1377,.T.);
#9432=EDGE_CURVE('',#7230,#7231,#5065,.T.);
#9433=EDGE_CURVE('',#7230,#7228,#1378,.T.);
#9434=EDGE_CURVE('',#7229,#7231,#1379,.T.);
#9435=EDGE_CURVE('',#7232,#7233,#5066,.T.);
#9436=EDGE_CURVE('',#7232,#7230,#1380,.T.);
#9437=EDGE_CURVE('',#7231,#7233,#1381,.T.);
#9438=EDGE_CURVE('',#7234,#7235,#5067,.T.);
#9439=EDGE_CURVE('',#7234,#7232,#1382,.T.);
#9440=EDGE_CURVE('',#7233,#7235,#1383,.T.);
#9441=EDGE_CURVE('',#7236,#7237,#5068,.T.);
#9442=EDGE_CURVE('',#7236,#7234,#1384,.T.);
#9443=EDGE_CURVE('',#7235,#7237,#1385,.T.);
#9444=EDGE_CURVE('',#7238,#7239,#5069,.T.);
#9445=EDGE_CURVE('',#7238,#7236,#1386,.T.);
#9446=EDGE_CURVE('',#7237,#7239,#1387,.T.);
#9447=EDGE_CURVE('',#7240,#7241,#5070,.T.);
#9448=EDGE_CURVE('',#7240,#7238,#1388,.T.);
#9449=EDGE_CURVE('',#7239,#7241,#1389,.T.);
#9450=EDGE_CURVE('',#7242,#7243,#5071,.T.);
#9451=EDGE_CURVE('',#7242,#7240,#1390,.T.);
#9452=EDGE_CURVE('',#7241,#7243,#1391,.T.);
#9453=EDGE_CURVE('',#7244,#7245,#5072,.T.);
#9454=EDGE_CURVE('',#7244,#7242,#1392,.T.);
#9455=EDGE_CURVE('',#7243,#7245,#1393,.T.);
#9456=EDGE_CURVE('',#7246,#7247,#5073,.T.);
#9457=EDGE_CURVE('',#7246,#7244,#1394,.T.);
#9458=EDGE_CURVE('',#7245,#7247,#1395,.T.);
#9459=EDGE_CURVE('',#7248,#7249,#5074,.T.);
#9460=EDGE_CURVE('',#7248,#7246,#1396,.T.);
#9461=EDGE_CURVE('',#7247,#7249,#1397,.T.);
#9462=EDGE_CURVE('',#7250,#7251,#5075,.T.);
#9463=EDGE_CURVE('',#7250,#7248,#1398,.T.);
#9464=EDGE_CURVE('',#7249,#7251,#1399,.T.);
#9465=EDGE_CURVE('',#7252,#7253,#5076,.T.);
#9466=EDGE_CURVE('',#7252,#7250,#1400,.T.);
#9467=EDGE_CURVE('',#7251,#7253,#1401,.T.);
#9468=EDGE_CURVE('',#7254,#7255,#5077,.T.);
#9469=EDGE_CURVE('',#7254,#7252,#1402,.T.);
#9470=EDGE_CURVE('',#7253,#7255,#1403,.T.);
#9471=EDGE_CURVE('',#7256,#7257,#5078,.T.);
#9472=EDGE_CURVE('',#7256,#7258,#1404,.T.);
#9473=EDGE_CURVE('',#7259,#7258,#2547,.T.);
#9474=EDGE_CURVE('',#7257,#7259,#1405,.T.);
#9475=EDGE_CURVE('',#7260,#7261,#5079,.T.);
#9476=EDGE_CURVE('',#7260,#7256,#1406,.T.);
#9477=EDGE_CURVE('',#7261,#7257,#1407,.T.);
#9478=EDGE_CURVE('',#7262,#7263,#5080,.T.);
#9479=EDGE_CURVE('',#7262,#7260,#1408,.T.);
#9480=EDGE_CURVE('',#7263,#7261,#1409,.T.);
#9481=EDGE_CURVE('',#7264,#7265,#5081,.T.);
#9482=EDGE_CURVE('',#7264,#7262,#1410,.T.);
#9483=EDGE_CURVE('',#7265,#7263,#1411,.T.);
#9484=EDGE_CURVE('',#7266,#7267,#5082,.T.);
#9485=EDGE_CURVE('',#7266,#7264,#1412,.T.);
#9486=EDGE_CURVE('',#7267,#7265,#1413,.T.);
#9487=EDGE_CURVE('',#7268,#7269,#5083,.T.);
#9488=EDGE_CURVE('',#7268,#7266,#1414,.T.);
#9489=EDGE_CURVE('',#7269,#7267,#1415,.T.);
#9490=EDGE_CURVE('',#7270,#7271,#5084,.T.);
#9491=EDGE_CURVE('',#7270,#7268,#1416,.T.);
#9492=EDGE_CURVE('',#7271,#7269,#1417,.T.);
#9493=EDGE_CURVE('',#7272,#7273,#5085,.T.);
#9494=EDGE_CURVE('',#7272,#7270,#1418,.T.);
#9495=EDGE_CURVE('',#7273,#7271,#1419,.T.);
#9496=EDGE_CURVE('',#7274,#7275,#5086,.T.);
#9497=EDGE_CURVE('',#7274,#7272,#1420,.T.);
#9498=EDGE_CURVE('',#7275,#7273,#1421,.T.);
#9499=EDGE_CURVE('',#7276,#7277,#5087,.T.);
#9500=EDGE_CURVE('',#7276,#7274,#1422,.T.);
#9501=EDGE_CURVE('',#7277,#7275,#1423,.T.);
#9502=EDGE_CURVE('',#7278,#7279,#5088,.T.);
#9503=EDGE_CURVE('',#7278,#7276,#1424,.T.);
#9504=EDGE_CURVE('',#7279,#7277,#1425,.T.);
#9505=EDGE_CURVE('',#7280,#7281,#5089,.T.);
#9506=EDGE_CURVE('',#7280,#7278,#1426,.T.);
#9507=EDGE_CURVE('',#7281,#7279,#1427,.T.);
#9508=EDGE_CURVE('',#7282,#7283,#5090,.T.);
#9509=EDGE_CURVE('',#7282,#7280,#1428,.T.);
#9510=EDGE_CURVE('',#7283,#7281,#1429,.T.);
#9511=EDGE_CURVE('',#7284,#7285,#5091,.T.);
#9512=EDGE_CURVE('',#7284,#7282,#1430,.T.);
#9513=EDGE_CURVE('',#7285,#7283,#1431,.T.);
#9514=EDGE_CURVE('',#7286,#7287,#5092,.T.);
#9515=EDGE_CURVE('',#7286,#7284,#1432,.T.);
#9516=EDGE_CURVE('',#7287,#7285,#1433,.T.);
#9517=EDGE_CURVE('',#7288,#7289,#5093,.T.);
#9518=EDGE_CURVE('',#7288,#7286,#1434,.T.);
#9519=EDGE_CURVE('',#7289,#7287,#1435,.T.);
#9520=EDGE_CURVE('',#7290,#7291,#5094,.T.);
#9521=EDGE_CURVE('',#7290,#7288,#1436,.T.);
#9522=EDGE_CURVE('',#7291,#7289,#1437,.T.);
#9523=EDGE_CURVE('',#7292,#7293,#5095,.T.);
#9524=EDGE_CURVE('',#7292,#7290,#1438,.T.);
#9525=EDGE_CURVE('',#7293,#7291,#1439,.T.);
#9526=EDGE_CURVE('',#7294,#7295,#5096,.T.);
#9527=EDGE_CURVE('',#7294,#7296,#5097,.T.);
#9528=EDGE_CURVE('',#7296,#7297,#5098,.T.);
#9529=EDGE_CURVE('',#7295,#7297,#5099,.T.);
#9530=EDGE_CURVE('',#7298,#7294,#5100,.T.);
#9531=EDGE_CURVE('',#7298,#7299,#5101,.T.);
#9532=EDGE_CURVE('',#7299,#7296,#5102,.T.);
#9533=EDGE_CURVE('',#7300,#7298,#5103,.T.);
#9534=EDGE_CURVE('',#7300,#7301,#5104,.T.);
#9535=EDGE_CURVE('',#7301,#7299,#5105,.T.);
#9536=EDGE_CURVE('',#7302,#7300,#5106,.T.);
#9537=EDGE_CURVE('',#7302,#7303,#5107,.T.);
#9538=EDGE_CURVE('',#7303,#7301,#5108,.T.);
#9539=EDGE_CURVE('',#7304,#7302,#5109,.T.);
#9540=EDGE_CURVE('',#7304,#7305,#5110,.T.);
#9541=EDGE_CURVE('',#7305,#7303,#5111,.T.);
#9542=EDGE_CURVE('',#7295,#7304,#5112,.T.);
#9543=EDGE_CURVE('',#7297,#7305,#5113,.T.);
#9544=EDGE_CURVE('',#7306,#7259,#1440,.T.);
#9545=EDGE_CURVE('',#7255,#7306,#1441,.T.);
#9546=EDGE_CURVE('',#7307,#7221,#1442,.T.);
#9547=EDGE_CURVE('',#7307,#7293,#1443,.T.);
#9548=EDGE_CURVE('',#7308,#7307,#2548,.T.);
#9549=EDGE_CURVE('',#7308,#7292,#1444,.T.);
#9550=EDGE_CURVE('',#7258,#7309,#1445,.T.);
#9551=EDGE_CURVE('',#7220,#7308,#1446,.T.);
#9552=EDGE_CURVE('',#7309,#7254,#1447,.T.);
#9553=EDGE_CURVE('',#7309,#7306,#2549,.F.);
#9554=EDGE_CURVE('',#7310,#7310,#2550,.T.);
#9555=EDGE_CURVE('',#7311,#7311,#2551,.T.);
#9556=EDGE_CURVE('',#7312,#7312,#2552,.T.);
#9557=EDGE_CURVE('',#7312,#7310,#5114,.T.);
#9558=EDGE_CURVE('',#7311,#7313,#5115,.T.);
#9559=EDGE_CURVE('',#7313,#7313,#2553,.T.);
#9560=EDGE_CURVE('',#7314,#7314,#2554,.T.);
#9561=EDGE_CURVE('',#7315,#7315,#2555,.T.);
#9562=EDGE_CURVE('',#7316,#7316,#2556,.T.);
#9563=EDGE_CURVE('',#7316,#7314,#5116,.T.);
#9564=EDGE_CURVE('',#7315,#7317,#5117,.T.);
#9565=EDGE_CURVE('',#7317,#7317,#2557,.T.);
#9566=EDGE_CURVE('',#7318,#7318,#2558,.T.);
#9567=EDGE_CURVE('',#7319,#7319,#2559,.T.);
#9568=EDGE_CURVE('',#7320,#7320,#2560,.T.);
#9569=EDGE_CURVE('',#7320,#7318,#5118,.T.);
#9570=EDGE_CURVE('',#7319,#7321,#5119,.T.);
#9571=EDGE_CURVE('',#7321,#7321,#2561,.T.);
#9572=EDGE_CURVE('',#7322,#7322,#2562,.T.);
#9573=EDGE_CURVE('',#7323,#7323,#2563,.T.);
#9574=EDGE_CURVE('',#7324,#7324,#2564,.T.);
#9575=EDGE_CURVE('',#7324,#7322,#5120,.T.);
#9576=EDGE_CURVE('',#7323,#7325,#5121,.T.);
#9577=EDGE_CURVE('',#7325,#7325,#2565,.T.);
#9578=EDGE_CURVE('',#7326,#7326,#2566,.T.);
#9579=EDGE_CURVE('',#7326,#7327,#5122,.T.);
#9580=EDGE_CURVE('',#7327,#7327,#2567,.T.);
#9581=EDGE_CURVE('',#7328,#7328,#2568,.T.);
#9582=EDGE_CURVE('',#7328,#7329,#5123,.T.);
#9583=EDGE_CURVE('',#7329,#7329,#2569,.T.);
#9584=EDGE_CURVE('',#7330,#7330,#2570,.T.);
#9585=EDGE_CURVE('',#7330,#7331,#2571,.T.);
#9586=EDGE_CURVE('',#7331,#7331,#2572,.T.);
#9587=EDGE_CURVE('',#7331,#7332,#5124,.T.);
#9588=EDGE_CURVE('',#7332,#7332,#2573,.T.);
#9589=EDGE_CURVE('',#7333,#7333,#2574,.T.);
#9590=EDGE_CURVE('',#7333,#7334,#5125,.T.);
#9591=EDGE_CURVE('',#7334,#7334,#2575,.T.);
#9592=EDGE_CURVE('',#7335,#7335,#2576,.T.);
#9593=EDGE_CURVE('',#7335,#7330,#5126,.T.);
#9594=EDGE_CURVE('',#7336,#7336,#2577,.T.);
#9595=EDGE_CURVE('',#7336,#7337,#2578,.T.);
#9596=EDGE_CURVE('',#7337,#7337,#2579,.T.);
#9597=EDGE_CURVE('',#7338,#7338,#2580,.T.);
#9598=EDGE_CURVE('',#7338,#7337,#5127,.T.);
#9599=EDGE_CURVE('',#7336,#7339,#5128,.T.);
#9600=EDGE_CURVE('',#7339,#7339,#2581,.T.);
#9601=EDGE_CURVE('',#7340,#7340,#2582,.T.);
#9602=EDGE_CURVE('',#7340,#7341,#5129,.T.);
#9603=EDGE_CURVE('',#7341,#7341,#2583,.T.);
#9604=EDGE_CURVE('',#7342,#7343,#2584,.T.);
#9605=EDGE_CURVE('',#7344,#7345,#1448,.T.);
#9606=EDGE_CURVE('',#7346,#7344,#2585,.T.);
#9607=EDGE_CURVE('',#7347,#7346,#1449,.T.);
#9608=EDGE_CURVE('',#7347,#7348,#2586,.T.);
#9609=EDGE_CURVE('',#7349,#7347,#1450,.T.);
#9610=EDGE_CURVE('',#7345,#7349,#2587,.T.);
#9611=EDGE_CURVE('',#7350,#7350,#2588,.T.);
#9612=EDGE_CURVE('',#7350,#7351,#5130,.T.);
#9613=EDGE_CURVE('',#7351,#7352,#1451,.T.);
#9614=EDGE_CURVE('',#7352,#7353,#2589,.T.);
#9615=EDGE_CURVE('',#7353,#7354,#1452,.T.);
#9616=EDGE_CURVE('',#7354,#7355,#2590,.T.);
#9617=EDGE_CURVE('',#7355,#7356,#1453,.T.);
#9618=EDGE_CURVE('',#7356,#7357,#2591,.T.);
#9619=EDGE_CURVE('',#7357,#7358,#1454,.T.);
#9620=EDGE_CURVE('',#7358,#7359,#2592,.T.);
#9621=EDGE_CURVE('',#7359,#7360,#1455,.T.);
#9622=EDGE_CURVE('',#7360,#7361,#1456,.T.);
#9623=EDGE_CURVE('',#7361,#7362,#2593,.T.);
#9624=EDGE_CURVE('',#7362,#7363,#1457,.T.);
#9625=EDGE_CURVE('',#7363,#7364,#1458,.T.);
#9626=EDGE_CURVE('',#7364,#7365,#2594,.T.);
#9627=EDGE_CURVE('',#7365,#7366,#1459,.T.);
#9628=EDGE_CURVE('',#7366,#7367,#1460,.T.);
#9629=EDGE_CURVE('',#7367,#7349,#2595,.T.);
#9630=EDGE_CURVE('',#7346,#7368,#2596,.T.);
#9631=EDGE_CURVE('',#7368,#7369,#1461,.T.);
#9632=EDGE_CURVE('',#7369,#7370,#1462,.T.);
#9633=EDGE_CURVE('',#7370,#7371,#2597,.T.);
#9634=EDGE_CURVE('',#7371,#7372,#1463,.T.);
#9635=EDGE_CURVE('',#7372,#7373,#2598,.T.);
#9636=EDGE_CURVE('',#7373,#7374,#1464,.T.);
#9637=EDGE_CURVE('',#7374,#7375,#2599,.T.);
#9638=EDGE_CURVE('',#7375,#7376,#1465,.T.);
#9639=EDGE_CURVE('',#7376,#7377,#2600,.T.);
#9640=EDGE_CURVE('',#7377,#7351,#1466,.T.);
#9641=EDGE_CURVE('',#7378,#7344,#2601,.T.);
#9642=EDGE_CURVE('',#7378,#7368,#2602,.T.);
#9643=EDGE_CURVE('',#7379,#7378,#1467,.T.);
#9644=EDGE_CURVE('',#7370,#7379,#2603,.T.);
#9645=EDGE_CURVE('',#7369,#7380,#2604,.T.);
#9646=EDGE_CURVE('',#7381,#7379,#2605,.T.);
#9647=EDGE_CURVE('',#7381,#7371,#2606,.T.);
#9648=EDGE_CURVE('',#7382,#7381,#1468,.T.);
#9649=EDGE_CURVE('',#7383,#7382,#2607,.T.);
#9650=EDGE_CURVE('',#7383,#7384,#2608,.T.);
#9651=EDGE_CURVE('',#7372,#7383,#2609,.T.);
#9652=EDGE_CURVE('',#7385,#7382,#2610,.T.);
#9653=EDGE_CURVE('',#7385,#7373,#2611,.T.);
#9654=EDGE_CURVE('',#7386,#7387,#1469,.T.);
#9655=EDGE_CURVE('',#7374,#7386,#2612,.T.);
#9656=EDGE_CURVE('',#7387,#7385,#1470,.T.);
#9657=EDGE_CURVE('',#7387,#7388,#2613,.T.);
#9658=EDGE_CURVE('',#7389,#7386,#2614,.T.);
#9659=EDGE_CURVE('',#7389,#7375,#2615,.T.);
#9660=EDGE_CURVE('',#7390,#7391,#1471,.T.);
#9661=EDGE_CURVE('',#7376,#7390,#2616,.T.);
#9662=EDGE_CURVE('',#7391,#7389,#1472,.T.);
#9663=EDGE_CURVE('',#7391,#7392,#2617,.T.);
#9664=EDGE_CURVE('',#7393,#7390,#2618,.T.);
#9665=EDGE_CURVE('',#7393,#7377,#2619,.T.);
#9666=EDGE_CURVE('',#7394,#7395,#1473,.T.);
#9667=EDGE_CURVE('',#7352,#7394,#2620,.T.);
#9668=EDGE_CURVE('',#7395,#7393,#1474,.T.);
#9669=EDGE_CURVE('',#7395,#7396,#2621,.T.);
#9670=EDGE_CURVE('',#7397,#7394,#2622,.T.);
#9671=EDGE_CURVE('',#7397,#7353,#2623,.T.);
#9672=EDGE_CURVE('',#7398,#7399,#1475,.T.);
#9673=EDGE_CURVE('',#7354,#7398,#2624,.T.);
#9674=EDGE_CURVE('',#7399,#7397,#1476,.T.);
#9675=EDGE_CURVE('',#7399,#7400,#2625,.T.);
#9676=EDGE_CURVE('',#7401,#7398,#2626,.T.);
#9677=EDGE_CURVE('',#7401,#7355,#2627,.T.);
#9678=EDGE_CURVE('',#7402,#7403,#1477,.T.);
#9679=EDGE_CURVE('',#7356,#7402,#2628,.T.);
#9680=EDGE_CURVE('',#7403,#7401,#1478,.T.);
#9681=EDGE_CURVE('',#7403,#7404,#2629,.T.);
#9682=EDGE_CURVE('',#7405,#7402,#2630,.T.);
#9683=EDGE_CURVE('',#7405,#7406,#2631,.T.);
#9684=EDGE_CURVE('',#7406,#7357,#2632,.T.);
#9685=EDGE_CURVE('',#7407,#7405,#1479,.T.);
#9686=EDGE_CURVE('',#7358,#7407,#2633,.T.);
#9687=EDGE_CURVE('',#7406,#7408,#2634,.T.);
#9688=EDGE_CURVE('',#7409,#7407,#2635,.T.);
#9689=EDGE_CURVE('',#7409,#7359,#2636,.T.);
#9690=EDGE_CURVE('',#7410,#7409,#1480,.T.);
#9691=EDGE_CURVE('',#7361,#7410,#2637,.T.);
#9692=EDGE_CURVE('',#7360,#7411,#2638,.T.);
#9693=EDGE_CURVE('',#7412,#7410,#2639,.T.);
#9694=EDGE_CURVE('',#7412,#7362,#2640,.T.);
#9695=EDGE_CURVE('',#7413,#7412,#1481,.T.);
#9696=EDGE_CURVE('',#7364,#7413,#2641,.T.);
#9697=EDGE_CURVE('',#7363,#7414,#2642,.T.);
#9698=EDGE_CURVE('',#7415,#7413,#2643,.T.);
#9699=EDGE_CURVE('',#7415,#7365,#2644,.T.);
#9700=EDGE_CURVE('',#7416,#7415,#1482,.T.);
#9701=EDGE_CURVE('',#7367,#7416,#2645,.T.);
#9702=EDGE_CURVE('',#7366,#7417,#2646,.T.);
#9703=EDGE_CURVE('',#7418,#7418,#2647,.T.);
#9704=EDGE_CURVE('',#7418,#7395,#5131,.T.);
#9705=EDGE_CURVE('',#7345,#7416,#2648,.T.);
#9706=EDGE_CURVE('',#7419,#7419,#2649,.T.);
#9707=EDGE_CURVE('',#7419,#7420,#5132,.T.);
#9708=EDGE_CURVE('',#7420,#7420,#2650,.T.);
#9709=EDGE_CURVE('',#7421,#7421,#2651,.T.);
#9710=EDGE_CURVE('',#7421,#7422,#5133,.T.);
#9711=EDGE_CURVE('',#7422,#7422,#2652,.T.);
#9712=EDGE_CURVE('',#7423,#7424,#5134,.T.);
#9713=EDGE_CURVE('',#7423,#7425,#1483,.T.);
#9714=EDGE_CURVE('',#7425,#7426,#2653,.F.);
#9715=EDGE_CURVE('',#7426,#7424,#1484,.T.);
#9716=EDGE_CURVE('',#7427,#7428,#5135,.T.);
#9717=EDGE_CURVE('',#7427,#7423,#1485,.T.);
#9718=EDGE_CURVE('',#7424,#7428,#1486,.T.);
#9719=EDGE_CURVE('',#7429,#7430,#5136,.T.);
#9720=EDGE_CURVE('',#7429,#7427,#1487,.T.);
#9721=EDGE_CURVE('',#7428,#7430,#1488,.T.);
#9722=EDGE_CURVE('',#7431,#7432,#5137,.T.);
#9723=EDGE_CURVE('',#7431,#7429,#1489,.T.);
#9724=EDGE_CURVE('',#7430,#7432,#1490,.T.);
#9725=EDGE_CURVE('',#7433,#7434,#5138,.T.);
#9726=EDGE_CURVE('',#7433,#7431,#1491,.T.);
#9727=EDGE_CURVE('',#7432,#7434,#1492,.T.);
#9728=EDGE_CURVE('',#7435,#7436,#5139,.T.);
#9729=EDGE_CURVE('',#7435,#7433,#1493,.T.);
#9730=EDGE_CURVE('',#7434,#7436,#1494,.T.);
#9731=EDGE_CURVE('',#7437,#7438,#5140,.T.);
#9732=EDGE_CURVE('',#7437,#7435,#1495,.T.);
#9733=EDGE_CURVE('',#7436,#7438,#1496,.T.);
#9734=EDGE_CURVE('',#7439,#7440,#5141,.T.);
#9735=EDGE_CURVE('',#7439,#7437,#1497,.T.);
#9736=EDGE_CURVE('',#7438,#7440,#1498,.T.);
#9737=EDGE_CURVE('',#7441,#7442,#5142,.T.);
#9738=EDGE_CURVE('',#7441,#7439,#1499,.T.);
#9739=EDGE_CURVE('',#7440,#7442,#1500,.T.);
#9740=EDGE_CURVE('',#7443,#7444,#5143,.T.);
#9741=EDGE_CURVE('',#7443,#7441,#1501,.T.);
#9742=EDGE_CURVE('',#7442,#7444,#1502,.T.);
#9743=EDGE_CURVE('',#7445,#7446,#5144,.T.);
#9744=EDGE_CURVE('',#7445,#7443,#1503,.T.);
#9745=EDGE_CURVE('',#7444,#7446,#1504,.T.);
#9746=EDGE_CURVE('',#7447,#7448,#5145,.T.);
#9747=EDGE_CURVE('',#7447,#7445,#1505,.T.);
#9748=EDGE_CURVE('',#7446,#7448,#1506,.T.);
#9749=EDGE_CURVE('',#7449,#7450,#5146,.T.);
#9750=EDGE_CURVE('',#7449,#7447,#1507,.T.);
#9751=EDGE_CURVE('',#7448,#7450,#1508,.T.);
#9752=EDGE_CURVE('',#7451,#7452,#5147,.T.);
#9753=EDGE_CURVE('',#7451,#7449,#1509,.T.);
#9754=EDGE_CURVE('',#7450,#7452,#1510,.T.);
#9755=EDGE_CURVE('',#7453,#7454,#5148,.T.);
#9756=EDGE_CURVE('',#7453,#7451,#1511,.T.);
#9757=EDGE_CURVE('',#7452,#7454,#1512,.T.);
#9758=EDGE_CURVE('',#7455,#7456,#5149,.T.);
#9759=EDGE_CURVE('',#7455,#7453,#1513,.T.);
#9760=EDGE_CURVE('',#7454,#7456,#1514,.T.);
#9761=EDGE_CURVE('',#7457,#7458,#5150,.T.);
#9762=EDGE_CURVE('',#7457,#7459,#1515,.T.);
#9763=EDGE_CURVE('',#7459,#7460,#2654,.T.);
#9764=EDGE_CURVE('',#7458,#7460,#1516,.T.);
#9765=EDGE_CURVE('',#7461,#7462,#5151,.T.);
#9766=EDGE_CURVE('',#7461,#7457,#1517,.T.);
#9767=EDGE_CURVE('',#7462,#7458,#1518,.T.);
#9768=EDGE_CURVE('',#7463,#7464,#5152,.T.);
#9769=EDGE_CURVE('',#7463,#7461,#1519,.T.);
#9770=EDGE_CURVE('',#7464,#7462,#1520,.T.);
#9771=EDGE_CURVE('',#7465,#7466,#5153,.T.);
#9772=EDGE_CURVE('',#7465,#7463,#1521,.T.);
#9773=EDGE_CURVE('',#7466,#7464,#1522,.T.);
#9774=EDGE_CURVE('',#7467,#7468,#5154,.T.);
#9775=EDGE_CURVE('',#7467,#7465,#1523,.T.);
#9776=EDGE_CURVE('',#7468,#7466,#1524,.T.);
#9777=EDGE_CURVE('',#7469,#7470,#5155,.T.);
#9778=EDGE_CURVE('',#7469,#7467,#1525,.T.);
#9779=EDGE_CURVE('',#7470,#7468,#1526,.T.);
#9780=EDGE_CURVE('',#7471,#7472,#5156,.T.);
#9781=EDGE_CURVE('',#7471,#7469,#1527,.T.);
#9782=EDGE_CURVE('',#7472,#7470,#1528,.T.);
#9783=EDGE_CURVE('',#7473,#7474,#5157,.T.);
#9784=EDGE_CURVE('',#7473,#7471,#1529,.T.);
#9785=EDGE_CURVE('',#7474,#7472,#1530,.T.);
#9786=EDGE_CURVE('',#7475,#7476,#5158,.T.);
#9787=EDGE_CURVE('',#7475,#7473,#1531,.T.);
#9788=EDGE_CURVE('',#7476,#7474,#1532,.T.);
#9789=EDGE_CURVE('',#7477,#7478,#5159,.T.);
#9790=EDGE_CURVE('',#7477,#7475,#1533,.T.);
#9791=EDGE_CURVE('',#7478,#7476,#1534,.T.);
#9792=EDGE_CURVE('',#7479,#7480,#5160,.T.);
#9793=EDGE_CURVE('',#7479,#7477,#1535,.T.);
#9794=EDGE_CURVE('',#7480,#7478,#1536,.T.);
#9795=EDGE_CURVE('',#7481,#7482,#5161,.T.);
#9796=EDGE_CURVE('',#7481,#7479,#1537,.T.);
#9797=EDGE_CURVE('',#7482,#7480,#1538,.T.);
#9798=EDGE_CURVE('',#7483,#7484,#5162,.T.);
#9799=EDGE_CURVE('',#7483,#7481,#1539,.T.);
#9800=EDGE_CURVE('',#7484,#7482,#1540,.T.);
#9801=EDGE_CURVE('',#7485,#7486,#5163,.T.);
#9802=EDGE_CURVE('',#7485,#7483,#1541,.T.);
#9803=EDGE_CURVE('',#7486,#7484,#1542,.T.);
#9804=EDGE_CURVE('',#7487,#7488,#5164,.T.);
#9805=EDGE_CURVE('',#7487,#7485,#1543,.T.);
#9806=EDGE_CURVE('',#7488,#7486,#1544,.T.);
#9807=EDGE_CURVE('',#7489,#7490,#5165,.T.);
#9808=EDGE_CURVE('',#7489,#7487,#1545,.T.);
#9809=EDGE_CURVE('',#7490,#7488,#1546,.T.);
#9810=EDGE_CURVE('',#7460,#7491,#1547,.T.);
#9811=EDGE_CURVE('',#7492,#7459,#1548,.T.);
#9812=EDGE_CURVE('',#7493,#7492,#2655,.T.);
#9813=EDGE_CURVE('',#7491,#7493,#1549,.T.);
#9814=EDGE_CURVE('',#7491,#7494,#5166,.T.);
#9815=EDGE_CURVE('',#7494,#7494,#2656,.T.);
#9816=EDGE_CURVE('',#7495,#7489,#1550,.T.);
#9817=EDGE_CURVE('',#7425,#7495,#1551,.T.);
#9818=EDGE_CURVE('',#7492,#7455,#1552,.T.);
#9819=EDGE_CURVE('',#7496,#7490,#1553,.T.);
#9820=EDGE_CURVE('',#7495,#7496,#2657,.T.);
#9821=EDGE_CURVE('',#7456,#7493,#1554,.T.);
#9822=EDGE_CURVE('',#7496,#7426,#1555,.T.);
#9823=EDGE_CURVE('',#7497,#7498,#5167,.T.);
#9824=EDGE_CURVE('',#7497,#7499,#5168,.T.);
#9825=EDGE_CURVE('',#7499,#7500,#5169,.T.);
#9826=EDGE_CURVE('',#7498,#7500,#5170,.T.);
#9827=EDGE_CURVE('',#7501,#7497,#5171,.T.);
#9828=EDGE_CURVE('',#7501,#7502,#5172,.T.);
#9829=EDGE_CURVE('',#7502,#7499,#5173,.T.);
#9830=EDGE_CURVE('',#7503,#7501,#5174,.T.);
#9831=EDGE_CURVE('',#7503,#7504,#5175,.T.);
#9832=EDGE_CURVE('',#7504,#7502,#5176,.T.);
#9833=EDGE_CURVE('',#7505,#7503,#5177,.T.);
#9834=EDGE_CURVE('',#7505,#7506,#5178,.T.);
#9835=EDGE_CURVE('',#7506,#7504,#5179,.T.);
#9836=EDGE_CURVE('',#7507,#7505,#5180,.T.);
#9837=EDGE_CURVE('',#7507,#7508,#5181,.T.);
#9838=EDGE_CURVE('',#7508,#7506,#5182,.T.);
#9839=EDGE_CURVE('',#7498,#7507,#5183,.T.);
#9840=EDGE_CURVE('',#7500,#7508,#5184,.T.);
#9841=EDGE_CURVE('',#7509,#7509,#2658,.T.);
#9842=EDGE_CURVE('',#7509,#7510,#5185,.T.);
#9843=EDGE_CURVE('',#7510,#7510,#2659,.T.);
#9844=ORIENTED_EDGE('',*,*,#7511,.F.);
#9845=ORIENTED_EDGE('',*,*,#7512,.T.);
#9846=ORIENTED_EDGE('',*,*,#7513,.F.);
#9847=ORIENTED_EDGE('',*,*,#7514,.T.);
#9848=ORIENTED_EDGE('',*,*,#7515,.F.);
#9849=ORIENTED_EDGE('',*,*,#7514,.F.);
#9850=ORIENTED_EDGE('',*,*,#7516,.F.);
#9851=ORIENTED_EDGE('',*,*,#7517,.F.);
#9852=ORIENTED_EDGE('',*,*,#7518,.F.);
#9853=ORIENTED_EDGE('',*,*,#7519,.F.);
#9854=ORIENTED_EDGE('',*,*,#7517,.T.);
#9855=ORIENTED_EDGE('',*,*,#7520,.T.);
#9856=ORIENTED_EDGE('',*,*,#7521,.T.);
#9857=ORIENTED_EDGE('',*,*,#7516,.T.);
#9858=ORIENTED_EDGE('',*,*,#7513,.T.);
#9859=ORIENTED_EDGE('',*,*,#7522,.T.);
#9860=ORIENTED_EDGE('',*,*,#7520,.F.);
#9861=ORIENTED_EDGE('',*,*,#7523,.F.);
#9862=ORIENTED_EDGE('',*,*,#7521,.F.);
#9863=ORIENTED_EDGE('',*,*,#7522,.F.);
#9864=ORIENTED_EDGE('',*,*,#7512,.F.);
#9865=ORIENTED_EDGE('',*,*,#7524,.F.);
#9866=ORIENTED_EDGE('',*,*,#7525,.F.);
#9867=ORIENTED_EDGE('',*,*,#7526,.F.);
#9868=ORIENTED_EDGE('',*,*,#7527,.F.);
#9869=ORIENTED_EDGE('',*,*,#7528,.T.);
#9870=ORIENTED_EDGE('',*,*,#7529,.F.);
#9871=ORIENTED_EDGE('',*,*,#7526,.T.);
#9872=ORIENTED_EDGE('',*,*,#7527,.T.);
#9873=ORIENTED_EDGE('',*,*,#7525,.T.);
#9874=ORIENTED_EDGE('',*,*,#7529,.T.);
#9875=ORIENTED_EDGE('',*,*,#7530,.T.);
#9876=ORIENTED_EDGE('',*,*,#7531,.T.);
#9877=ORIENTED_EDGE('',*,*,#7532,.F.);
#9878=ORIENTED_EDGE('',*,*,#7533,.T.);
#9879=ORIENTED_EDGE('',*,*,#7534,.T.);
#9880=ORIENTED_EDGE('',*,*,#7533,.F.);
#9881=ORIENTED_EDGE('',*,*,#7535,.F.);
#9882=ORIENTED_EDGE('',*,*,#7536,.T.);
#9883=ORIENTED_EDGE('',*,*,#7537,.T.);
#9884=ORIENTED_EDGE('',*,*,#7538,.F.);
#9885=ORIENTED_EDGE('',*,*,#7539,.T.);
#9886=ORIENTED_EDGE('',*,*,#7540,.F.);
#9887=ORIENTED_EDGE('',*,*,#7539,.F.);
#9888=ORIENTED_EDGE('',*,*,#7541,.F.);
#9889=ORIENTED_EDGE('',*,*,#7542,.T.);
#9890=ORIENTED_EDGE('',*,*,#7543,.F.);
#9891=ORIENTED_EDGE('',*,*,#7542,.F.);
#9892=ORIENTED_EDGE('',*,*,#7544,.F.);
#9893=ORIENTED_EDGE('',*,*,#7545,.T.);
#9894=ORIENTED_EDGE('',*,*,#7546,.F.);
#9895=ORIENTED_EDGE('',*,*,#7545,.F.);
#9896=ORIENTED_EDGE('',*,*,#7547,.F.);
#9897=ORIENTED_EDGE('',*,*,#7548,.T.);
#9898=ORIENTED_EDGE('',*,*,#7549,.F.);
#9899=ORIENTED_EDGE('',*,*,#7548,.F.);
#9900=ORIENTED_EDGE('',*,*,#7550,.F.);
#9901=ORIENTED_EDGE('',*,*,#7551,.T.);
#9902=ORIENTED_EDGE('',*,*,#7552,.F.);
#9903=ORIENTED_EDGE('',*,*,#7551,.F.);
#9904=ORIENTED_EDGE('',*,*,#7553,.F.);
#9905=ORIENTED_EDGE('',*,*,#7554,.T.);
#9906=ORIENTED_EDGE('',*,*,#7555,.F.);
#9907=ORIENTED_EDGE('',*,*,#7554,.F.);
#9908=ORIENTED_EDGE('',*,*,#7536,.F.);
#9909=ORIENTED_EDGE('',*,*,#7556,.F.);
#9910=ORIENTED_EDGE('',*,*,#7557,.F.);
#9911=ORIENTED_EDGE('',*,*,#7558,.T.);
#9912=ORIENTED_EDGE('',*,*,#7559,.T.);
#9913=ORIENTED_EDGE('',*,*,#7557,.T.);
#9914=ORIENTED_EDGE('',*,*,#7560,.F.);
#9915=ORIENTED_EDGE('',*,*,#7561,.F.);
#9916=ORIENTED_EDGE('',*,*,#7531,.F.);
#9917=ORIENTED_EDGE('',*,*,#7562,.T.);
#9918=ORIENTED_EDGE('',*,*,#7561,.T.);
#9919=ORIENTED_EDGE('',*,*,#7563,.F.);
#9920=ORIENTED_EDGE('',*,*,#7537,.F.);
#9921=ORIENTED_EDGE('',*,*,#7558,.F.);
#9922=ORIENTED_EDGE('',*,*,#7559,.F.);
#9923=ORIENTED_EDGE('',*,*,#7562,.F.);
#9924=ORIENTED_EDGE('',*,*,#7530,.F.);
#9925=ORIENTED_EDGE('',*,*,#7528,.F.);
#9926=ORIENTED_EDGE('',*,*,#7540,.T.);
#9927=ORIENTED_EDGE('',*,*,#7564,.T.);
#9928=ORIENTED_EDGE('',*,*,#7541,.T.);
#9929=ORIENTED_EDGE('',*,*,#7534,.F.);
#9930=ORIENTED_EDGE('',*,*,#7553,.T.);
#9931=ORIENTED_EDGE('',*,*,#7550,.T.);
#9932=ORIENTED_EDGE('',*,*,#7547,.T.);
#9933=ORIENTED_EDGE('',*,*,#7544,.T.);
#9934=ORIENTED_EDGE('',*,*,#7565,.F.);
#9935=ORIENTED_EDGE('',*,*,#7543,.T.);
#9936=ORIENTED_EDGE('',*,*,#7566,.F.);
#9937=ORIENTED_EDGE('',*,*,#7555,.T.);
#9938=ORIENTED_EDGE('',*,*,#7552,.T.);
#9939=ORIENTED_EDGE('',*,*,#7549,.T.);
#9940=ORIENTED_EDGE('',*,*,#7546,.T.);
#9941=ORIENTED_EDGE('',*,*,#7564,.F.);
#9942=ORIENTED_EDGE('',*,*,#7567,.T.);
#9943=ORIENTED_EDGE('',*,*,#7565,.T.);
#9944=ORIENTED_EDGE('',*,*,#7567,.F.);
#9945=ORIENTED_EDGE('',*,*,#7566,.T.);
#9946=ORIENTED_EDGE('',*,*,#7568,.T.);
#9947=ORIENTED_EDGE('',*,*,#7569,.T.);
#9948=ORIENTED_EDGE('',*,*,#7568,.F.);
#9949=ORIENTED_EDGE('',*,*,#7570,.F.);
#9950=ORIENTED_EDGE('',*,*,#7571,.T.);
#9951=ORIENTED_EDGE('',*,*,#7518,.T.);
#9952=ORIENTED_EDGE('',*,*,#7519,.T.);
#9953=ORIENTED_EDGE('',*,*,#7523,.T.);
#9954=ORIENTED_EDGE('',*,*,#7572,.T.);
#9955=ORIENTED_EDGE('',*,*,#7573,.T.);
#9956=ORIENTED_EDGE('',*,*,#7572,.F.);
#9957=ORIENTED_EDGE('',*,*,#7524,.T.);
#9958=ORIENTED_EDGE('',*,*,#7511,.T.);
#9959=ORIENTED_EDGE('',*,*,#7515,.T.);
#9960=ORIENTED_EDGE('',*,*,#7571,.F.);
#9961=ORIENTED_EDGE('',*,*,#7535,.T.);
#9962=ORIENTED_EDGE('',*,*,#7532,.T.);
#9963=ORIENTED_EDGE('',*,*,#7563,.T.);
#9964=ORIENTED_EDGE('',*,*,#7560,.T.);
#9965=ORIENTED_EDGE('',*,*,#7556,.T.);
#9966=ORIENTED_EDGE('',*,*,#7538,.T.);
#9967=ORIENTED_EDGE('',*,*,#7570,.T.);
#9968=ORIENTED_EDGE('',*,*,#7569,.F.);
#9969=ORIENTED_EDGE('',*,*,#7573,.F.);
#9970=ORIENTED_EDGE('',*,*,#7574,.T.);
#9971=ORIENTED_EDGE('',*,*,#7575,.F.);
#9972=ORIENTED_EDGE('',*,*,#7576,.T.);
#9973=ORIENTED_EDGE('',*,*,#7577,.T.);
#9974=ORIENTED_EDGE('',*,*,#7578,.T.);
#9975=ORIENTED_EDGE('',*,*,#7579,.F.);
#9976=ORIENTED_EDGE('',*,*,#7574,.F.);
#9977=ORIENTED_EDGE('',*,*,#7580,.T.);
#9978=ORIENTED_EDGE('',*,*,#7581,.T.);
#9979=ORIENTED_EDGE('',*,*,#7582,.T.);
#9980=ORIENTED_EDGE('',*,*,#7577,.F.);
#9981=ORIENTED_EDGE('',*,*,#7583,.T.);
#9982=ORIENTED_EDGE('',*,*,#7584,.T.);
#9983=ORIENTED_EDGE('',*,*,#7585,.T.);
#9984=ORIENTED_EDGE('',*,*,#7581,.F.);
#9985=ORIENTED_EDGE('',*,*,#7586,.T.);
#9986=ORIENTED_EDGE('',*,*,#7587,.T.);
#9987=ORIENTED_EDGE('',*,*,#7588,.T.);
#9988=ORIENTED_EDGE('',*,*,#7584,.F.);
#9989=ORIENTED_EDGE('',*,*,#7589,.T.);
#9990=ORIENTED_EDGE('',*,*,#7590,.T.);
#9991=ORIENTED_EDGE('',*,*,#7591,.T.);
#9992=ORIENTED_EDGE('',*,*,#7587,.F.);
#9993=ORIENTED_EDGE('',*,*,#7592,.T.);
#9994=ORIENTED_EDGE('',*,*,#7593,.F.);
#9995=ORIENTED_EDGE('',*,*,#7594,.T.);
#9996=ORIENTED_EDGE('',*,*,#7595,.F.);
#9997=ORIENTED_EDGE('',*,*,#7596,.T.);
#9998=ORIENTED_EDGE('',*,*,#7597,.T.);
#9999=ORIENTED_EDGE('',*,*,#7598,.T.);
#10000=ORIENTED_EDGE('',*,*,#7599,.F.);
#10001=ORIENTED_EDGE('',*,*,#7600,.F.);
#10002=ORIENTED_EDGE('',*,*,#7601,.T.);
#10003=ORIENTED_EDGE('',*,*,#7602,.T.);
#10004=ORIENTED_EDGE('',*,*,#7597,.F.);
#10005=ORIENTED_EDGE('',*,*,#7603,.F.);
#10006=ORIENTED_EDGE('',*,*,#7604,.T.);
#10007=ORIENTED_EDGE('',*,*,#7605,.T.);
#10008=ORIENTED_EDGE('',*,*,#7601,.F.);
#10009=ORIENTED_EDGE('',*,*,#7606,.F.);
#10010=ORIENTED_EDGE('',*,*,#7607,.T.);
#10011=ORIENTED_EDGE('',*,*,#7608,.T.);
#10012=ORIENTED_EDGE('',*,*,#7604,.F.);
#10013=ORIENTED_EDGE('',*,*,#7609,.F.);
#10014=ORIENTED_EDGE('',*,*,#7610,.T.);
#10015=ORIENTED_EDGE('',*,*,#7611,.T.);
#10016=ORIENTED_EDGE('',*,*,#7607,.F.);
#10017=ORIENTED_EDGE('',*,*,#7612,.F.);
#10018=ORIENTED_EDGE('',*,*,#7613,.T.);
#10019=ORIENTED_EDGE('',*,*,#7614,.T.);
#10020=ORIENTED_EDGE('',*,*,#7610,.F.);
#10021=ORIENTED_EDGE('',*,*,#7615,.F.);
#10022=ORIENTED_EDGE('',*,*,#7616,.F.);
#10023=ORIENTED_EDGE('',*,*,#7617,.F.);
#10024=ORIENTED_EDGE('',*,*,#7618,.F.);
#10025=ORIENTED_EDGE('',*,*,#7619,.T.);
#10026=ORIENTED_EDGE('',*,*,#7620,.T.);
#10027=ORIENTED_EDGE('',*,*,#7621,.T.);
#10028=ORIENTED_EDGE('',*,*,#7622,.T.);
#10029=ORIENTED_EDGE('',*,*,#7623,.T.);
#10030=ORIENTED_EDGE('',*,*,#7624,.T.);
#10031=ORIENTED_EDGE('',*,*,#7623,.F.);
#10032=ORIENTED_EDGE('',*,*,#7625,.T.);
#10033=ORIENTED_EDGE('',*,*,#7626,.T.);
#10034=ORIENTED_EDGE('',*,*,#7627,.T.);
#10035=ORIENTED_EDGE('',*,*,#7628,.T.);
#10036=ORIENTED_EDGE('',*,*,#7620,.F.);
#10037=ORIENTED_EDGE('',*,*,#7629,.T.);
#10038=ORIENTED_EDGE('',*,*,#7630,.T.);
#10039=ORIENTED_EDGE('',*,*,#7631,.T.);
#10040=ORIENTED_EDGE('',*,*,#7627,.F.);
#10041=ORIENTED_EDGE('',*,*,#7632,.T.);
#10042=ORIENTED_EDGE('',*,*,#7633,.T.);
#10043=ORIENTED_EDGE('',*,*,#7634,.T.);
#10044=ORIENTED_EDGE('',*,*,#7630,.F.);
#10045=ORIENTED_EDGE('',*,*,#7635,.T.);
#10046=ORIENTED_EDGE('',*,*,#7636,.T.);
#10047=ORIENTED_EDGE('',*,*,#7637,.T.);
#10048=ORIENTED_EDGE('',*,*,#7633,.F.);
#10049=ORIENTED_EDGE('',*,*,#7638,.T.);
#10050=ORIENTED_EDGE('',*,*,#7639,.T.);
#10051=ORIENTED_EDGE('',*,*,#7640,.T.);
#10052=ORIENTED_EDGE('',*,*,#7636,.F.);
#10053=ORIENTED_EDGE('',*,*,#7641,.T.);
#10054=ORIENTED_EDGE('',*,*,#7642,.T.);
#10055=ORIENTED_EDGE('',*,*,#7643,.T.);
#10056=ORIENTED_EDGE('',*,*,#7639,.F.);
#10057=ORIENTED_EDGE('',*,*,#7644,.T.);
#10058=ORIENTED_EDGE('',*,*,#7645,.T.);
#10059=ORIENTED_EDGE('',*,*,#7646,.T.);
#10060=ORIENTED_EDGE('',*,*,#7642,.F.);
#10061=ORIENTED_EDGE('',*,*,#7647,.T.);
#10062=ORIENTED_EDGE('',*,*,#7648,.T.);
#10063=ORIENTED_EDGE('',*,*,#7649,.T.);
#10064=ORIENTED_EDGE('',*,*,#7645,.F.);
#10065=ORIENTED_EDGE('',*,*,#7650,.T.);
#10066=ORIENTED_EDGE('',*,*,#7651,.T.);
#10067=ORIENTED_EDGE('',*,*,#7652,.T.);
#10068=ORIENTED_EDGE('',*,*,#7648,.F.);
#10069=ORIENTED_EDGE('',*,*,#7653,.T.);
#10070=ORIENTED_EDGE('',*,*,#7654,.T.);
#10071=ORIENTED_EDGE('',*,*,#7655,.T.);
#10072=ORIENTED_EDGE('',*,*,#7651,.F.);
#10073=ORIENTED_EDGE('',*,*,#7656,.T.);
#10074=ORIENTED_EDGE('',*,*,#7657,.T.);
#10075=ORIENTED_EDGE('',*,*,#7658,.T.);
#10076=ORIENTED_EDGE('',*,*,#7654,.F.);
#10077=ORIENTED_EDGE('',*,*,#7659,.T.);
#10078=ORIENTED_EDGE('',*,*,#7660,.T.);
#10079=ORIENTED_EDGE('',*,*,#7661,.T.);
#10080=ORIENTED_EDGE('',*,*,#7657,.F.);
#10081=ORIENTED_EDGE('',*,*,#7662,.T.);
#10082=ORIENTED_EDGE('',*,*,#7663,.T.);
#10083=ORIENTED_EDGE('',*,*,#7664,.T.);
#10084=ORIENTED_EDGE('',*,*,#7660,.F.);
#10085=ORIENTED_EDGE('',*,*,#7665,.T.);
#10086=ORIENTED_EDGE('',*,*,#7666,.T.);
#10087=ORIENTED_EDGE('',*,*,#7667,.T.);
#10088=ORIENTED_EDGE('',*,*,#7663,.F.);
#10089=ORIENTED_EDGE('',*,*,#7668,.T.);
#10090=ORIENTED_EDGE('',*,*,#7669,.T.);
#10091=ORIENTED_EDGE('',*,*,#7670,.T.);
#10092=ORIENTED_EDGE('',*,*,#7666,.F.);
#10093=ORIENTED_EDGE('',*,*,#7671,.T.);
#10094=ORIENTED_EDGE('',*,*,#7672,.T.);
#10095=ORIENTED_EDGE('',*,*,#7673,.T.);
#10096=ORIENTED_EDGE('',*,*,#7669,.F.);
#10097=ORIENTED_EDGE('',*,*,#7674,.T.);
#10098=ORIENTED_EDGE('',*,*,#7675,.F.);
#10099=ORIENTED_EDGE('',*,*,#7676,.T.);
#10100=ORIENTED_EDGE('',*,*,#7677,.F.);
#10101=ORIENTED_EDGE('',*,*,#7678,.T.);
#10102=ORIENTED_EDGE('',*,*,#7679,.T.);
#10103=ORIENTED_EDGE('',*,*,#7680,.T.);
#10104=ORIENTED_EDGE('',*,*,#7681,.F.);
#10105=ORIENTED_EDGE('',*,*,#7682,.F.);
#10106=ORIENTED_EDGE('',*,*,#7683,.T.);
#10107=ORIENTED_EDGE('',*,*,#7684,.T.);
#10108=ORIENTED_EDGE('',*,*,#7679,.F.);
#10109=ORIENTED_EDGE('',*,*,#7685,.F.);
#10110=ORIENTED_EDGE('',*,*,#7686,.T.);
#10111=ORIENTED_EDGE('',*,*,#7687,.T.);
#10112=ORIENTED_EDGE('',*,*,#7683,.F.);
#10113=ORIENTED_EDGE('',*,*,#7688,.F.);
#10114=ORIENTED_EDGE('',*,*,#7689,.T.);
#10115=ORIENTED_EDGE('',*,*,#7690,.T.);
#10116=ORIENTED_EDGE('',*,*,#7686,.F.);
#10117=ORIENTED_EDGE('',*,*,#7691,.F.);
#10118=ORIENTED_EDGE('',*,*,#7692,.T.);
#10119=ORIENTED_EDGE('',*,*,#7693,.T.);
#10120=ORIENTED_EDGE('',*,*,#7689,.F.);
#10121=ORIENTED_EDGE('',*,*,#7694,.F.);
#10122=ORIENTED_EDGE('',*,*,#7695,.T.);
#10123=ORIENTED_EDGE('',*,*,#7696,.T.);
#10124=ORIENTED_EDGE('',*,*,#7692,.F.);
#10125=ORIENTED_EDGE('',*,*,#7697,.F.);
#10126=ORIENTED_EDGE('',*,*,#7698,.T.);
#10127=ORIENTED_EDGE('',*,*,#7699,.T.);
#10128=ORIENTED_EDGE('',*,*,#7695,.F.);
#10129=ORIENTED_EDGE('',*,*,#7700,.F.);
#10130=ORIENTED_EDGE('',*,*,#7701,.T.);
#10131=ORIENTED_EDGE('',*,*,#7702,.T.);
#10132=ORIENTED_EDGE('',*,*,#7698,.F.);
#10133=ORIENTED_EDGE('',*,*,#7703,.F.);
#10134=ORIENTED_EDGE('',*,*,#7704,.T.);
#10135=ORIENTED_EDGE('',*,*,#7705,.T.);
#10136=ORIENTED_EDGE('',*,*,#7701,.F.);
#10137=ORIENTED_EDGE('',*,*,#7706,.F.);
#10138=ORIENTED_EDGE('',*,*,#7707,.T.);
#10139=ORIENTED_EDGE('',*,*,#7708,.T.);
#10140=ORIENTED_EDGE('',*,*,#7704,.F.);
#10141=ORIENTED_EDGE('',*,*,#7709,.F.);
#10142=ORIENTED_EDGE('',*,*,#7710,.T.);
#10143=ORIENTED_EDGE('',*,*,#7711,.T.);
#10144=ORIENTED_EDGE('',*,*,#7707,.F.);
#10145=ORIENTED_EDGE('',*,*,#7712,.F.);
#10146=ORIENTED_EDGE('',*,*,#7713,.T.);
#10147=ORIENTED_EDGE('',*,*,#7714,.T.);
#10148=ORIENTED_EDGE('',*,*,#7710,.F.);
#10149=ORIENTED_EDGE('',*,*,#7715,.F.);
#10150=ORIENTED_EDGE('',*,*,#7716,.T.);
#10151=ORIENTED_EDGE('',*,*,#7717,.T.);
#10152=ORIENTED_EDGE('',*,*,#7713,.F.);
#10153=ORIENTED_EDGE('',*,*,#7718,.F.);
#10154=ORIENTED_EDGE('',*,*,#7719,.T.);
#10155=ORIENTED_EDGE('',*,*,#7720,.T.);
#10156=ORIENTED_EDGE('',*,*,#7716,.F.);
#10157=ORIENTED_EDGE('',*,*,#7721,.F.);
#10158=ORIENTED_EDGE('',*,*,#7722,.T.);
#10159=ORIENTED_EDGE('',*,*,#7723,.T.);
#10160=ORIENTED_EDGE('',*,*,#7719,.F.);
#10161=ORIENTED_EDGE('',*,*,#7724,.F.);
#10162=ORIENTED_EDGE('',*,*,#7725,.T.);
#10163=ORIENTED_EDGE('',*,*,#7726,.T.);
#10164=ORIENTED_EDGE('',*,*,#7722,.F.);
#10165=ORIENTED_EDGE('',*,*,#7727,.F.);
#10166=ORIENTED_EDGE('',*,*,#7728,.T.);
#10167=ORIENTED_EDGE('',*,*,#7729,.T.);
#10168=ORIENTED_EDGE('',*,*,#7725,.F.);
#10169=ORIENTED_EDGE('',*,*,#7730,.F.);
#10170=ORIENTED_EDGE('',*,*,#7731,.T.);
#10171=ORIENTED_EDGE('',*,*,#7732,.T.);
#10172=ORIENTED_EDGE('',*,*,#7728,.F.);
#10173=ORIENTED_EDGE('',*,*,#7733,.F.);
#10174=ORIENTED_EDGE('',*,*,#7734,.F.);
#10175=ORIENTED_EDGE('',*,*,#7735,.F.);
#10176=ORIENTED_EDGE('',*,*,#7736,.F.);
#10177=ORIENTED_EDGE('',*,*,#7737,.T.);
#10178=ORIENTED_EDGE('',*,*,#7738,.T.);
#10179=ORIENTED_EDGE('',*,*,#7739,.T.);
#10180=ORIENTED_EDGE('',*,*,#7740,.T.);
#10181=ORIENTED_EDGE('',*,*,#7741,.T.);
#10182=ORIENTED_EDGE('',*,*,#7742,.T.);
#10183=ORIENTED_EDGE('',*,*,#7741,.F.);
#10184=ORIENTED_EDGE('',*,*,#7743,.T.);
#10185=ORIENTED_EDGE('',*,*,#7744,.T.);
#10186=ORIENTED_EDGE('',*,*,#7745,.T.);
#10187=ORIENTED_EDGE('',*,*,#7746,.T.);
#10188=ORIENTED_EDGE('',*,*,#7738,.F.);
#10189=ORIENTED_EDGE('',*,*,#7747,.T.);
#10190=ORIENTED_EDGE('',*,*,#7748,.T.);
#10191=ORIENTED_EDGE('',*,*,#7749,.T.);
#10192=ORIENTED_EDGE('',*,*,#7745,.F.);
#10193=ORIENTED_EDGE('',*,*,#7750,.T.);
#10194=ORIENTED_EDGE('',*,*,#7751,.T.);
#10195=ORIENTED_EDGE('',*,*,#7752,.T.);
#10196=ORIENTED_EDGE('',*,*,#7748,.F.);
#10197=ORIENTED_EDGE('',*,*,#7753,.T.);
#10198=ORIENTED_EDGE('',*,*,#7754,.T.);
#10199=ORIENTED_EDGE('',*,*,#7755,.T.);
#10200=ORIENTED_EDGE('',*,*,#7751,.F.);
#10201=ORIENTED_EDGE('',*,*,#7756,.T.);
#10202=ORIENTED_EDGE('',*,*,#7757,.T.);
#10203=ORIENTED_EDGE('',*,*,#7758,.T.);
#10204=ORIENTED_EDGE('',*,*,#7754,.F.);
#10205=ORIENTED_EDGE('',*,*,#7759,.T.);
#10206=ORIENTED_EDGE('',*,*,#7760,.T.);
#10207=ORIENTED_EDGE('',*,*,#7761,.T.);
#10208=ORIENTED_EDGE('',*,*,#7757,.F.);
#10209=ORIENTED_EDGE('',*,*,#7762,.T.);
#10210=ORIENTED_EDGE('',*,*,#7763,.T.);
#10211=ORIENTED_EDGE('',*,*,#7764,.T.);
#10212=ORIENTED_EDGE('',*,*,#7760,.F.);
#10213=ORIENTED_EDGE('',*,*,#7765,.T.);
#10214=ORIENTED_EDGE('',*,*,#7766,.T.);
#10215=ORIENTED_EDGE('',*,*,#7767,.T.);
#10216=ORIENTED_EDGE('',*,*,#7763,.F.);
#10217=ORIENTED_EDGE('',*,*,#7768,.T.);
#10218=ORIENTED_EDGE('',*,*,#7769,.T.);
#10219=ORIENTED_EDGE('',*,*,#7770,.T.);
#10220=ORIENTED_EDGE('',*,*,#7766,.F.);
#10221=ORIENTED_EDGE('',*,*,#7771,.T.);
#10222=ORIENTED_EDGE('',*,*,#7772,.T.);
#10223=ORIENTED_EDGE('',*,*,#7773,.T.);
#10224=ORIENTED_EDGE('',*,*,#7769,.F.);
#10225=ORIENTED_EDGE('',*,*,#7774,.T.);
#10226=ORIENTED_EDGE('',*,*,#7775,.T.);
#10227=ORIENTED_EDGE('',*,*,#7776,.T.);
#10228=ORIENTED_EDGE('',*,*,#7772,.F.);
#10229=ORIENTED_EDGE('',*,*,#7777,.T.);
#10230=ORIENTED_EDGE('',*,*,#7778,.T.);
#10231=ORIENTED_EDGE('',*,*,#7779,.T.);
#10232=ORIENTED_EDGE('',*,*,#7775,.F.);
#10233=ORIENTED_EDGE('',*,*,#7780,.T.);
#10234=ORIENTED_EDGE('',*,*,#7781,.T.);
#10235=ORIENTED_EDGE('',*,*,#7782,.T.);
#10236=ORIENTED_EDGE('',*,*,#7778,.F.);
#10237=ORIENTED_EDGE('',*,*,#7783,.T.);
#10238=ORIENTED_EDGE('',*,*,#7784,.T.);
#10239=ORIENTED_EDGE('',*,*,#7785,.T.);
#10240=ORIENTED_EDGE('',*,*,#7781,.F.);
#10241=ORIENTED_EDGE('',*,*,#7786,.T.);
#10242=ORIENTED_EDGE('',*,*,#7787,.T.);
#10243=ORIENTED_EDGE('',*,*,#7788,.T.);
#10244=ORIENTED_EDGE('',*,*,#7784,.F.);
#10245=ORIENTED_EDGE('',*,*,#7789,.T.);
#10246=ORIENTED_EDGE('',*,*,#7790,.T.);
#10247=ORIENTED_EDGE('',*,*,#7791,.T.);
#10248=ORIENTED_EDGE('',*,*,#7787,.F.);
#10249=ORIENTED_EDGE('',*,*,#7792,.T.);
#10250=ORIENTED_EDGE('',*,*,#7793,.F.);
#10251=ORIENTED_EDGE('',*,*,#7794,.T.);
#10252=ORIENTED_EDGE('',*,*,#7795,.F.);
#10253=ORIENTED_EDGE('',*,*,#7796,.T.);
#10254=ORIENTED_EDGE('',*,*,#7797,.T.);
#10255=ORIENTED_EDGE('',*,*,#7798,.T.);
#10256=ORIENTED_EDGE('',*,*,#7799,.F.);
#10257=ORIENTED_EDGE('',*,*,#7800,.F.);
#10258=ORIENTED_EDGE('',*,*,#7801,.T.);
#10259=ORIENTED_EDGE('',*,*,#7802,.T.);
#10260=ORIENTED_EDGE('',*,*,#7797,.F.);
#10261=ORIENTED_EDGE('',*,*,#7803,.F.);
#10262=ORIENTED_EDGE('',*,*,#7804,.T.);
#10263=ORIENTED_EDGE('',*,*,#7805,.T.);
#10264=ORIENTED_EDGE('',*,*,#7801,.F.);
#10265=ORIENTED_EDGE('',*,*,#7806,.F.);
#10266=ORIENTED_EDGE('',*,*,#7807,.T.);
#10267=ORIENTED_EDGE('',*,*,#7808,.T.);
#10268=ORIENTED_EDGE('',*,*,#7804,.F.);
#10269=ORIENTED_EDGE('',*,*,#7809,.F.);
#10270=ORIENTED_EDGE('',*,*,#7810,.T.);
#10271=ORIENTED_EDGE('',*,*,#7811,.T.);
#10272=ORIENTED_EDGE('',*,*,#7807,.F.);
#10273=ORIENTED_EDGE('',*,*,#7812,.F.);
#10274=ORIENTED_EDGE('',*,*,#7813,.T.);
#10275=ORIENTED_EDGE('',*,*,#7814,.T.);
#10276=ORIENTED_EDGE('',*,*,#7810,.F.);
#10277=ORIENTED_EDGE('',*,*,#7815,.F.);
#10278=ORIENTED_EDGE('',*,*,#7816,.T.);
#10279=ORIENTED_EDGE('',*,*,#7817,.T.);
#10280=ORIENTED_EDGE('',*,*,#7813,.F.);
#10281=ORIENTED_EDGE('',*,*,#7818,.F.);
#10282=ORIENTED_EDGE('',*,*,#7819,.T.);
#10283=ORIENTED_EDGE('',*,*,#7820,.T.);
#10284=ORIENTED_EDGE('',*,*,#7816,.F.);
#10285=ORIENTED_EDGE('',*,*,#7821,.F.);
#10286=ORIENTED_EDGE('',*,*,#7822,.T.);
#10287=ORIENTED_EDGE('',*,*,#7823,.T.);
#10288=ORIENTED_EDGE('',*,*,#7819,.F.);
#10289=ORIENTED_EDGE('',*,*,#7824,.F.);
#10290=ORIENTED_EDGE('',*,*,#7825,.T.);
#10291=ORIENTED_EDGE('',*,*,#7826,.T.);
#10292=ORIENTED_EDGE('',*,*,#7822,.F.);
#10293=ORIENTED_EDGE('',*,*,#7827,.F.);
#10294=ORIENTED_EDGE('',*,*,#7828,.T.);
#10295=ORIENTED_EDGE('',*,*,#7829,.T.);
#10296=ORIENTED_EDGE('',*,*,#7825,.F.);
#10297=ORIENTED_EDGE('',*,*,#7830,.F.);
#10298=ORIENTED_EDGE('',*,*,#7831,.T.);
#10299=ORIENTED_EDGE('',*,*,#7832,.T.);
#10300=ORIENTED_EDGE('',*,*,#7828,.F.);
#10301=ORIENTED_EDGE('',*,*,#7833,.F.);
#10302=ORIENTED_EDGE('',*,*,#7834,.T.);
#10303=ORIENTED_EDGE('',*,*,#7835,.T.);
#10304=ORIENTED_EDGE('',*,*,#7831,.F.);
#10305=ORIENTED_EDGE('',*,*,#7836,.F.);
#10306=ORIENTED_EDGE('',*,*,#7837,.T.);
#10307=ORIENTED_EDGE('',*,*,#7838,.T.);
#10308=ORIENTED_EDGE('',*,*,#7834,.F.);
#10309=ORIENTED_EDGE('',*,*,#7839,.F.);
#10310=ORIENTED_EDGE('',*,*,#7840,.T.);
#10311=ORIENTED_EDGE('',*,*,#7841,.T.);
#10312=ORIENTED_EDGE('',*,*,#7837,.F.);
#10313=ORIENTED_EDGE('',*,*,#7842,.F.);
#10314=ORIENTED_EDGE('',*,*,#7843,.T.);
#10315=ORIENTED_EDGE('',*,*,#7844,.T.);
#10316=ORIENTED_EDGE('',*,*,#7840,.F.);
#10317=ORIENTED_EDGE('',*,*,#7845,.F.);
#10318=ORIENTED_EDGE('',*,*,#7846,.T.);
#10319=ORIENTED_EDGE('',*,*,#7847,.T.);
#10320=ORIENTED_EDGE('',*,*,#7843,.F.);
#10321=ORIENTED_EDGE('',*,*,#7848,.F.);
#10322=ORIENTED_EDGE('',*,*,#7849,.T.);
#10323=ORIENTED_EDGE('',*,*,#7850,.T.);
#10324=ORIENTED_EDGE('',*,*,#7846,.F.);
#10325=ORIENTED_EDGE('',*,*,#7851,.F.);
#10326=ORIENTED_EDGE('',*,*,#7852,.F.);
#10327=ORIENTED_EDGE('',*,*,#7853,.F.);
#10328=ORIENTED_EDGE('',*,*,#7854,.F.);
#10329=ORIENTED_EDGE('',*,*,#7855,.T.);
#10330=ORIENTED_EDGE('',*,*,#7856,.T.);
#10331=ORIENTED_EDGE('',*,*,#7857,.T.);
#10332=ORIENTED_EDGE('',*,*,#7858,.T.);
#10333=ORIENTED_EDGE('',*,*,#7859,.T.);
#10334=ORIENTED_EDGE('',*,*,#7860,.T.);
#10335=ORIENTED_EDGE('',*,*,#7859,.F.);
#10336=ORIENTED_EDGE('',*,*,#7861,.T.);
#10337=ORIENTED_EDGE('',*,*,#7862,.T.);
#10338=ORIENTED_EDGE('',*,*,#7863,.T.);
#10339=ORIENTED_EDGE('',*,*,#7864,.T.);
#10340=ORIENTED_EDGE('',*,*,#7856,.F.);
#10341=ORIENTED_EDGE('',*,*,#7865,.T.);
#10342=ORIENTED_EDGE('',*,*,#7866,.T.);
#10343=ORIENTED_EDGE('',*,*,#7867,.T.);
#10344=ORIENTED_EDGE('',*,*,#7863,.F.);
#10345=ORIENTED_EDGE('',*,*,#7868,.T.);
#10346=ORIENTED_EDGE('',*,*,#7869,.T.);
#10347=ORIENTED_EDGE('',*,*,#7870,.T.);
#10348=ORIENTED_EDGE('',*,*,#7866,.F.);
#10349=ORIENTED_EDGE('',*,*,#7871,.T.);
#10350=ORIENTED_EDGE('',*,*,#7872,.T.);
#10351=ORIENTED_EDGE('',*,*,#7873,.T.);
#10352=ORIENTED_EDGE('',*,*,#7869,.F.);
#10353=ORIENTED_EDGE('',*,*,#7874,.T.);
#10354=ORIENTED_EDGE('',*,*,#7875,.T.);
#10355=ORIENTED_EDGE('',*,*,#7876,.T.);
#10356=ORIENTED_EDGE('',*,*,#7872,.F.);
#10357=ORIENTED_EDGE('',*,*,#7877,.T.);
#10358=ORIENTED_EDGE('',*,*,#7878,.T.);
#10359=ORIENTED_EDGE('',*,*,#7879,.T.);
#10360=ORIENTED_EDGE('',*,*,#7875,.F.);
#10361=ORIENTED_EDGE('',*,*,#7880,.T.);
#10362=ORIENTED_EDGE('',*,*,#7881,.T.);
#10363=ORIENTED_EDGE('',*,*,#7882,.T.);
#10364=ORIENTED_EDGE('',*,*,#7878,.F.);
#10365=ORIENTED_EDGE('',*,*,#7883,.T.);
#10366=ORIENTED_EDGE('',*,*,#7884,.T.);
#10367=ORIENTED_EDGE('',*,*,#7885,.T.);
#10368=ORIENTED_EDGE('',*,*,#7881,.F.);
#10369=ORIENTED_EDGE('',*,*,#7886,.T.);
#10370=ORIENTED_EDGE('',*,*,#7887,.T.);
#10371=ORIENTED_EDGE('',*,*,#7888,.T.);
#10372=ORIENTED_EDGE('',*,*,#7884,.F.);
#10373=ORIENTED_EDGE('',*,*,#7889,.T.);
#10374=ORIENTED_EDGE('',*,*,#7890,.T.);
#10375=ORIENTED_EDGE('',*,*,#7891,.T.);
#10376=ORIENTED_EDGE('',*,*,#7887,.F.);
#10377=ORIENTED_EDGE('',*,*,#7892,.T.);
#10378=ORIENTED_EDGE('',*,*,#7893,.T.);
#10379=ORIENTED_EDGE('',*,*,#7894,.T.);
#10380=ORIENTED_EDGE('',*,*,#7890,.F.);
#10381=ORIENTED_EDGE('',*,*,#7895,.T.);
#10382=ORIENTED_EDGE('',*,*,#7896,.T.);
#10383=ORIENTED_EDGE('',*,*,#7897,.T.);
#10384=ORIENTED_EDGE('',*,*,#7893,.F.);
#10385=ORIENTED_EDGE('',*,*,#7898,.T.);
#10386=ORIENTED_EDGE('',*,*,#7899,.T.);
#10387=ORIENTED_EDGE('',*,*,#7900,.T.);
#10388=ORIENTED_EDGE('',*,*,#7896,.F.);
#10389=ORIENTED_EDGE('',*,*,#7901,.T.);
#10390=ORIENTED_EDGE('',*,*,#7902,.T.);
#10391=ORIENTED_EDGE('',*,*,#7903,.T.);
#10392=ORIENTED_EDGE('',*,*,#7899,.F.);
#10393=ORIENTED_EDGE('',*,*,#7904,.T.);
#10394=ORIENTED_EDGE('',*,*,#7905,.T.);
#10395=ORIENTED_EDGE('',*,*,#7906,.T.);
#10396=ORIENTED_EDGE('',*,*,#7902,.F.);
#10397=ORIENTED_EDGE('',*,*,#7907,.T.);
#10398=ORIENTED_EDGE('',*,*,#7908,.T.);
#10399=ORIENTED_EDGE('',*,*,#7909,.T.);
#10400=ORIENTED_EDGE('',*,*,#7905,.F.);
#10401=ORIENTED_EDGE('',*,*,#7910,.T.);
#10402=ORIENTED_EDGE('',*,*,#7911,.F.);
#10403=ORIENTED_EDGE('',*,*,#7912,.T.);
#10404=ORIENTED_EDGE('',*,*,#7913,.F.);
#10405=ORIENTED_EDGE('',*,*,#7914,.T.);
#10406=ORIENTED_EDGE('',*,*,#7915,.T.);
#10407=ORIENTED_EDGE('',*,*,#7916,.T.);
#10408=ORIENTED_EDGE('',*,*,#7917,.F.);
#10409=ORIENTED_EDGE('',*,*,#7918,.F.);
#10410=ORIENTED_EDGE('',*,*,#7919,.T.);
#10411=ORIENTED_EDGE('',*,*,#7920,.T.);
#10412=ORIENTED_EDGE('',*,*,#7915,.F.);
#10413=ORIENTED_EDGE('',*,*,#7921,.F.);
#10414=ORIENTED_EDGE('',*,*,#7922,.T.);
#10415=ORIENTED_EDGE('',*,*,#7923,.T.);
#10416=ORIENTED_EDGE('',*,*,#7919,.F.);
#10417=ORIENTED_EDGE('',*,*,#7924,.F.);
#10418=ORIENTED_EDGE('',*,*,#7925,.T.);
#10419=ORIENTED_EDGE('',*,*,#7926,.T.);
#10420=ORIENTED_EDGE('',*,*,#7922,.F.);
#10421=ORIENTED_EDGE('',*,*,#7927,.F.);
#10422=ORIENTED_EDGE('',*,*,#7928,.T.);
#10423=ORIENTED_EDGE('',*,*,#7929,.T.);
#10424=ORIENTED_EDGE('',*,*,#7925,.F.);
#10425=ORIENTED_EDGE('',*,*,#7930,.F.);
#10426=ORIENTED_EDGE('',*,*,#7931,.T.);
#10427=ORIENTED_EDGE('',*,*,#7932,.T.);
#10428=ORIENTED_EDGE('',*,*,#7928,.F.);
#10429=ORIENTED_EDGE('',*,*,#7933,.F.);
#10430=ORIENTED_EDGE('',*,*,#7934,.T.);
#10431=ORIENTED_EDGE('',*,*,#7935,.T.);
#10432=ORIENTED_EDGE('',*,*,#7931,.F.);
#10433=ORIENTED_EDGE('',*,*,#7936,.F.);
#10434=ORIENTED_EDGE('',*,*,#7937,.T.);
#10435=ORIENTED_EDGE('',*,*,#7938,.T.);
#10436=ORIENTED_EDGE('',*,*,#7934,.F.);
#10437=ORIENTED_EDGE('',*,*,#7939,.F.);
#10438=ORIENTED_EDGE('',*,*,#7940,.T.);
#10439=ORIENTED_EDGE('',*,*,#7941,.T.);
#10440=ORIENTED_EDGE('',*,*,#7937,.F.);
#10441=ORIENTED_EDGE('',*,*,#7942,.F.);
#10442=ORIENTED_EDGE('',*,*,#7943,.T.);
#10443=ORIENTED_EDGE('',*,*,#7944,.T.);
#10444=ORIENTED_EDGE('',*,*,#7940,.F.);
#10445=ORIENTED_EDGE('',*,*,#7945,.F.);
#10446=ORIENTED_EDGE('',*,*,#7946,.T.);
#10447=ORIENTED_EDGE('',*,*,#7947,.T.);
#10448=ORIENTED_EDGE('',*,*,#7943,.F.);
#10449=ORIENTED_EDGE('',*,*,#7948,.F.);
#10450=ORIENTED_EDGE('',*,*,#7949,.T.);
#10451=ORIENTED_EDGE('',*,*,#7950,.T.);
#10452=ORIENTED_EDGE('',*,*,#7946,.F.);
#10453=ORIENTED_EDGE('',*,*,#7951,.F.);
#10454=ORIENTED_EDGE('',*,*,#7952,.T.);
#10455=ORIENTED_EDGE('',*,*,#7953,.T.);
#10456=ORIENTED_EDGE('',*,*,#7949,.F.);
#10457=ORIENTED_EDGE('',*,*,#7954,.F.);
#10458=ORIENTED_EDGE('',*,*,#7955,.T.);
#10459=ORIENTED_EDGE('',*,*,#7956,.T.);
#10460=ORIENTED_EDGE('',*,*,#7952,.F.);
#10461=ORIENTED_EDGE('',*,*,#7957,.F.);
#10462=ORIENTED_EDGE('',*,*,#7958,.T.);
#10463=ORIENTED_EDGE('',*,*,#7959,.T.);
#10464=ORIENTED_EDGE('',*,*,#7955,.F.);
#10465=ORIENTED_EDGE('',*,*,#7960,.F.);
#10466=ORIENTED_EDGE('',*,*,#7961,.T.);
#10467=ORIENTED_EDGE('',*,*,#7962,.T.);
#10468=ORIENTED_EDGE('',*,*,#7958,.F.);
#10469=ORIENTED_EDGE('',*,*,#7963,.F.);
#10470=ORIENTED_EDGE('',*,*,#7964,.T.);
#10471=ORIENTED_EDGE('',*,*,#7965,.T.);
#10472=ORIENTED_EDGE('',*,*,#7961,.F.);
#10473=ORIENTED_EDGE('',*,*,#7966,.F.);
#10474=ORIENTED_EDGE('',*,*,#7967,.T.);
#10475=ORIENTED_EDGE('',*,*,#7968,.T.);
#10476=ORIENTED_EDGE('',*,*,#7964,.F.);
#10477=ORIENTED_EDGE('',*,*,#7969,.F.);
#10478=ORIENTED_EDGE('',*,*,#7970,.F.);
#10479=ORIENTED_EDGE('',*,*,#7971,.F.);
#10480=ORIENTED_EDGE('',*,*,#7972,.F.);
#10481=ORIENTED_EDGE('',*,*,#7973,.T.);
#10482=ORIENTED_EDGE('',*,*,#7974,.T.);
#10483=ORIENTED_EDGE('',*,*,#7975,.T.);
#10484=ORIENTED_EDGE('',*,*,#7976,.T.);
#10485=ORIENTED_EDGE('',*,*,#7977,.T.);
#10486=ORIENTED_EDGE('',*,*,#7978,.T.);
#10487=ORIENTED_EDGE('',*,*,#7977,.F.);
#10488=ORIENTED_EDGE('',*,*,#7979,.T.);
#10489=ORIENTED_EDGE('',*,*,#7980,.T.);
#10490=ORIENTED_EDGE('',*,*,#7981,.T.);
#10491=ORIENTED_EDGE('',*,*,#7982,.T.);
#10492=ORIENTED_EDGE('',*,*,#7974,.F.);
#10493=ORIENTED_EDGE('',*,*,#7983,.T.);
#10494=ORIENTED_EDGE('',*,*,#7984,.T.);
#10495=ORIENTED_EDGE('',*,*,#7985,.T.);
#10496=ORIENTED_EDGE('',*,*,#7981,.F.);
#10497=ORIENTED_EDGE('',*,*,#7986,.T.);
#10498=ORIENTED_EDGE('',*,*,#7987,.T.);
#10499=ORIENTED_EDGE('',*,*,#7988,.T.);
#10500=ORIENTED_EDGE('',*,*,#7984,.F.);
#10501=ORIENTED_EDGE('',*,*,#7989,.T.);
#10502=ORIENTED_EDGE('',*,*,#7990,.T.);
#10503=ORIENTED_EDGE('',*,*,#7991,.T.);
#10504=ORIENTED_EDGE('',*,*,#7987,.F.);
#10505=ORIENTED_EDGE('',*,*,#7992,.T.);
#10506=ORIENTED_EDGE('',*,*,#7993,.T.);
#10507=ORIENTED_EDGE('',*,*,#7994,.T.);
#10508=ORIENTED_EDGE('',*,*,#7990,.F.);
#10509=ORIENTED_EDGE('',*,*,#7995,.T.);
#10510=ORIENTED_EDGE('',*,*,#7996,.T.);
#10511=ORIENTED_EDGE('',*,*,#7997,.T.);
#10512=ORIENTED_EDGE('',*,*,#7993,.F.);
#10513=ORIENTED_EDGE('',*,*,#7998,.T.);
#10514=ORIENTED_EDGE('',*,*,#7999,.T.);
#10515=ORIENTED_EDGE('',*,*,#8000,.T.);
#10516=ORIENTED_EDGE('',*,*,#7996,.F.);
#10517=ORIENTED_EDGE('',*,*,#8001,.T.);
#10518=ORIENTED_EDGE('',*,*,#8002,.T.);
#10519=ORIENTED_EDGE('',*,*,#8003,.T.);
#10520=ORIENTED_EDGE('',*,*,#7999,.F.);
#10521=ORIENTED_EDGE('',*,*,#8004,.T.);
#10522=ORIENTED_EDGE('',*,*,#8005,.T.);
#10523=ORIENTED_EDGE('',*,*,#8006,.T.);
#10524=ORIENTED_EDGE('',*,*,#8002,.F.);
#10525=ORIENTED_EDGE('',*,*,#8007,.T.);
#10526=ORIENTED_EDGE('',*,*,#8008,.T.);
#10527=ORIENTED_EDGE('',*,*,#8009,.T.);
#10528=ORIENTED_EDGE('',*,*,#8005,.F.);
#10529=ORIENTED_EDGE('',*,*,#8010,.T.);
#10530=ORIENTED_EDGE('',*,*,#8011,.T.);
#10531=ORIENTED_EDGE('',*,*,#8012,.T.);
#10532=ORIENTED_EDGE('',*,*,#8008,.F.);
#10533=ORIENTED_EDGE('',*,*,#8013,.T.);
#10534=ORIENTED_EDGE('',*,*,#8014,.T.);
#10535=ORIENTED_EDGE('',*,*,#8015,.T.);
#10536=ORIENTED_EDGE('',*,*,#8011,.F.);
#10537=ORIENTED_EDGE('',*,*,#8016,.T.);
#10538=ORIENTED_EDGE('',*,*,#8017,.T.);
#10539=ORIENTED_EDGE('',*,*,#8018,.T.);
#10540=ORIENTED_EDGE('',*,*,#8014,.F.);
#10541=ORIENTED_EDGE('',*,*,#8019,.T.);
#10542=ORIENTED_EDGE('',*,*,#8020,.T.);
#10543=ORIENTED_EDGE('',*,*,#8021,.T.);
#10544=ORIENTED_EDGE('',*,*,#8017,.F.);
#10545=ORIENTED_EDGE('',*,*,#8022,.T.);
#10546=ORIENTED_EDGE('',*,*,#8023,.T.);
#10547=ORIENTED_EDGE('',*,*,#8024,.T.);
#10548=ORIENTED_EDGE('',*,*,#8020,.F.);
#10549=ORIENTED_EDGE('',*,*,#8025,.T.);
#10550=ORIENTED_EDGE('',*,*,#8026,.T.);
#10551=ORIENTED_EDGE('',*,*,#8027,.T.);
#10552=ORIENTED_EDGE('',*,*,#8023,.F.);
#10553=ORIENTED_EDGE('',*,*,#8028,.T.);
#10554=ORIENTED_EDGE('',*,*,#8029,.F.);
#10555=ORIENTED_EDGE('',*,*,#8030,.T.);
#10556=ORIENTED_EDGE('',*,*,#8031,.F.);
#10557=ORIENTED_EDGE('',*,*,#8032,.T.);
#10558=ORIENTED_EDGE('',*,*,#8033,.T.);
#10559=ORIENTED_EDGE('',*,*,#8034,.T.);
#10560=ORIENTED_EDGE('',*,*,#8035,.F.);
#10561=ORIENTED_EDGE('',*,*,#8036,.F.);
#10562=ORIENTED_EDGE('',*,*,#8037,.T.);
#10563=ORIENTED_EDGE('',*,*,#8038,.T.);
#10564=ORIENTED_EDGE('',*,*,#8033,.F.);
#10565=ORIENTED_EDGE('',*,*,#8039,.F.);
#10566=ORIENTED_EDGE('',*,*,#8040,.T.);
#10567=ORIENTED_EDGE('',*,*,#8041,.T.);
#10568=ORIENTED_EDGE('',*,*,#8037,.F.);
#10569=ORIENTED_EDGE('',*,*,#8042,.F.);
#10570=ORIENTED_EDGE('',*,*,#8043,.T.);
#10571=ORIENTED_EDGE('',*,*,#8044,.T.);
#10572=ORIENTED_EDGE('',*,*,#8040,.F.);
#10573=ORIENTED_EDGE('',*,*,#8045,.F.);
#10574=ORIENTED_EDGE('',*,*,#8046,.T.);
#10575=ORIENTED_EDGE('',*,*,#8047,.T.);
#10576=ORIENTED_EDGE('',*,*,#8043,.F.);
#10577=ORIENTED_EDGE('',*,*,#8048,.F.);
#10578=ORIENTED_EDGE('',*,*,#8049,.T.);
#10579=ORIENTED_EDGE('',*,*,#8050,.T.);
#10580=ORIENTED_EDGE('',*,*,#8046,.F.);
#10581=ORIENTED_EDGE('',*,*,#8051,.F.);
#10582=ORIENTED_EDGE('',*,*,#8052,.T.);
#10583=ORIENTED_EDGE('',*,*,#8053,.T.);
#10584=ORIENTED_EDGE('',*,*,#8049,.F.);
#10585=ORIENTED_EDGE('',*,*,#8054,.F.);
#10586=ORIENTED_EDGE('',*,*,#8055,.T.);
#10587=ORIENTED_EDGE('',*,*,#8056,.T.);
#10588=ORIENTED_EDGE('',*,*,#8052,.F.);
#10589=ORIENTED_EDGE('',*,*,#8057,.F.);
#10590=ORIENTED_EDGE('',*,*,#8058,.T.);
#10591=ORIENTED_EDGE('',*,*,#8059,.T.);
#10592=ORIENTED_EDGE('',*,*,#8055,.F.);
#10593=ORIENTED_EDGE('',*,*,#8060,.F.);
#10594=ORIENTED_EDGE('',*,*,#8061,.T.);
#10595=ORIENTED_EDGE('',*,*,#8062,.T.);
#10596=ORIENTED_EDGE('',*,*,#8058,.F.);
#10597=ORIENTED_EDGE('',*,*,#8063,.F.);
#10598=ORIENTED_EDGE('',*,*,#8064,.T.);
#10599=ORIENTED_EDGE('',*,*,#8065,.T.);
#10600=ORIENTED_EDGE('',*,*,#8061,.F.);
#10601=ORIENTED_EDGE('',*,*,#8066,.F.);
#10602=ORIENTED_EDGE('',*,*,#8067,.T.);
#10603=ORIENTED_EDGE('',*,*,#8068,.T.);
#10604=ORIENTED_EDGE('',*,*,#8064,.F.);
#10605=ORIENTED_EDGE('',*,*,#8069,.F.);
#10606=ORIENTED_EDGE('',*,*,#8070,.T.);
#10607=ORIENTED_EDGE('',*,*,#8071,.T.);
#10608=ORIENTED_EDGE('',*,*,#8067,.F.);
#10609=ORIENTED_EDGE('',*,*,#8072,.F.);
#10610=ORIENTED_EDGE('',*,*,#8073,.T.);
#10611=ORIENTED_EDGE('',*,*,#8074,.T.);
#10612=ORIENTED_EDGE('',*,*,#8070,.F.);
#10613=ORIENTED_EDGE('',*,*,#8075,.F.);
#10614=ORIENTED_EDGE('',*,*,#8076,.T.);
#10615=ORIENTED_EDGE('',*,*,#8077,.T.);
#10616=ORIENTED_EDGE('',*,*,#8073,.F.);
#10617=ORIENTED_EDGE('',*,*,#8078,.F.);
#10618=ORIENTED_EDGE('',*,*,#8079,.T.);
#10619=ORIENTED_EDGE('',*,*,#8080,.T.);
#10620=ORIENTED_EDGE('',*,*,#8076,.F.);
#10621=ORIENTED_EDGE('',*,*,#8081,.F.);
#10622=ORIENTED_EDGE('',*,*,#8082,.T.);
#10623=ORIENTED_EDGE('',*,*,#8083,.T.);
#10624=ORIENTED_EDGE('',*,*,#8079,.F.);
#10625=ORIENTED_EDGE('',*,*,#8084,.F.);
#10626=ORIENTED_EDGE('',*,*,#8085,.T.);
#10627=ORIENTED_EDGE('',*,*,#8086,.T.);
#10628=ORIENTED_EDGE('',*,*,#8082,.F.);
#10629=ORIENTED_EDGE('',*,*,#8087,.F.);
#10630=ORIENTED_EDGE('',*,*,#8088,.F.);
#10631=ORIENTED_EDGE('',*,*,#8089,.F.);
#10632=ORIENTED_EDGE('',*,*,#8090,.F.);
#10633=ORIENTED_EDGE('',*,*,#8091,.T.);
#10634=ORIENTED_EDGE('',*,*,#8092,.T.);
#10635=ORIENTED_EDGE('',*,*,#8093,.T.);
#10636=ORIENTED_EDGE('',*,*,#8094,.T.);
#10637=ORIENTED_EDGE('',*,*,#8095,.T.);
#10638=ORIENTED_EDGE('',*,*,#8096,.T.);
#10639=ORIENTED_EDGE('',*,*,#8095,.F.);
#10640=ORIENTED_EDGE('',*,*,#8097,.T.);
#10641=ORIENTED_EDGE('',*,*,#8098,.T.);
#10642=ORIENTED_EDGE('',*,*,#8099,.T.);
#10643=ORIENTED_EDGE('',*,*,#8100,.T.);
#10644=ORIENTED_EDGE('',*,*,#8092,.F.);
#10645=ORIENTED_EDGE('',*,*,#8101,.T.);
#10646=ORIENTED_EDGE('',*,*,#8102,.T.);
#10647=ORIENTED_EDGE('',*,*,#8103,.T.);
#10648=ORIENTED_EDGE('',*,*,#8099,.F.);
#10649=ORIENTED_EDGE('',*,*,#8104,.T.);
#10650=ORIENTED_EDGE('',*,*,#8105,.T.);
#10651=ORIENTED_EDGE('',*,*,#8106,.T.);
#10652=ORIENTED_EDGE('',*,*,#8102,.F.);
#10653=ORIENTED_EDGE('',*,*,#8107,.T.);
#10654=ORIENTED_EDGE('',*,*,#8108,.T.);
#10655=ORIENTED_EDGE('',*,*,#8109,.T.);
#10656=ORIENTED_EDGE('',*,*,#8105,.F.);
#10657=ORIENTED_EDGE('',*,*,#8110,.T.);
#10658=ORIENTED_EDGE('',*,*,#8111,.T.);
#10659=ORIENTED_EDGE('',*,*,#8112,.T.);
#10660=ORIENTED_EDGE('',*,*,#8108,.F.);
#10661=ORIENTED_EDGE('',*,*,#8113,.T.);
#10662=ORIENTED_EDGE('',*,*,#8114,.T.);
#10663=ORIENTED_EDGE('',*,*,#8115,.T.);
#10664=ORIENTED_EDGE('',*,*,#8111,.F.);
#10665=ORIENTED_EDGE('',*,*,#8116,.T.);
#10666=ORIENTED_EDGE('',*,*,#8117,.T.);
#10667=ORIENTED_EDGE('',*,*,#8118,.T.);
#10668=ORIENTED_EDGE('',*,*,#8114,.F.);
#10669=ORIENTED_EDGE('',*,*,#8119,.T.);
#10670=ORIENTED_EDGE('',*,*,#8120,.T.);
#10671=ORIENTED_EDGE('',*,*,#8121,.T.);
#10672=ORIENTED_EDGE('',*,*,#8117,.F.);
#10673=ORIENTED_EDGE('',*,*,#8122,.T.);
#10674=ORIENTED_EDGE('',*,*,#8123,.T.);
#10675=ORIENTED_EDGE('',*,*,#8124,.T.);
#10676=ORIENTED_EDGE('',*,*,#8120,.F.);
#10677=ORIENTED_EDGE('',*,*,#8125,.T.);
#10678=ORIENTED_EDGE('',*,*,#8126,.T.);
#10679=ORIENTED_EDGE('',*,*,#8127,.T.);
#10680=ORIENTED_EDGE('',*,*,#8123,.F.);
#10681=ORIENTED_EDGE('',*,*,#8128,.T.);
#10682=ORIENTED_EDGE('',*,*,#8129,.T.);
#10683=ORIENTED_EDGE('',*,*,#8130,.T.);
#10684=ORIENTED_EDGE('',*,*,#8126,.F.);
#10685=ORIENTED_EDGE('',*,*,#8131,.T.);
#10686=ORIENTED_EDGE('',*,*,#8132,.T.);
#10687=ORIENTED_EDGE('',*,*,#8133,.T.);
#10688=ORIENTED_EDGE('',*,*,#8129,.F.);
#10689=ORIENTED_EDGE('',*,*,#8134,.T.);
#10690=ORIENTED_EDGE('',*,*,#8135,.T.);
#10691=ORIENTED_EDGE('',*,*,#8136,.T.);
#10692=ORIENTED_EDGE('',*,*,#8132,.F.);
#10693=ORIENTED_EDGE('',*,*,#8137,.T.);
#10694=ORIENTED_EDGE('',*,*,#8138,.T.);
#10695=ORIENTED_EDGE('',*,*,#8139,.T.);
#10696=ORIENTED_EDGE('',*,*,#8135,.F.);
#10697=ORIENTED_EDGE('',*,*,#8140,.T.);
#10698=ORIENTED_EDGE('',*,*,#8141,.T.);
#10699=ORIENTED_EDGE('',*,*,#8142,.T.);
#10700=ORIENTED_EDGE('',*,*,#8138,.F.);
#10701=ORIENTED_EDGE('',*,*,#8143,.T.);
#10702=ORIENTED_EDGE('',*,*,#8144,.T.);
#10703=ORIENTED_EDGE('',*,*,#8145,.T.);
#10704=ORIENTED_EDGE('',*,*,#8141,.F.);
#10705=ORIENTED_EDGE('',*,*,#8146,.T.);
#10706=ORIENTED_EDGE('',*,*,#8147,.F.);
#10707=ORIENTED_EDGE('',*,*,#8148,.T.);
#10708=ORIENTED_EDGE('',*,*,#8149,.F.);
#10709=ORIENTED_EDGE('',*,*,#8150,.T.);
#10710=ORIENTED_EDGE('',*,*,#8151,.T.);
#10711=ORIENTED_EDGE('',*,*,#8152,.T.);
#10712=ORIENTED_EDGE('',*,*,#8153,.F.);
#10713=ORIENTED_EDGE('',*,*,#8154,.F.);
#10714=ORIENTED_EDGE('',*,*,#8155,.T.);
#10715=ORIENTED_EDGE('',*,*,#8156,.T.);
#10716=ORIENTED_EDGE('',*,*,#8151,.F.);
#10717=ORIENTED_EDGE('',*,*,#8157,.F.);
#10718=ORIENTED_EDGE('',*,*,#8158,.T.);
#10719=ORIENTED_EDGE('',*,*,#8159,.T.);
#10720=ORIENTED_EDGE('',*,*,#8155,.F.);
#10721=ORIENTED_EDGE('',*,*,#8160,.F.);
#10722=ORIENTED_EDGE('',*,*,#8161,.T.);
#10723=ORIENTED_EDGE('',*,*,#8162,.T.);
#10724=ORIENTED_EDGE('',*,*,#8158,.F.);
#10725=ORIENTED_EDGE('',*,*,#8163,.F.);
#10726=ORIENTED_EDGE('',*,*,#8164,.T.);
#10727=ORIENTED_EDGE('',*,*,#8165,.T.);
#10728=ORIENTED_EDGE('',*,*,#8161,.F.);
#10729=ORIENTED_EDGE('',*,*,#8166,.F.);
#10730=ORIENTED_EDGE('',*,*,#8167,.T.);
#10731=ORIENTED_EDGE('',*,*,#8168,.T.);
#10732=ORIENTED_EDGE('',*,*,#8164,.F.);
#10733=ORIENTED_EDGE('',*,*,#8169,.F.);
#10734=ORIENTED_EDGE('',*,*,#8170,.T.);
#10735=ORIENTED_EDGE('',*,*,#8171,.T.);
#10736=ORIENTED_EDGE('',*,*,#8167,.F.);
#10737=ORIENTED_EDGE('',*,*,#8172,.F.);
#10738=ORIENTED_EDGE('',*,*,#8173,.T.);
#10739=ORIENTED_EDGE('',*,*,#8174,.T.);
#10740=ORIENTED_EDGE('',*,*,#8170,.F.);
#10741=ORIENTED_EDGE('',*,*,#8175,.F.);
#10742=ORIENTED_EDGE('',*,*,#8176,.T.);
#10743=ORIENTED_EDGE('',*,*,#8177,.T.);
#10744=ORIENTED_EDGE('',*,*,#8173,.F.);
#10745=ORIENTED_EDGE('',*,*,#8178,.F.);
#10746=ORIENTED_EDGE('',*,*,#8179,.T.);
#10747=ORIENTED_EDGE('',*,*,#8180,.T.);
#10748=ORIENTED_EDGE('',*,*,#8176,.F.);
#10749=ORIENTED_EDGE('',*,*,#8181,.F.);
#10750=ORIENTED_EDGE('',*,*,#8182,.T.);
#10751=ORIENTED_EDGE('',*,*,#8183,.T.);
#10752=ORIENTED_EDGE('',*,*,#8179,.F.);
#10753=ORIENTED_EDGE('',*,*,#8184,.F.);
#10754=ORIENTED_EDGE('',*,*,#8185,.T.);
#10755=ORIENTED_EDGE('',*,*,#8186,.T.);
#10756=ORIENTED_EDGE('',*,*,#8182,.F.);
#10757=ORIENTED_EDGE('',*,*,#8187,.F.);
#10758=ORIENTED_EDGE('',*,*,#8188,.T.);
#10759=ORIENTED_EDGE('',*,*,#8189,.T.);
#10760=ORIENTED_EDGE('',*,*,#8185,.F.);
#10761=ORIENTED_EDGE('',*,*,#8190,.F.);
#10762=ORIENTED_EDGE('',*,*,#8191,.T.);
#10763=ORIENTED_EDGE('',*,*,#8192,.T.);
#10764=ORIENTED_EDGE('',*,*,#8188,.F.);
#10765=ORIENTED_EDGE('',*,*,#8193,.F.);
#10766=ORIENTED_EDGE('',*,*,#8194,.T.);
#10767=ORIENTED_EDGE('',*,*,#8195,.T.);
#10768=ORIENTED_EDGE('',*,*,#8191,.F.);
#10769=ORIENTED_EDGE('',*,*,#8196,.F.);
#10770=ORIENTED_EDGE('',*,*,#8197,.T.);
#10771=ORIENTED_EDGE('',*,*,#8198,.T.);
#10772=ORIENTED_EDGE('',*,*,#8194,.F.);
#10773=ORIENTED_EDGE('',*,*,#8199,.F.);
#10774=ORIENTED_EDGE('',*,*,#8200,.T.);
#10775=ORIENTED_EDGE('',*,*,#8201,.T.);
#10776=ORIENTED_EDGE('',*,*,#8197,.F.);
#10777=ORIENTED_EDGE('',*,*,#8202,.F.);
#10778=ORIENTED_EDGE('',*,*,#8203,.T.);
#10779=ORIENTED_EDGE('',*,*,#8204,.T.);
#10780=ORIENTED_EDGE('',*,*,#8200,.F.);
#10781=ORIENTED_EDGE('',*,*,#8205,.F.);
#10782=ORIENTED_EDGE('',*,*,#8206,.F.);
#10783=ORIENTED_EDGE('',*,*,#8207,.F.);
#10784=ORIENTED_EDGE('',*,*,#8208,.F.);
#10785=ORIENTED_EDGE('',*,*,#8209,.T.);
#10786=ORIENTED_EDGE('',*,*,#8210,.T.);
#10787=ORIENTED_EDGE('',*,*,#8211,.T.);
#10788=ORIENTED_EDGE('',*,*,#8212,.T.);
#10789=ORIENTED_EDGE('',*,*,#8213,.T.);
#10790=ORIENTED_EDGE('',*,*,#8214,.T.);
#10791=ORIENTED_EDGE('',*,*,#8213,.F.);
#10792=ORIENTED_EDGE('',*,*,#8215,.T.);
#10793=ORIENTED_EDGE('',*,*,#8216,.T.);
#10794=ORIENTED_EDGE('',*,*,#8217,.T.);
#10795=ORIENTED_EDGE('',*,*,#8218,.T.);
#10796=ORIENTED_EDGE('',*,*,#8210,.F.);
#10797=ORIENTED_EDGE('',*,*,#8219,.T.);
#10798=ORIENTED_EDGE('',*,*,#8220,.T.);
#10799=ORIENTED_EDGE('',*,*,#8221,.T.);
#10800=ORIENTED_EDGE('',*,*,#8217,.F.);
#10801=ORIENTED_EDGE('',*,*,#8222,.T.);
#10802=ORIENTED_EDGE('',*,*,#8223,.T.);
#10803=ORIENTED_EDGE('',*,*,#8224,.T.);
#10804=ORIENTED_EDGE('',*,*,#8220,.F.);
#10805=ORIENTED_EDGE('',*,*,#8225,.T.);
#10806=ORIENTED_EDGE('',*,*,#8226,.T.);
#10807=ORIENTED_EDGE('',*,*,#8227,.T.);
#10808=ORIENTED_EDGE('',*,*,#8223,.F.);
#10809=ORIENTED_EDGE('',*,*,#8228,.T.);
#10810=ORIENTED_EDGE('',*,*,#8229,.T.);
#10811=ORIENTED_EDGE('',*,*,#8230,.T.);
#10812=ORIENTED_EDGE('',*,*,#8226,.F.);
#10813=ORIENTED_EDGE('',*,*,#8231,.T.);
#10814=ORIENTED_EDGE('',*,*,#8232,.T.);
#10815=ORIENTED_EDGE('',*,*,#8233,.T.);
#10816=ORIENTED_EDGE('',*,*,#8229,.F.);
#10817=ORIENTED_EDGE('',*,*,#8234,.T.);
#10818=ORIENTED_EDGE('',*,*,#8235,.T.);
#10819=ORIENTED_EDGE('',*,*,#8236,.T.);
#10820=ORIENTED_EDGE('',*,*,#8232,.F.);
#10821=ORIENTED_EDGE('',*,*,#8237,.T.);
#10822=ORIENTED_EDGE('',*,*,#8238,.T.);
#10823=ORIENTED_EDGE('',*,*,#8239,.T.);
#10824=ORIENTED_EDGE('',*,*,#8235,.F.);
#10825=ORIENTED_EDGE('',*,*,#8240,.T.);
#10826=ORIENTED_EDGE('',*,*,#8241,.T.);
#10827=ORIENTED_EDGE('',*,*,#8242,.T.);
#10828=ORIENTED_EDGE('',*,*,#8238,.F.);
#10829=ORIENTED_EDGE('',*,*,#8243,.T.);
#10830=ORIENTED_EDGE('',*,*,#8244,.T.);
#10831=ORIENTED_EDGE('',*,*,#8245,.T.);
#10832=ORIENTED_EDGE('',*,*,#8241,.F.);
#10833=ORIENTED_EDGE('',*,*,#8246,.T.);
#10834=ORIENTED_EDGE('',*,*,#8247,.T.);
#10835=ORIENTED_EDGE('',*,*,#8248,.T.);
#10836=ORIENTED_EDGE('',*,*,#8244,.F.);
#10837=ORIENTED_EDGE('',*,*,#8249,.T.);
#10838=ORIENTED_EDGE('',*,*,#8250,.T.);
#10839=ORIENTED_EDGE('',*,*,#8251,.T.);
#10840=ORIENTED_EDGE('',*,*,#8247,.F.);
#10841=ORIENTED_EDGE('',*,*,#8252,.T.);
#10842=ORIENTED_EDGE('',*,*,#8253,.T.);
#10843=ORIENTED_EDGE('',*,*,#8254,.T.);
#10844=ORIENTED_EDGE('',*,*,#8250,.F.);
#10845=ORIENTED_EDGE('',*,*,#8255,.T.);
#10846=ORIENTED_EDGE('',*,*,#8256,.T.);
#10847=ORIENTED_EDGE('',*,*,#8257,.T.);
#10848=ORIENTED_EDGE('',*,*,#8253,.F.);
#10849=ORIENTED_EDGE('',*,*,#8258,.T.);
#10850=ORIENTED_EDGE('',*,*,#8259,.T.);
#10851=ORIENTED_EDGE('',*,*,#8260,.T.);
#10852=ORIENTED_EDGE('',*,*,#8256,.F.);
#10853=ORIENTED_EDGE('',*,*,#8261,.T.);
#10854=ORIENTED_EDGE('',*,*,#8262,.T.);
#10855=ORIENTED_EDGE('',*,*,#8263,.T.);
#10856=ORIENTED_EDGE('',*,*,#8259,.F.);
#10857=ORIENTED_EDGE('',*,*,#8264,.T.);
#10858=ORIENTED_EDGE('',*,*,#8265,.F.);
#10859=ORIENTED_EDGE('',*,*,#8266,.T.);
#10860=ORIENTED_EDGE('',*,*,#8267,.F.);
#10861=ORIENTED_EDGE('',*,*,#8268,.T.);
#10862=ORIENTED_EDGE('',*,*,#8269,.T.);
#10863=ORIENTED_EDGE('',*,*,#8270,.T.);
#10864=ORIENTED_EDGE('',*,*,#8271,.F.);
#10865=ORIENTED_EDGE('',*,*,#8272,.F.);
#10866=ORIENTED_EDGE('',*,*,#8273,.T.);
#10867=ORIENTED_EDGE('',*,*,#8274,.T.);
#10868=ORIENTED_EDGE('',*,*,#8269,.F.);
#10869=ORIENTED_EDGE('',*,*,#8275,.F.);
#10870=ORIENTED_EDGE('',*,*,#8276,.T.);
#10871=ORIENTED_EDGE('',*,*,#8277,.T.);
#10872=ORIENTED_EDGE('',*,*,#8273,.F.);
#10873=ORIENTED_EDGE('',*,*,#8278,.F.);
#10874=ORIENTED_EDGE('',*,*,#8279,.T.);
#10875=ORIENTED_EDGE('',*,*,#8280,.T.);
#10876=ORIENTED_EDGE('',*,*,#8276,.F.);
#10877=ORIENTED_EDGE('',*,*,#8281,.F.);
#10878=ORIENTED_EDGE('',*,*,#8282,.T.);
#10879=ORIENTED_EDGE('',*,*,#8283,.T.);
#10880=ORIENTED_EDGE('',*,*,#8279,.F.);
#10881=ORIENTED_EDGE('',*,*,#8284,.F.);
#10882=ORIENTED_EDGE('',*,*,#8285,.T.);
#10883=ORIENTED_EDGE('',*,*,#8286,.T.);
#10884=ORIENTED_EDGE('',*,*,#8282,.F.);
#10885=ORIENTED_EDGE('',*,*,#8287,.F.);
#10886=ORIENTED_EDGE('',*,*,#8288,.T.);
#10887=ORIENTED_EDGE('',*,*,#8289,.T.);
#10888=ORIENTED_EDGE('',*,*,#8285,.F.);
#10889=ORIENTED_EDGE('',*,*,#8290,.F.);
#10890=ORIENTED_EDGE('',*,*,#8291,.T.);
#10891=ORIENTED_EDGE('',*,*,#8292,.T.);
#10892=ORIENTED_EDGE('',*,*,#8288,.F.);
#10893=ORIENTED_EDGE('',*,*,#8293,.F.);
#10894=ORIENTED_EDGE('',*,*,#8294,.T.);
#10895=ORIENTED_EDGE('',*,*,#8295,.T.);
#10896=ORIENTED_EDGE('',*,*,#8291,.F.);
#10897=ORIENTED_EDGE('',*,*,#8296,.F.);
#10898=ORIENTED_EDGE('',*,*,#8297,.T.);
#10899=ORIENTED_EDGE('',*,*,#8298,.T.);
#10900=ORIENTED_EDGE('',*,*,#8294,.F.);
#10901=ORIENTED_EDGE('',*,*,#8299,.F.);
#10902=ORIENTED_EDGE('',*,*,#8300,.T.);
#10903=ORIENTED_EDGE('',*,*,#8301,.T.);
#10904=ORIENTED_EDGE('',*,*,#8297,.F.);
#10905=ORIENTED_EDGE('',*,*,#8302,.F.);
#10906=ORIENTED_EDGE('',*,*,#8303,.T.);
#10907=ORIENTED_EDGE('',*,*,#8304,.T.);
#10908=ORIENTED_EDGE('',*,*,#8300,.F.);
#10909=ORIENTED_EDGE('',*,*,#8305,.F.);
#10910=ORIENTED_EDGE('',*,*,#8306,.T.);
#10911=ORIENTED_EDGE('',*,*,#8307,.T.);
#10912=ORIENTED_EDGE('',*,*,#8303,.F.);
#10913=ORIENTED_EDGE('',*,*,#8308,.F.);
#10914=ORIENTED_EDGE('',*,*,#8309,.T.);
#10915=ORIENTED_EDGE('',*,*,#8310,.T.);
#10916=ORIENTED_EDGE('',*,*,#8306,.F.);
#10917=ORIENTED_EDGE('',*,*,#8311,.F.);
#10918=ORIENTED_EDGE('',*,*,#8312,.T.);
#10919=ORIENTED_EDGE('',*,*,#8313,.T.);
#10920=ORIENTED_EDGE('',*,*,#8309,.F.);
#10921=ORIENTED_EDGE('',*,*,#8314,.F.);
#10922=ORIENTED_EDGE('',*,*,#8315,.T.);
#10923=ORIENTED_EDGE('',*,*,#8316,.T.);
#10924=ORIENTED_EDGE('',*,*,#8312,.F.);
#10925=ORIENTED_EDGE('',*,*,#8317,.F.);
#10926=ORIENTED_EDGE('',*,*,#8318,.T.);
#10927=ORIENTED_EDGE('',*,*,#8319,.T.);
#10928=ORIENTED_EDGE('',*,*,#8315,.F.);
#10929=ORIENTED_EDGE('',*,*,#8320,.F.);
#10930=ORIENTED_EDGE('',*,*,#8321,.T.);
#10931=ORIENTED_EDGE('',*,*,#8322,.T.);
#10932=ORIENTED_EDGE('',*,*,#8318,.F.);
#10933=ORIENTED_EDGE('',*,*,#8323,.F.);
#10934=ORIENTED_EDGE('',*,*,#8324,.F.);
#10935=ORIENTED_EDGE('',*,*,#8325,.F.);
#10936=ORIENTED_EDGE('',*,*,#8326,.F.);
#10937=ORIENTED_EDGE('',*,*,#8327,.T.);
#10938=ORIENTED_EDGE('',*,*,#8328,.T.);
#10939=ORIENTED_EDGE('',*,*,#8329,.T.);
#10940=ORIENTED_EDGE('',*,*,#8330,.T.);
#10941=ORIENTED_EDGE('',*,*,#8331,.T.);
#10942=ORIENTED_EDGE('',*,*,#8332,.T.);
#10943=ORIENTED_EDGE('',*,*,#8331,.F.);
#10944=ORIENTED_EDGE('',*,*,#8333,.T.);
#10945=ORIENTED_EDGE('',*,*,#8334,.T.);
#10946=ORIENTED_EDGE('',*,*,#8335,.T.);
#10947=ORIENTED_EDGE('',*,*,#8336,.T.);
#10948=ORIENTED_EDGE('',*,*,#8328,.F.);
#10949=ORIENTED_EDGE('',*,*,#8337,.T.);
#10950=ORIENTED_EDGE('',*,*,#8338,.T.);
#10951=ORIENTED_EDGE('',*,*,#8339,.T.);
#10952=ORIENTED_EDGE('',*,*,#8335,.F.);
#10953=ORIENTED_EDGE('',*,*,#8340,.T.);
#10954=ORIENTED_EDGE('',*,*,#8341,.T.);
#10955=ORIENTED_EDGE('',*,*,#8342,.T.);
#10956=ORIENTED_EDGE('',*,*,#8338,.F.);
#10957=ORIENTED_EDGE('',*,*,#8343,.T.);
#10958=ORIENTED_EDGE('',*,*,#8344,.T.);
#10959=ORIENTED_EDGE('',*,*,#8345,.T.);
#10960=ORIENTED_EDGE('',*,*,#8341,.F.);
#10961=ORIENTED_EDGE('',*,*,#8346,.T.);
#10962=ORIENTED_EDGE('',*,*,#8347,.T.);
#10963=ORIENTED_EDGE('',*,*,#8348,.T.);
#10964=ORIENTED_EDGE('',*,*,#8344,.F.);
#10965=ORIENTED_EDGE('',*,*,#8349,.T.);
#10966=ORIENTED_EDGE('',*,*,#8350,.T.);
#10967=ORIENTED_EDGE('',*,*,#8351,.T.);
#10968=ORIENTED_EDGE('',*,*,#8347,.F.);
#10969=ORIENTED_EDGE('',*,*,#8352,.T.);
#10970=ORIENTED_EDGE('',*,*,#8353,.T.);
#10971=ORIENTED_EDGE('',*,*,#8354,.T.);
#10972=ORIENTED_EDGE('',*,*,#8350,.F.);
#10973=ORIENTED_EDGE('',*,*,#8355,.T.);
#10974=ORIENTED_EDGE('',*,*,#8356,.T.);
#10975=ORIENTED_EDGE('',*,*,#8357,.T.);
#10976=ORIENTED_EDGE('',*,*,#8353,.F.);
#10977=ORIENTED_EDGE('',*,*,#8358,.T.);
#10978=ORIENTED_EDGE('',*,*,#8359,.T.);
#10979=ORIENTED_EDGE('',*,*,#8360,.T.);
#10980=ORIENTED_EDGE('',*,*,#8356,.F.);
#10981=ORIENTED_EDGE('',*,*,#8361,.T.);
#10982=ORIENTED_EDGE('',*,*,#8362,.T.);
#10983=ORIENTED_EDGE('',*,*,#8363,.T.);
#10984=ORIENTED_EDGE('',*,*,#8359,.F.);
#10985=ORIENTED_EDGE('',*,*,#8364,.T.);
#10986=ORIENTED_EDGE('',*,*,#8365,.T.);
#10987=ORIENTED_EDGE('',*,*,#8366,.T.);
#10988=ORIENTED_EDGE('',*,*,#8362,.F.);
#10989=ORIENTED_EDGE('',*,*,#8367,.T.);
#10990=ORIENTED_EDGE('',*,*,#8368,.T.);
#10991=ORIENTED_EDGE('',*,*,#8369,.T.);
#10992=ORIENTED_EDGE('',*,*,#8365,.F.);
#10993=ORIENTED_EDGE('',*,*,#8370,.T.);
#10994=ORIENTED_EDGE('',*,*,#8371,.T.);
#10995=ORIENTED_EDGE('',*,*,#8372,.T.);
#10996=ORIENTED_EDGE('',*,*,#8368,.F.);
#10997=ORIENTED_EDGE('',*,*,#8373,.T.);
#10998=ORIENTED_EDGE('',*,*,#8374,.T.);
#10999=ORIENTED_EDGE('',*,*,#8375,.T.);
#11000=ORIENTED_EDGE('',*,*,#8371,.F.);
#11001=ORIENTED_EDGE('',*,*,#8376,.T.);
#11002=ORIENTED_EDGE('',*,*,#8377,.T.);
#11003=ORIENTED_EDGE('',*,*,#8378,.T.);
#11004=ORIENTED_EDGE('',*,*,#8374,.F.);
#11005=ORIENTED_EDGE('',*,*,#8379,.T.);
#11006=ORIENTED_EDGE('',*,*,#8380,.T.);
#11007=ORIENTED_EDGE('',*,*,#8381,.T.);
#11008=ORIENTED_EDGE('',*,*,#8377,.F.);
#11009=ORIENTED_EDGE('',*,*,#8382,.T.);
#11010=ORIENTED_EDGE('',*,*,#8383,.F.);
#11011=ORIENTED_EDGE('',*,*,#8384,.T.);
#11012=ORIENTED_EDGE('',*,*,#8385,.F.);
#11013=ORIENTED_EDGE('',*,*,#8386,.T.);
#11014=ORIENTED_EDGE('',*,*,#8387,.T.);
#11015=ORIENTED_EDGE('',*,*,#8388,.T.);
#11016=ORIENTED_EDGE('',*,*,#8389,.F.);
#11017=ORIENTED_EDGE('',*,*,#8390,.F.);
#11018=ORIENTED_EDGE('',*,*,#8391,.T.);
#11019=ORIENTED_EDGE('',*,*,#8392,.T.);
#11020=ORIENTED_EDGE('',*,*,#8387,.F.);
#11021=ORIENTED_EDGE('',*,*,#8393,.F.);
#11022=ORIENTED_EDGE('',*,*,#8394,.T.);
#11023=ORIENTED_EDGE('',*,*,#8395,.T.);
#11024=ORIENTED_EDGE('',*,*,#8391,.F.);
#11025=ORIENTED_EDGE('',*,*,#8396,.F.);
#11026=ORIENTED_EDGE('',*,*,#8397,.T.);
#11027=ORIENTED_EDGE('',*,*,#8398,.T.);
#11028=ORIENTED_EDGE('',*,*,#8394,.F.);
#11029=ORIENTED_EDGE('',*,*,#8399,.F.);
#11030=ORIENTED_EDGE('',*,*,#8400,.T.);
#11031=ORIENTED_EDGE('',*,*,#8401,.T.);
#11032=ORIENTED_EDGE('',*,*,#8397,.F.);
#11033=ORIENTED_EDGE('',*,*,#8402,.F.);
#11034=ORIENTED_EDGE('',*,*,#8403,.T.);
#11035=ORIENTED_EDGE('',*,*,#8404,.T.);
#11036=ORIENTED_EDGE('',*,*,#8400,.F.);
#11037=ORIENTED_EDGE('',*,*,#8405,.F.);
#11038=ORIENTED_EDGE('',*,*,#8406,.T.);
#11039=ORIENTED_EDGE('',*,*,#8407,.T.);
#11040=ORIENTED_EDGE('',*,*,#8403,.F.);
#11041=ORIENTED_EDGE('',*,*,#8408,.F.);
#11042=ORIENTED_EDGE('',*,*,#8409,.T.);
#11043=ORIENTED_EDGE('',*,*,#8410,.T.);
#11044=ORIENTED_EDGE('',*,*,#8406,.F.);
#11045=ORIENTED_EDGE('',*,*,#8411,.F.);
#11046=ORIENTED_EDGE('',*,*,#8412,.T.);
#11047=ORIENTED_EDGE('',*,*,#8413,.T.);
#11048=ORIENTED_EDGE('',*,*,#8409,.F.);
#11049=ORIENTED_EDGE('',*,*,#8414,.F.);
#11050=ORIENTED_EDGE('',*,*,#8415,.T.);
#11051=ORIENTED_EDGE('',*,*,#8416,.T.);
#11052=ORIENTED_EDGE('',*,*,#8412,.F.);
#11053=ORIENTED_EDGE('',*,*,#8417,.F.);
#11054=ORIENTED_EDGE('',*,*,#8418,.T.);
#11055=ORIENTED_EDGE('',*,*,#8419,.T.);
#11056=ORIENTED_EDGE('',*,*,#8415,.F.);
#11057=ORIENTED_EDGE('',*,*,#8420,.F.);
#11058=ORIENTED_EDGE('',*,*,#8421,.T.);
#11059=ORIENTED_EDGE('',*,*,#8422,.T.);
#11060=ORIENTED_EDGE('',*,*,#8418,.F.);
#11061=ORIENTED_EDGE('',*,*,#8423,.F.);
#11062=ORIENTED_EDGE('',*,*,#8424,.T.);
#11063=ORIENTED_EDGE('',*,*,#8425,.T.);
#11064=ORIENTED_EDGE('',*,*,#8421,.F.);
#11065=ORIENTED_EDGE('',*,*,#8426,.F.);
#11066=ORIENTED_EDGE('',*,*,#8427,.T.);
#11067=ORIENTED_EDGE('',*,*,#8428,.T.);
#11068=ORIENTED_EDGE('',*,*,#8424,.F.);
#11069=ORIENTED_EDGE('',*,*,#8429,.F.);
#11070=ORIENTED_EDGE('',*,*,#8430,.T.);
#11071=ORIENTED_EDGE('',*,*,#8431,.T.);
#11072=ORIENTED_EDGE('',*,*,#8427,.F.);
#11073=ORIENTED_EDGE('',*,*,#8432,.F.);
#11074=ORIENTED_EDGE('',*,*,#8433,.T.);
#11075=ORIENTED_EDGE('',*,*,#8434,.T.);
#11076=ORIENTED_EDGE('',*,*,#8430,.F.);
#11077=ORIENTED_EDGE('',*,*,#8435,.F.);
#11078=ORIENTED_EDGE('',*,*,#8436,.T.);
#11079=ORIENTED_EDGE('',*,*,#8437,.T.);
#11080=ORIENTED_EDGE('',*,*,#8433,.F.);
#11081=ORIENTED_EDGE('',*,*,#8438,.F.);
#11082=ORIENTED_EDGE('',*,*,#8439,.T.);
#11083=ORIENTED_EDGE('',*,*,#8440,.T.);
#11084=ORIENTED_EDGE('',*,*,#8436,.F.);
#11085=ORIENTED_EDGE('',*,*,#8441,.F.);
#11086=ORIENTED_EDGE('',*,*,#8442,.F.);
#11087=ORIENTED_EDGE('',*,*,#8443,.F.);
#11088=ORIENTED_EDGE('',*,*,#8444,.F.);
#11089=ORIENTED_EDGE('',*,*,#8445,.T.);
#11090=ORIENTED_EDGE('',*,*,#8446,.T.);
#11091=ORIENTED_EDGE('',*,*,#8447,.T.);
#11092=ORIENTED_EDGE('',*,*,#8448,.T.);
#11093=ORIENTED_EDGE('',*,*,#8449,.T.);
#11094=ORIENTED_EDGE('',*,*,#8450,.T.);
#11095=ORIENTED_EDGE('',*,*,#8449,.F.);
#11096=ORIENTED_EDGE('',*,*,#8451,.T.);
#11097=ORIENTED_EDGE('',*,*,#8452,.T.);
#11098=ORIENTED_EDGE('',*,*,#8453,.T.);
#11099=ORIENTED_EDGE('',*,*,#8454,.T.);
#11100=ORIENTED_EDGE('',*,*,#8446,.F.);
#11101=ORIENTED_EDGE('',*,*,#8455,.T.);
#11102=ORIENTED_EDGE('',*,*,#8456,.T.);
#11103=ORIENTED_EDGE('',*,*,#8457,.T.);
#11104=ORIENTED_EDGE('',*,*,#8453,.F.);
#11105=ORIENTED_EDGE('',*,*,#8458,.T.);
#11106=ORIENTED_EDGE('',*,*,#8459,.T.);
#11107=ORIENTED_EDGE('',*,*,#8460,.T.);
#11108=ORIENTED_EDGE('',*,*,#8456,.F.);
#11109=ORIENTED_EDGE('',*,*,#8461,.T.);
#11110=ORIENTED_EDGE('',*,*,#8462,.T.);
#11111=ORIENTED_EDGE('',*,*,#8463,.T.);
#11112=ORIENTED_EDGE('',*,*,#8459,.F.);
#11113=ORIENTED_EDGE('',*,*,#8464,.T.);
#11114=ORIENTED_EDGE('',*,*,#8465,.T.);
#11115=ORIENTED_EDGE('',*,*,#8466,.T.);
#11116=ORIENTED_EDGE('',*,*,#8462,.F.);
#11117=ORIENTED_EDGE('',*,*,#8467,.T.);
#11118=ORIENTED_EDGE('',*,*,#8468,.T.);
#11119=ORIENTED_EDGE('',*,*,#8469,.T.);
#11120=ORIENTED_EDGE('',*,*,#8465,.F.);
#11121=ORIENTED_EDGE('',*,*,#8470,.T.);
#11122=ORIENTED_EDGE('',*,*,#8471,.T.);
#11123=ORIENTED_EDGE('',*,*,#8472,.T.);
#11124=ORIENTED_EDGE('',*,*,#8468,.F.);
#11125=ORIENTED_EDGE('',*,*,#8473,.T.);
#11126=ORIENTED_EDGE('',*,*,#8474,.T.);
#11127=ORIENTED_EDGE('',*,*,#8475,.T.);
#11128=ORIENTED_EDGE('',*,*,#8471,.F.);
#11129=ORIENTED_EDGE('',*,*,#8476,.T.);
#11130=ORIENTED_EDGE('',*,*,#8477,.T.);
#11131=ORIENTED_EDGE('',*,*,#8478,.T.);
#11132=ORIENTED_EDGE('',*,*,#8474,.F.);
#11133=ORIENTED_EDGE('',*,*,#8479,.T.);
#11134=ORIENTED_EDGE('',*,*,#8480,.T.);
#11135=ORIENTED_EDGE('',*,*,#8481,.T.);
#11136=ORIENTED_EDGE('',*,*,#8477,.F.);
#11137=ORIENTED_EDGE('',*,*,#8482,.T.);
#11138=ORIENTED_EDGE('',*,*,#8483,.T.);
#11139=ORIENTED_EDGE('',*,*,#8484,.T.);
#11140=ORIENTED_EDGE('',*,*,#8480,.F.);
#11141=ORIENTED_EDGE('',*,*,#8485,.T.);
#11142=ORIENTED_EDGE('',*,*,#8486,.T.);
#11143=ORIENTED_EDGE('',*,*,#8487,.T.);
#11144=ORIENTED_EDGE('',*,*,#8483,.F.);
#11145=ORIENTED_EDGE('',*,*,#8488,.T.);
#11146=ORIENTED_EDGE('',*,*,#8489,.T.);
#11147=ORIENTED_EDGE('',*,*,#8490,.T.);
#11148=ORIENTED_EDGE('',*,*,#8486,.F.);
#11149=ORIENTED_EDGE('',*,*,#8491,.T.);
#11150=ORIENTED_EDGE('',*,*,#8492,.T.);
#11151=ORIENTED_EDGE('',*,*,#8493,.T.);
#11152=ORIENTED_EDGE('',*,*,#8489,.F.);
#11153=ORIENTED_EDGE('',*,*,#8494,.T.);
#11154=ORIENTED_EDGE('',*,*,#8495,.T.);
#11155=ORIENTED_EDGE('',*,*,#8496,.T.);
#11156=ORIENTED_EDGE('',*,*,#8492,.F.);
#11157=ORIENTED_EDGE('',*,*,#8497,.T.);
#11158=ORIENTED_EDGE('',*,*,#8498,.T.);
#11159=ORIENTED_EDGE('',*,*,#8499,.T.);
#11160=ORIENTED_EDGE('',*,*,#8495,.F.);
#11161=ORIENTED_EDGE('',*,*,#8500,.T.);
#11162=ORIENTED_EDGE('',*,*,#8501,.F.);
#11163=ORIENTED_EDGE('',*,*,#8502,.T.);
#11164=ORIENTED_EDGE('',*,*,#8503,.F.);
#11165=ORIENTED_EDGE('',*,*,#8504,.T.);
#11166=ORIENTED_EDGE('',*,*,#8505,.T.);
#11167=ORIENTED_EDGE('',*,*,#8506,.T.);
#11168=ORIENTED_EDGE('',*,*,#8507,.F.);
#11169=ORIENTED_EDGE('',*,*,#8508,.F.);
#11170=ORIENTED_EDGE('',*,*,#8509,.T.);
#11171=ORIENTED_EDGE('',*,*,#8510,.T.);
#11172=ORIENTED_EDGE('',*,*,#8505,.F.);
#11173=ORIENTED_EDGE('',*,*,#8511,.F.);
#11174=ORIENTED_EDGE('',*,*,#8512,.T.);
#11175=ORIENTED_EDGE('',*,*,#8513,.T.);
#11176=ORIENTED_EDGE('',*,*,#8509,.F.);
#11177=ORIENTED_EDGE('',*,*,#8514,.F.);
#11178=ORIENTED_EDGE('',*,*,#8515,.T.);
#11179=ORIENTED_EDGE('',*,*,#8516,.T.);
#11180=ORIENTED_EDGE('',*,*,#8512,.F.);
#11181=ORIENTED_EDGE('',*,*,#8517,.F.);
#11182=ORIENTED_EDGE('',*,*,#8518,.T.);
#11183=ORIENTED_EDGE('',*,*,#8519,.T.);
#11184=ORIENTED_EDGE('',*,*,#8515,.F.);
#11185=ORIENTED_EDGE('',*,*,#8520,.F.);
#11186=ORIENTED_EDGE('',*,*,#8521,.T.);
#11187=ORIENTED_EDGE('',*,*,#8522,.T.);
#11188=ORIENTED_EDGE('',*,*,#8518,.F.);
#11189=ORIENTED_EDGE('',*,*,#8523,.F.);
#11190=ORIENTED_EDGE('',*,*,#8524,.T.);
#11191=ORIENTED_EDGE('',*,*,#8525,.T.);
#11192=ORIENTED_EDGE('',*,*,#8521,.F.);
#11193=ORIENTED_EDGE('',*,*,#8526,.F.);
#11194=ORIENTED_EDGE('',*,*,#8527,.T.);
#11195=ORIENTED_EDGE('',*,*,#8528,.T.);
#11196=ORIENTED_EDGE('',*,*,#8524,.F.);
#11197=ORIENTED_EDGE('',*,*,#8529,.F.);
#11198=ORIENTED_EDGE('',*,*,#8530,.T.);
#11199=ORIENTED_EDGE('',*,*,#8531,.T.);
#11200=ORIENTED_EDGE('',*,*,#8527,.F.);
#11201=ORIENTED_EDGE('',*,*,#8532,.F.);
#11202=ORIENTED_EDGE('',*,*,#8533,.T.);
#11203=ORIENTED_EDGE('',*,*,#8534,.T.);
#11204=ORIENTED_EDGE('',*,*,#8530,.F.);
#11205=ORIENTED_EDGE('',*,*,#8535,.F.);
#11206=ORIENTED_EDGE('',*,*,#8536,.T.);
#11207=ORIENTED_EDGE('',*,*,#8537,.T.);
#11208=ORIENTED_EDGE('',*,*,#8533,.F.);
#11209=ORIENTED_EDGE('',*,*,#8538,.F.);
#11210=ORIENTED_EDGE('',*,*,#8539,.T.);
#11211=ORIENTED_EDGE('',*,*,#8540,.T.);
#11212=ORIENTED_EDGE('',*,*,#8536,.F.);
#11213=ORIENTED_EDGE('',*,*,#8541,.F.);
#11214=ORIENTED_EDGE('',*,*,#8542,.T.);
#11215=ORIENTED_EDGE('',*,*,#8543,.T.);
#11216=ORIENTED_EDGE('',*,*,#8539,.F.);
#11217=ORIENTED_EDGE('',*,*,#8544,.F.);
#11218=ORIENTED_EDGE('',*,*,#8545,.T.);
#11219=ORIENTED_EDGE('',*,*,#8546,.T.);
#11220=ORIENTED_EDGE('',*,*,#8542,.F.);
#11221=ORIENTED_EDGE('',*,*,#8547,.F.);
#11222=ORIENTED_EDGE('',*,*,#8548,.T.);
#11223=ORIENTED_EDGE('',*,*,#8549,.T.);
#11224=ORIENTED_EDGE('',*,*,#8545,.F.);
#11225=ORIENTED_EDGE('',*,*,#8550,.F.);
#11226=ORIENTED_EDGE('',*,*,#8551,.T.);
#11227=ORIENTED_EDGE('',*,*,#8552,.T.);
#11228=ORIENTED_EDGE('',*,*,#8548,.F.);
#11229=ORIENTED_EDGE('',*,*,#8553,.F.);
#11230=ORIENTED_EDGE('',*,*,#8554,.T.);
#11231=ORIENTED_EDGE('',*,*,#8555,.T.);
#11232=ORIENTED_EDGE('',*,*,#8551,.F.);
#11233=ORIENTED_EDGE('',*,*,#8556,.F.);
#11234=ORIENTED_EDGE('',*,*,#8557,.T.);
#11235=ORIENTED_EDGE('',*,*,#8558,.T.);
#11236=ORIENTED_EDGE('',*,*,#8554,.F.);
#11237=ORIENTED_EDGE('',*,*,#8559,.F.);
#11238=ORIENTED_EDGE('',*,*,#8560,.F.);
#11239=ORIENTED_EDGE('',*,*,#8561,.F.);
#11240=ORIENTED_EDGE('',*,*,#8562,.F.);
#11241=ORIENTED_EDGE('',*,*,#8563,.T.);
#11242=ORIENTED_EDGE('',*,*,#8448,.F.);
#11243=ORIENTED_EDGE('',*,*,#8564,.T.);
#11244=ORIENTED_EDGE('',*,*,#8507,.T.);
#11245=ORIENTED_EDGE('',*,*,#8565,.T.);
#11246=ORIENTED_EDGE('',*,*,#8451,.F.);
#11247=ORIENTED_EDGE('',*,*,#8560,.T.);
#11248=ORIENTED_EDGE('',*,*,#8566,.T.);
#11249=ORIENTED_EDGE('',*,*,#8557,.F.);
#11250=ORIENTED_EDGE('',*,*,#8567,.F.);
#11251=ORIENTED_EDGE('',*,*,#8565,.F.);
#11252=ORIENTED_EDGE('',*,*,#8506,.F.);
#11253=ORIENTED_EDGE('',*,*,#8510,.F.);
#11254=ORIENTED_EDGE('',*,*,#8513,.F.);
#11255=ORIENTED_EDGE('',*,*,#8516,.F.);
#11256=ORIENTED_EDGE('',*,*,#8519,.F.);
#11257=ORIENTED_EDGE('',*,*,#8522,.F.);
#11258=ORIENTED_EDGE('',*,*,#8525,.F.);
#11259=ORIENTED_EDGE('',*,*,#8528,.F.);
#11260=ORIENTED_EDGE('',*,*,#8531,.F.);
#11261=ORIENTED_EDGE('',*,*,#8534,.F.);
#11262=ORIENTED_EDGE('',*,*,#8537,.F.);
#11263=ORIENTED_EDGE('',*,*,#8540,.F.);
#11264=ORIENTED_EDGE('',*,*,#8543,.F.);
#11265=ORIENTED_EDGE('',*,*,#8546,.F.);
#11266=ORIENTED_EDGE('',*,*,#8549,.F.);
#11267=ORIENTED_EDGE('',*,*,#8552,.F.);
#11268=ORIENTED_EDGE('',*,*,#8555,.F.);
#11269=ORIENTED_EDGE('',*,*,#8558,.F.);
#11270=ORIENTED_EDGE('',*,*,#8566,.F.);
#11271=ORIENTED_EDGE('',*,*,#8563,.F.);
#11272=ORIENTED_EDGE('',*,*,#8568,.F.);
#11273=ORIENTED_EDGE('',*,*,#8502,.F.);
#11274=ORIENTED_EDGE('',*,*,#8569,.F.);
#11275=ORIENTED_EDGE('',*,*,#8500,.F.);
#11276=ORIENTED_EDGE('',*,*,#8497,.F.);
#11277=ORIENTED_EDGE('',*,*,#8494,.F.);
#11278=ORIENTED_EDGE('',*,*,#8491,.F.);
#11279=ORIENTED_EDGE('',*,*,#8488,.F.);
#11280=ORIENTED_EDGE('',*,*,#8485,.F.);
#11281=ORIENTED_EDGE('',*,*,#8482,.F.);
#11282=ORIENTED_EDGE('',*,*,#8479,.F.);
#11283=ORIENTED_EDGE('',*,*,#8476,.F.);
#11284=ORIENTED_EDGE('',*,*,#8473,.F.);
#11285=ORIENTED_EDGE('',*,*,#8470,.F.);
#11286=ORIENTED_EDGE('',*,*,#8467,.F.);
#11287=ORIENTED_EDGE('',*,*,#8464,.F.);
#11288=ORIENTED_EDGE('',*,*,#8461,.F.);
#11289=ORIENTED_EDGE('',*,*,#8458,.F.);
#11290=ORIENTED_EDGE('',*,*,#8455,.F.);
#11291=ORIENTED_EDGE('',*,*,#8452,.F.);
#11292=ORIENTED_EDGE('',*,*,#8564,.F.);
#11293=ORIENTED_EDGE('',*,*,#8447,.F.);
#11294=ORIENTED_EDGE('',*,*,#8454,.F.);
#11295=ORIENTED_EDGE('',*,*,#8457,.F.);
#11296=ORIENTED_EDGE('',*,*,#8460,.F.);
#11297=ORIENTED_EDGE('',*,*,#8463,.F.);
#11298=ORIENTED_EDGE('',*,*,#8466,.F.);
#11299=ORIENTED_EDGE('',*,*,#8469,.F.);
#11300=ORIENTED_EDGE('',*,*,#8472,.F.);
#11301=ORIENTED_EDGE('',*,*,#8475,.F.);
#11302=ORIENTED_EDGE('',*,*,#8478,.F.);
#11303=ORIENTED_EDGE('',*,*,#8481,.F.);
#11304=ORIENTED_EDGE('',*,*,#8484,.F.);
#11305=ORIENTED_EDGE('',*,*,#8487,.F.);
#11306=ORIENTED_EDGE('',*,*,#8490,.F.);
#11307=ORIENTED_EDGE('',*,*,#8493,.F.);
#11308=ORIENTED_EDGE('',*,*,#8496,.F.);
#11309=ORIENTED_EDGE('',*,*,#8499,.F.);
#11310=ORIENTED_EDGE('',*,*,#8570,.F.);
#11311=ORIENTED_EDGE('',*,*,#8504,.F.);
#11312=ORIENTED_EDGE('',*,*,#8571,.F.);
#11313=ORIENTED_EDGE('',*,*,#8561,.T.);
#11314=ORIENTED_EDGE('',*,*,#8567,.T.);
#11315=ORIENTED_EDGE('',*,*,#8559,.T.);
#11316=ORIENTED_EDGE('',*,*,#8556,.T.);
#11317=ORIENTED_EDGE('',*,*,#8553,.T.);
#11318=ORIENTED_EDGE('',*,*,#8550,.T.);
#11319=ORIENTED_EDGE('',*,*,#8547,.T.);
#11320=ORIENTED_EDGE('',*,*,#8544,.T.);
#11321=ORIENTED_EDGE('',*,*,#8541,.T.);
#11322=ORIENTED_EDGE('',*,*,#8538,.T.);
#11323=ORIENTED_EDGE('',*,*,#8535,.T.);
#11324=ORIENTED_EDGE('',*,*,#8532,.T.);
#11325=ORIENTED_EDGE('',*,*,#8529,.T.);
#11326=ORIENTED_EDGE('',*,*,#8526,.T.);
#11327=ORIENTED_EDGE('',*,*,#8523,.T.);
#11328=ORIENTED_EDGE('',*,*,#8520,.T.);
#11329=ORIENTED_EDGE('',*,*,#8517,.T.);
#11330=ORIENTED_EDGE('',*,*,#8514,.T.);
#11331=ORIENTED_EDGE('',*,*,#8511,.T.);
#11332=ORIENTED_EDGE('',*,*,#8508,.T.);
#11333=ORIENTED_EDGE('',*,*,#8501,.T.);
#11334=ORIENTED_EDGE('',*,*,#8570,.T.);
#11335=ORIENTED_EDGE('',*,*,#8498,.F.);
#11336=ORIENTED_EDGE('',*,*,#8569,.T.);
#11337=ORIENTED_EDGE('',*,*,#8330,.F.);
#11338=ORIENTED_EDGE('',*,*,#8572,.T.);
#11339=ORIENTED_EDGE('',*,*,#8389,.T.);
#11340=ORIENTED_EDGE('',*,*,#8573,.T.);
#11341=ORIENTED_EDGE('',*,*,#8333,.F.);
#11342=ORIENTED_EDGE('',*,*,#8442,.T.);
#11343=ORIENTED_EDGE('',*,*,#8574,.T.);
#11344=ORIENTED_EDGE('',*,*,#8439,.F.);
#11345=ORIENTED_EDGE('',*,*,#8575,.F.);
#11346=ORIENTED_EDGE('',*,*,#8573,.F.);
#11347=ORIENTED_EDGE('',*,*,#8388,.F.);
#11348=ORIENTED_EDGE('',*,*,#8392,.F.);
#11349=ORIENTED_EDGE('',*,*,#8395,.F.);
#11350=ORIENTED_EDGE('',*,*,#8398,.F.);
#11351=ORIENTED_EDGE('',*,*,#8401,.F.);
#11352=ORIENTED_EDGE('',*,*,#8404,.F.);
#11353=ORIENTED_EDGE('',*,*,#8407,.F.);
#11354=ORIENTED_EDGE('',*,*,#8410,.F.);
#11355=ORIENTED_EDGE('',*,*,#8413,.F.);
#11356=ORIENTED_EDGE('',*,*,#8416,.F.);
#11357=ORIENTED_EDGE('',*,*,#8419,.F.);
#11358=ORIENTED_EDGE('',*,*,#8422,.F.);
#11359=ORIENTED_EDGE('',*,*,#8425,.F.);
#11360=ORIENTED_EDGE('',*,*,#8428,.F.);
#11361=ORIENTED_EDGE('',*,*,#8431,.F.);
#11362=ORIENTED_EDGE('',*,*,#8434,.F.);
#11363=ORIENTED_EDGE('',*,*,#8437,.F.);
#11364=ORIENTED_EDGE('',*,*,#8440,.F.);
#11365=ORIENTED_EDGE('',*,*,#8574,.F.);
#11366=ORIENTED_EDGE('',*,*,#8445,.F.);
#11367=ORIENTED_EDGE('',*,*,#8576,.F.);
#11368=ORIENTED_EDGE('',*,*,#8384,.F.);
#11369=ORIENTED_EDGE('',*,*,#8577,.F.);
#11370=ORIENTED_EDGE('',*,*,#8382,.F.);
#11371=ORIENTED_EDGE('',*,*,#8379,.F.);
#11372=ORIENTED_EDGE('',*,*,#8376,.F.);
#11373=ORIENTED_EDGE('',*,*,#8373,.F.);
#11374=ORIENTED_EDGE('',*,*,#8370,.F.);
#11375=ORIENTED_EDGE('',*,*,#8367,.F.);
#11376=ORIENTED_EDGE('',*,*,#8364,.F.);
#11377=ORIENTED_EDGE('',*,*,#8361,.F.);
#11378=ORIENTED_EDGE('',*,*,#8358,.F.);
#11379=ORIENTED_EDGE('',*,*,#8355,.F.);
#11380=ORIENTED_EDGE('',*,*,#8352,.F.);
#11381=ORIENTED_EDGE('',*,*,#8349,.F.);
#11382=ORIENTED_EDGE('',*,*,#8346,.F.);
#11383=ORIENTED_EDGE('',*,*,#8343,.F.);
#11384=ORIENTED_EDGE('',*,*,#8340,.F.);
#11385=ORIENTED_EDGE('',*,*,#8337,.F.);
#11386=ORIENTED_EDGE('',*,*,#8334,.F.);
#11387=ORIENTED_EDGE('',*,*,#8572,.F.);
#11388=ORIENTED_EDGE('',*,*,#8329,.F.);
#11389=ORIENTED_EDGE('',*,*,#8336,.F.);
#11390=ORIENTED_EDGE('',*,*,#8339,.F.);
#11391=ORIENTED_EDGE('',*,*,#8342,.F.);
#11392=ORIENTED_EDGE('',*,*,#8345,.F.);
#11393=ORIENTED_EDGE('',*,*,#8348,.F.);
#11394=ORIENTED_EDGE('',*,*,#8351,.F.);
#11395=ORIENTED_EDGE('',*,*,#8354,.F.);
#11396=ORIENTED_EDGE('',*,*,#8357,.F.);
#11397=ORIENTED_EDGE('',*,*,#8360,.F.);
#11398=ORIENTED_EDGE('',*,*,#8363,.F.);
#11399=ORIENTED_EDGE('',*,*,#8366,.F.);
#11400=ORIENTED_EDGE('',*,*,#8369,.F.);
#11401=ORIENTED_EDGE('',*,*,#8372,.F.);
#11402=ORIENTED_EDGE('',*,*,#8375,.F.);
#11403=ORIENTED_EDGE('',*,*,#8378,.F.);
#11404=ORIENTED_EDGE('',*,*,#8381,.F.);
#11405=ORIENTED_EDGE('',*,*,#8578,.F.);
#11406=ORIENTED_EDGE('',*,*,#8386,.F.);
#11407=ORIENTED_EDGE('',*,*,#8579,.F.);
#11408=ORIENTED_EDGE('',*,*,#8443,.T.);
#11409=ORIENTED_EDGE('',*,*,#8575,.T.);
#11410=ORIENTED_EDGE('',*,*,#8441,.T.);
#11411=ORIENTED_EDGE('',*,*,#8438,.T.);
#11412=ORIENTED_EDGE('',*,*,#8435,.T.);
#11413=ORIENTED_EDGE('',*,*,#8432,.T.);
#11414=ORIENTED_EDGE('',*,*,#8429,.T.);
#11415=ORIENTED_EDGE('',*,*,#8426,.T.);
#11416=ORIENTED_EDGE('',*,*,#8423,.T.);
#11417=ORIENTED_EDGE('',*,*,#8420,.T.);
#11418=ORIENTED_EDGE('',*,*,#8417,.T.);
#11419=ORIENTED_EDGE('',*,*,#8414,.T.);
#11420=ORIENTED_EDGE('',*,*,#8411,.T.);
#11421=ORIENTED_EDGE('',*,*,#8408,.T.);
#11422=ORIENTED_EDGE('',*,*,#8405,.T.);
#11423=ORIENTED_EDGE('',*,*,#8402,.T.);
#11424=ORIENTED_EDGE('',*,*,#8399,.T.);
#11425=ORIENTED_EDGE('',*,*,#8396,.T.);
#11426=ORIENTED_EDGE('',*,*,#8393,.T.);
#11427=ORIENTED_EDGE('',*,*,#8390,.T.);
#11428=ORIENTED_EDGE('',*,*,#8383,.T.);
#11429=ORIENTED_EDGE('',*,*,#8578,.T.);
#11430=ORIENTED_EDGE('',*,*,#8380,.F.);
#11431=ORIENTED_EDGE('',*,*,#8577,.T.);
#11432=ORIENTED_EDGE('',*,*,#8212,.F.);
#11433=ORIENTED_EDGE('',*,*,#8580,.T.);
#11434=ORIENTED_EDGE('',*,*,#8271,.T.);
#11435=ORIENTED_EDGE('',*,*,#8581,.T.);
#11436=ORIENTED_EDGE('',*,*,#8215,.F.);
#11437=ORIENTED_EDGE('',*,*,#8324,.T.);
#11438=ORIENTED_EDGE('',*,*,#8582,.T.);
#11439=ORIENTED_EDGE('',*,*,#8321,.F.);
#11440=ORIENTED_EDGE('',*,*,#8583,.F.);
#11441=ORIENTED_EDGE('',*,*,#8581,.F.);
#11442=ORIENTED_EDGE('',*,*,#8270,.F.);
#11443=ORIENTED_EDGE('',*,*,#8274,.F.);
#11444=ORIENTED_EDGE('',*,*,#8277,.F.);
#11445=ORIENTED_EDGE('',*,*,#8280,.F.);
#11446=ORIENTED_EDGE('',*,*,#8283,.F.);
#11447=ORIENTED_EDGE('',*,*,#8286,.F.);
#11448=ORIENTED_EDGE('',*,*,#8289,.F.);
#11449=ORIENTED_EDGE('',*,*,#8292,.F.);
#11450=ORIENTED_EDGE('',*,*,#8295,.F.);
#11451=ORIENTED_EDGE('',*,*,#8298,.F.);
#11452=ORIENTED_EDGE('',*,*,#8301,.F.);
#11453=ORIENTED_EDGE('',*,*,#8304,.F.);
#11454=ORIENTED_EDGE('',*,*,#8307,.F.);
#11455=ORIENTED_EDGE('',*,*,#8310,.F.);
#11456=ORIENTED_EDGE('',*,*,#8313,.F.);
#11457=ORIENTED_EDGE('',*,*,#8316,.F.);
#11458=ORIENTED_EDGE('',*,*,#8319,.F.);
#11459=ORIENTED_EDGE('',*,*,#8322,.F.);
#11460=ORIENTED_EDGE('',*,*,#8582,.F.);
#11461=ORIENTED_EDGE('',*,*,#8327,.F.);
#11462=ORIENTED_EDGE('',*,*,#8584,.F.);
#11463=ORIENTED_EDGE('',*,*,#8266,.F.);
#11464=ORIENTED_EDGE('',*,*,#8585,.F.);
#11465=ORIENTED_EDGE('',*,*,#8264,.F.);
#11466=ORIENTED_EDGE('',*,*,#8261,.F.);
#11467=ORIENTED_EDGE('',*,*,#8258,.F.);
#11468=ORIENTED_EDGE('',*,*,#8255,.F.);
#11469=ORIENTED_EDGE('',*,*,#8252,.F.);
#11470=ORIENTED_EDGE('',*,*,#8249,.F.);
#11471=ORIENTED_EDGE('',*,*,#8246,.F.);
#11472=ORIENTED_EDGE('',*,*,#8243,.F.);
#11473=ORIENTED_EDGE('',*,*,#8240,.F.);
#11474=ORIENTED_EDGE('',*,*,#8237,.F.);
#11475=ORIENTED_EDGE('',*,*,#8234,.F.);
#11476=ORIENTED_EDGE('',*,*,#8231,.F.);
#11477=ORIENTED_EDGE('',*,*,#8228,.F.);
#11478=ORIENTED_EDGE('',*,*,#8225,.F.);
#11479=ORIENTED_EDGE('',*,*,#8222,.F.);
#11480=ORIENTED_EDGE('',*,*,#8219,.F.);
#11481=ORIENTED_EDGE('',*,*,#8216,.F.);
#11482=ORIENTED_EDGE('',*,*,#8580,.F.);
#11483=ORIENTED_EDGE('',*,*,#8211,.F.);
#11484=ORIENTED_EDGE('',*,*,#8218,.F.);
#11485=ORIENTED_EDGE('',*,*,#8221,.F.);
#11486=ORIENTED_EDGE('',*,*,#8224,.F.);
#11487=ORIENTED_EDGE('',*,*,#8227,.F.);
#11488=ORIENTED_EDGE('',*,*,#8230,.F.);
#11489=ORIENTED_EDGE('',*,*,#8233,.F.);
#11490=ORIENTED_EDGE('',*,*,#8236,.F.);
#11491=ORIENTED_EDGE('',*,*,#8239,.F.);
#11492=ORIENTED_EDGE('',*,*,#8242,.F.);
#11493=ORIENTED_EDGE('',*,*,#8245,.F.);
#11494=ORIENTED_EDGE('',*,*,#8248,.F.);
#11495=ORIENTED_EDGE('',*,*,#8251,.F.);
#11496=ORIENTED_EDGE('',*,*,#8254,.F.);
#11497=ORIENTED_EDGE('',*,*,#8257,.F.);
#11498=ORIENTED_EDGE('',*,*,#8260,.F.);
#11499=ORIENTED_EDGE('',*,*,#8263,.F.);
#11500=ORIENTED_EDGE('',*,*,#8586,.F.);
#11501=ORIENTED_EDGE('',*,*,#8268,.F.);
#11502=ORIENTED_EDGE('',*,*,#8587,.F.);
#11503=ORIENTED_EDGE('',*,*,#8325,.T.);
#11504=ORIENTED_EDGE('',*,*,#8583,.T.);
#11505=ORIENTED_EDGE('',*,*,#8323,.T.);
#11506=ORIENTED_EDGE('',*,*,#8320,.T.);
#11507=ORIENTED_EDGE('',*,*,#8317,.T.);
#11508=ORIENTED_EDGE('',*,*,#8314,.T.);
#11509=ORIENTED_EDGE('',*,*,#8311,.T.);
#11510=ORIENTED_EDGE('',*,*,#8308,.T.);
#11511=ORIENTED_EDGE('',*,*,#8305,.T.);
#11512=ORIENTED_EDGE('',*,*,#8302,.T.);
#11513=ORIENTED_EDGE('',*,*,#8299,.T.);
#11514=ORIENTED_EDGE('',*,*,#8296,.T.);
#11515=ORIENTED_EDGE('',*,*,#8293,.T.);
#11516=ORIENTED_EDGE('',*,*,#8290,.T.);
#11517=ORIENTED_EDGE('',*,*,#8287,.T.);
#11518=ORIENTED_EDGE('',*,*,#8284,.T.);
#11519=ORIENTED_EDGE('',*,*,#8281,.T.);
#11520=ORIENTED_EDGE('',*,*,#8278,.T.);
#11521=ORIENTED_EDGE('',*,*,#8275,.T.);
#11522=ORIENTED_EDGE('',*,*,#8272,.T.);
#11523=ORIENTED_EDGE('',*,*,#8265,.T.);
#11524=ORIENTED_EDGE('',*,*,#8586,.T.);
#11525=ORIENTED_EDGE('',*,*,#8262,.F.);
#11526=ORIENTED_EDGE('',*,*,#8585,.T.);
#11527=ORIENTED_EDGE('',*,*,#8094,.F.);
#11528=ORIENTED_EDGE('',*,*,#8588,.T.);
#11529=ORIENTED_EDGE('',*,*,#8153,.T.);
#11530=ORIENTED_EDGE('',*,*,#8589,.T.);
#11531=ORIENTED_EDGE('',*,*,#8097,.F.);
#11532=ORIENTED_EDGE('',*,*,#8206,.T.);
#11533=ORIENTED_EDGE('',*,*,#8590,.T.);
#11534=ORIENTED_EDGE('',*,*,#8203,.F.);
#11535=ORIENTED_EDGE('',*,*,#8591,.F.);
#11536=ORIENTED_EDGE('',*,*,#8589,.F.);
#11537=ORIENTED_EDGE('',*,*,#8152,.F.);
#11538=ORIENTED_EDGE('',*,*,#8156,.F.);
#11539=ORIENTED_EDGE('',*,*,#8159,.F.);
#11540=ORIENTED_EDGE('',*,*,#8162,.F.);
#11541=ORIENTED_EDGE('',*,*,#8165,.F.);
#11542=ORIENTED_EDGE('',*,*,#8168,.F.);
#11543=ORIENTED_EDGE('',*,*,#8171,.F.);
#11544=ORIENTED_EDGE('',*,*,#8174,.F.);
#11545=ORIENTED_EDGE('',*,*,#8177,.F.);
#11546=ORIENTED_EDGE('',*,*,#8180,.F.);
#11547=ORIENTED_EDGE('',*,*,#8183,.F.);
#11548=ORIENTED_EDGE('',*,*,#8186,.F.);
#11549=ORIENTED_EDGE('',*,*,#8189,.F.);
#11550=ORIENTED_EDGE('',*,*,#8192,.F.);
#11551=ORIENTED_EDGE('',*,*,#8195,.F.);
#11552=ORIENTED_EDGE('',*,*,#8198,.F.);
#11553=ORIENTED_EDGE('',*,*,#8201,.F.);
#11554=ORIENTED_EDGE('',*,*,#8204,.F.);
#11555=ORIENTED_EDGE('',*,*,#8590,.F.);
#11556=ORIENTED_EDGE('',*,*,#8209,.F.);
#11557=ORIENTED_EDGE('',*,*,#8592,.F.);
#11558=ORIENTED_EDGE('',*,*,#8148,.F.);
#11559=ORIENTED_EDGE('',*,*,#8593,.F.);
#11560=ORIENTED_EDGE('',*,*,#8146,.F.);
#11561=ORIENTED_EDGE('',*,*,#8143,.F.);
#11562=ORIENTED_EDGE('',*,*,#8140,.F.);
#11563=ORIENTED_EDGE('',*,*,#8137,.F.);
#11564=ORIENTED_EDGE('',*,*,#8134,.F.);
#11565=ORIENTED_EDGE('',*,*,#8131,.F.);
#11566=ORIENTED_EDGE('',*,*,#8128,.F.);
#11567=ORIENTED_EDGE('',*,*,#8125,.F.);
#11568=ORIENTED_EDGE('',*,*,#8122,.F.);
#11569=ORIENTED_EDGE('',*,*,#8119,.F.);
#11570=ORIENTED_EDGE('',*,*,#8116,.F.);
#11571=ORIENTED_EDGE('',*,*,#8113,.F.);
#11572=ORIENTED_EDGE('',*,*,#8110,.F.);
#11573=ORIENTED_EDGE('',*,*,#8107,.F.);
#11574=ORIENTED_EDGE('',*,*,#8104,.F.);
#11575=ORIENTED_EDGE('',*,*,#8101,.F.);
#11576=ORIENTED_EDGE('',*,*,#8098,.F.);
#11577=ORIENTED_EDGE('',*,*,#8588,.F.);
#11578=ORIENTED_EDGE('',*,*,#8093,.F.);
#11579=ORIENTED_EDGE('',*,*,#8100,.F.);
#11580=ORIENTED_EDGE('',*,*,#8103,.F.);
#11581=ORIENTED_EDGE('',*,*,#8106,.F.);
#11582=ORIENTED_EDGE('',*,*,#8109,.F.);
#11583=ORIENTED_EDGE('',*,*,#8112,.F.);
#11584=ORIENTED_EDGE('',*,*,#8115,.F.);
#11585=ORIENTED_EDGE('',*,*,#8118,.F.);
#11586=ORIENTED_EDGE('',*,*,#8121,.F.);
#11587=ORIENTED_EDGE('',*,*,#8124,.F.);
#11588=ORIENTED_EDGE('',*,*,#8127,.F.);
#11589=ORIENTED_EDGE('',*,*,#8130,.F.);
#11590=ORIENTED_EDGE('',*,*,#8133,.F.);
#11591=ORIENTED_EDGE('',*,*,#8136,.F.);
#11592=ORIENTED_EDGE('',*,*,#8139,.F.);
#11593=ORIENTED_EDGE('',*,*,#8142,.F.);
#11594=ORIENTED_EDGE('',*,*,#8145,.F.);
#11595=ORIENTED_EDGE('',*,*,#8594,.F.);
#11596=ORIENTED_EDGE('',*,*,#8150,.F.);
#11597=ORIENTED_EDGE('',*,*,#8595,.F.);
#11598=ORIENTED_EDGE('',*,*,#8207,.T.);
#11599=ORIENTED_EDGE('',*,*,#8591,.T.);
#11600=ORIENTED_EDGE('',*,*,#8205,.T.);
#11601=ORIENTED_EDGE('',*,*,#8202,.T.);
#11602=ORIENTED_EDGE('',*,*,#8199,.T.);
#11603=ORIENTED_EDGE('',*,*,#8196,.T.);
#11604=ORIENTED_EDGE('',*,*,#8193,.T.);
#11605=ORIENTED_EDGE('',*,*,#8190,.T.);
#11606=ORIENTED_EDGE('',*,*,#8187,.T.);
#11607=ORIENTED_EDGE('',*,*,#8184,.T.);
#11608=ORIENTED_EDGE('',*,*,#8181,.T.);
#11609=ORIENTED_EDGE('',*,*,#8178,.T.);
#11610=ORIENTED_EDGE('',*,*,#8175,.T.);
#11611=ORIENTED_EDGE('',*,*,#8172,.T.);
#11612=ORIENTED_EDGE('',*,*,#8169,.T.);
#11613=ORIENTED_EDGE('',*,*,#8166,.T.);
#11614=ORIENTED_EDGE('',*,*,#8163,.T.);
#11615=ORIENTED_EDGE('',*,*,#8160,.T.);
#11616=ORIENTED_EDGE('',*,*,#8157,.T.);
#11617=ORIENTED_EDGE('',*,*,#8154,.T.);
#11618=ORIENTED_EDGE('',*,*,#8147,.T.);
#11619=ORIENTED_EDGE('',*,*,#8594,.T.);
#11620=ORIENTED_EDGE('',*,*,#8144,.F.);
#11621=ORIENTED_EDGE('',*,*,#8593,.T.);
#11622=ORIENTED_EDGE('',*,*,#8096,.F.);
#11623=ORIENTED_EDGE('',*,*,#8332,.F.);
#11624=ORIENTED_EDGE('',*,*,#8214,.F.);
#11625=ORIENTED_EDGE('',*,*,#8450,.F.);
#11626=ORIENTED_EDGE('',*,*,#7976,.F.);
#11627=ORIENTED_EDGE('',*,*,#8596,.T.);
#11628=ORIENTED_EDGE('',*,*,#8035,.T.);
#11629=ORIENTED_EDGE('',*,*,#8597,.T.);
#11630=ORIENTED_EDGE('',*,*,#7979,.F.);
#11631=ORIENTED_EDGE('',*,*,#8088,.T.);
#11632=ORIENTED_EDGE('',*,*,#8598,.T.);
#11633=ORIENTED_EDGE('',*,*,#8085,.F.);
#11634=ORIENTED_EDGE('',*,*,#8599,.F.);
#11635=ORIENTED_EDGE('',*,*,#8597,.F.);
#11636=ORIENTED_EDGE('',*,*,#8034,.F.);
#11637=ORIENTED_EDGE('',*,*,#8038,.F.);
#11638=ORIENTED_EDGE('',*,*,#8041,.F.);
#11639=ORIENTED_EDGE('',*,*,#8044,.F.);
#11640=ORIENTED_EDGE('',*,*,#8047,.F.);
#11641=ORIENTED_EDGE('',*,*,#8050,.F.);
#11642=ORIENTED_EDGE('',*,*,#8053,.F.);
#11643=ORIENTED_EDGE('',*,*,#8056,.F.);
#11644=ORIENTED_EDGE('',*,*,#8059,.F.);
#11645=ORIENTED_EDGE('',*,*,#8062,.F.);
#11646=ORIENTED_EDGE('',*,*,#8065,.F.);
#11647=ORIENTED_EDGE('',*,*,#8068,.F.);
#11648=ORIENTED_EDGE('',*,*,#8071,.F.);
#11649=ORIENTED_EDGE('',*,*,#8074,.F.);
#11650=ORIENTED_EDGE('',*,*,#8077,.F.);
#11651=ORIENTED_EDGE('',*,*,#8080,.F.);
#11652=ORIENTED_EDGE('',*,*,#8083,.F.);
#11653=ORIENTED_EDGE('',*,*,#8086,.F.);
#11654=ORIENTED_EDGE('',*,*,#8598,.F.);
#11655=ORIENTED_EDGE('',*,*,#8091,.F.);
#11656=ORIENTED_EDGE('',*,*,#8600,.F.);
#11657=ORIENTED_EDGE('',*,*,#8030,.F.);
#11658=ORIENTED_EDGE('',*,*,#8601,.F.);
#11659=ORIENTED_EDGE('',*,*,#8028,.F.);
#11660=ORIENTED_EDGE('',*,*,#8025,.F.);
#11661=ORIENTED_EDGE('',*,*,#8022,.F.);
#11662=ORIENTED_EDGE('',*,*,#8019,.F.);
#11663=ORIENTED_EDGE('',*,*,#8016,.F.);
#11664=ORIENTED_EDGE('',*,*,#8013,.F.);
#11665=ORIENTED_EDGE('',*,*,#8010,.F.);
#11666=ORIENTED_EDGE('',*,*,#8007,.F.);
#11667=ORIENTED_EDGE('',*,*,#8004,.F.);
#11668=ORIENTED_EDGE('',*,*,#8001,.F.);
#11669=ORIENTED_EDGE('',*,*,#7998,.F.);
#11670=ORIENTED_EDGE('',*,*,#7995,.F.);
#11671=ORIENTED_EDGE('',*,*,#7992,.F.);
#11672=ORIENTED_EDGE('',*,*,#7989,.F.);
#11673=ORIENTED_EDGE('',*,*,#7986,.F.);
#11674=ORIENTED_EDGE('',*,*,#7983,.F.);
#11675=ORIENTED_EDGE('',*,*,#7980,.F.);
#11676=ORIENTED_EDGE('',*,*,#8596,.F.);
#11677=ORIENTED_EDGE('',*,*,#7975,.F.);
#11678=ORIENTED_EDGE('',*,*,#7982,.F.);
#11679=ORIENTED_EDGE('',*,*,#7985,.F.);
#11680=ORIENTED_EDGE('',*,*,#7988,.F.);
#11681=ORIENTED_EDGE('',*,*,#7991,.F.);
#11682=ORIENTED_EDGE('',*,*,#7994,.F.);
#11683=ORIENTED_EDGE('',*,*,#7997,.F.);
#11684=ORIENTED_EDGE('',*,*,#8000,.F.);
#11685=ORIENTED_EDGE('',*,*,#8003,.F.);
#11686=ORIENTED_EDGE('',*,*,#8006,.F.);
#11687=ORIENTED_EDGE('',*,*,#8009,.F.);
#11688=ORIENTED_EDGE('',*,*,#8012,.F.);
#11689=ORIENTED_EDGE('',*,*,#8015,.F.);
#11690=ORIENTED_EDGE('',*,*,#8018,.F.);
#11691=ORIENTED_EDGE('',*,*,#8021,.F.);
#11692=ORIENTED_EDGE('',*,*,#8024,.F.);
#11693=ORIENTED_EDGE('',*,*,#8027,.F.);
#11694=ORIENTED_EDGE('',*,*,#8602,.F.);
#11695=ORIENTED_EDGE('',*,*,#8032,.F.);
#11696=ORIENTED_EDGE('',*,*,#8603,.F.);
#11697=ORIENTED_EDGE('',*,*,#8089,.T.);
#11698=ORIENTED_EDGE('',*,*,#8599,.T.);
#11699=ORIENTED_EDGE('',*,*,#8087,.T.);
#11700=ORIENTED_EDGE('',*,*,#8084,.T.);
#11701=ORIENTED_EDGE('',*,*,#8081,.T.);
#11702=ORIENTED_EDGE('',*,*,#8078,.T.);
#11703=ORIENTED_EDGE('',*,*,#8075,.T.);
#11704=ORIENTED_EDGE('',*,*,#8072,.T.);
#11705=ORIENTED_EDGE('',*,*,#8069,.T.);
#11706=ORIENTED_EDGE('',*,*,#8066,.T.);
#11707=ORIENTED_EDGE('',*,*,#8063,.T.);
#11708=ORIENTED_EDGE('',*,*,#8060,.T.);
#11709=ORIENTED_EDGE('',*,*,#8057,.T.);
#11710=ORIENTED_EDGE('',*,*,#8054,.T.);
#11711=ORIENTED_EDGE('',*,*,#8051,.T.);
#11712=ORIENTED_EDGE('',*,*,#8048,.T.);
#11713=ORIENTED_EDGE('',*,*,#8045,.T.);
#11714=ORIENTED_EDGE('',*,*,#8042,.T.);
#11715=ORIENTED_EDGE('',*,*,#8039,.T.);
#11716=ORIENTED_EDGE('',*,*,#8036,.T.);
#11717=ORIENTED_EDGE('',*,*,#8029,.T.);
#11718=ORIENTED_EDGE('',*,*,#8602,.T.);
#11719=ORIENTED_EDGE('',*,*,#8026,.F.);
#11720=ORIENTED_EDGE('',*,*,#8601,.T.);
#11721=ORIENTED_EDGE('',*,*,#7858,.F.);
#11722=ORIENTED_EDGE('',*,*,#8604,.T.);
#11723=ORIENTED_EDGE('',*,*,#7917,.T.);
#11724=ORIENTED_EDGE('',*,*,#8605,.T.);
#11725=ORIENTED_EDGE('',*,*,#7861,.F.);
#11726=ORIENTED_EDGE('',*,*,#7970,.T.);
#11727=ORIENTED_EDGE('',*,*,#8606,.T.);
#11728=ORIENTED_EDGE('',*,*,#7967,.F.);
#11729=ORIENTED_EDGE('',*,*,#8607,.F.);
#11730=ORIENTED_EDGE('',*,*,#8605,.F.);
#11731=ORIENTED_EDGE('',*,*,#7916,.F.);
#11732=ORIENTED_EDGE('',*,*,#7920,.F.);
#11733=ORIENTED_EDGE('',*,*,#7923,.F.);
#11734=ORIENTED_EDGE('',*,*,#7926,.F.);
#11735=ORIENTED_EDGE('',*,*,#7929,.F.);
#11736=ORIENTED_EDGE('',*,*,#7932,.F.);
#11737=ORIENTED_EDGE('',*,*,#7935,.F.);
#11738=ORIENTED_EDGE('',*,*,#7938,.F.);
#11739=ORIENTED_EDGE('',*,*,#7941,.F.);
#11740=ORIENTED_EDGE('',*,*,#7944,.F.);
#11741=ORIENTED_EDGE('',*,*,#7947,.F.);
#11742=ORIENTED_EDGE('',*,*,#7950,.F.);
#11743=ORIENTED_EDGE('',*,*,#7953,.F.);
#11744=ORIENTED_EDGE('',*,*,#7956,.F.);
#11745=ORIENTED_EDGE('',*,*,#7959,.F.);
#11746=ORIENTED_EDGE('',*,*,#7962,.F.);
#11747=ORIENTED_EDGE('',*,*,#7965,.F.);
#11748=ORIENTED_EDGE('',*,*,#7968,.F.);
#11749=ORIENTED_EDGE('',*,*,#8606,.F.);
#11750=ORIENTED_EDGE('',*,*,#7973,.F.);
#11751=ORIENTED_EDGE('',*,*,#8608,.F.);
#11752=ORIENTED_EDGE('',*,*,#7912,.F.);
#11753=ORIENTED_EDGE('',*,*,#8609,.F.);
#11754=ORIENTED_EDGE('',*,*,#7910,.F.);
#11755=ORIENTED_EDGE('',*,*,#7907,.F.);
#11756=ORIENTED_EDGE('',*,*,#7904,.F.);
#11757=ORIENTED_EDGE('',*,*,#7901,.F.);
#11758=ORIENTED_EDGE('',*,*,#7898,.F.);
#11759=ORIENTED_EDGE('',*,*,#7895,.F.);
#11760=ORIENTED_EDGE('',*,*,#7892,.F.);
#11761=ORIENTED_EDGE('',*,*,#7889,.F.);
#11762=ORIENTED_EDGE('',*,*,#7886,.F.);
#11763=ORIENTED_EDGE('',*,*,#7883,.F.);
#11764=ORIENTED_EDGE('',*,*,#7880,.F.);
#11765=ORIENTED_EDGE('',*,*,#7877,.F.);
#11766=ORIENTED_EDGE('',*,*,#7874,.F.);
#11767=ORIENTED_EDGE('',*,*,#7871,.F.);
#11768=ORIENTED_EDGE('',*,*,#7868,.F.);
#11769=ORIENTED_EDGE('',*,*,#7865,.F.);
#11770=ORIENTED_EDGE('',*,*,#7862,.F.);
#11771=ORIENTED_EDGE('',*,*,#8604,.F.);
#11772=ORIENTED_EDGE('',*,*,#7857,.F.);
#11773=ORIENTED_EDGE('',*,*,#7864,.F.);
#11774=ORIENTED_EDGE('',*,*,#7867,.F.);
#11775=ORIENTED_EDGE('',*,*,#7870,.F.);
#11776=ORIENTED_EDGE('',*,*,#7873,.F.);
#11777=ORIENTED_EDGE('',*,*,#7876,.F.);
#11778=ORIENTED_EDGE('',*,*,#7879,.F.);
#11779=ORIENTED_EDGE('',*,*,#7882,.F.);
#11780=ORIENTED_EDGE('',*,*,#7885,.F.);
#11781=ORIENTED_EDGE('',*,*,#7888,.F.);
#11782=ORIENTED_EDGE('',*,*,#7891,.F.);
#11783=ORIENTED_EDGE('',*,*,#7894,.F.);
#11784=ORIENTED_EDGE('',*,*,#7897,.F.);
#11785=ORIENTED_EDGE('',*,*,#7900,.F.);
#11786=ORIENTED_EDGE('',*,*,#7903,.F.);
#11787=ORIENTED_EDGE('',*,*,#7906,.F.);
#11788=ORIENTED_EDGE('',*,*,#7909,.F.);
#11789=ORIENTED_EDGE('',*,*,#8610,.F.);
#11790=ORIENTED_EDGE('',*,*,#7914,.F.);
#11791=ORIENTED_EDGE('',*,*,#8611,.F.);
#11792=ORIENTED_EDGE('',*,*,#7971,.T.);
#11793=ORIENTED_EDGE('',*,*,#8607,.T.);
#11794=ORIENTED_EDGE('',*,*,#7969,.T.);
#11795=ORIENTED_EDGE('',*,*,#7966,.T.);
#11796=ORIENTED_EDGE('',*,*,#7963,.T.);
#11797=ORIENTED_EDGE('',*,*,#7960,.T.);
#11798=ORIENTED_EDGE('',*,*,#7957,.T.);
#11799=ORIENTED_EDGE('',*,*,#7954,.T.);
#11800=ORIENTED_EDGE('',*,*,#7951,.T.);
#11801=ORIENTED_EDGE('',*,*,#7948,.T.);
#11802=ORIENTED_EDGE('',*,*,#7945,.T.);
#11803=ORIENTED_EDGE('',*,*,#7942,.T.);
#11804=ORIENTED_EDGE('',*,*,#7939,.T.);
#11805=ORIENTED_EDGE('',*,*,#7936,.T.);
#11806=ORIENTED_EDGE('',*,*,#7933,.T.);
#11807=ORIENTED_EDGE('',*,*,#7930,.T.);
#11808=ORIENTED_EDGE('',*,*,#7927,.T.);
#11809=ORIENTED_EDGE('',*,*,#7924,.T.);
#11810=ORIENTED_EDGE('',*,*,#7921,.T.);
#11811=ORIENTED_EDGE('',*,*,#7918,.T.);
#11812=ORIENTED_EDGE('',*,*,#7911,.T.);
#11813=ORIENTED_EDGE('',*,*,#8610,.T.);
#11814=ORIENTED_EDGE('',*,*,#7908,.F.);
#11815=ORIENTED_EDGE('',*,*,#8609,.T.);
#11816=ORIENTED_EDGE('',*,*,#7740,.F.);
#11817=ORIENTED_EDGE('',*,*,#8612,.T.);
#11818=ORIENTED_EDGE('',*,*,#7799,.T.);
#11819=ORIENTED_EDGE('',*,*,#8613,.T.);
#11820=ORIENTED_EDGE('',*,*,#7743,.F.);
#11821=ORIENTED_EDGE('',*,*,#7852,.T.);
#11822=ORIENTED_EDGE('',*,*,#8614,.T.);
#11823=ORIENTED_EDGE('',*,*,#7849,.F.);
#11824=ORIENTED_EDGE('',*,*,#8615,.F.);
#11825=ORIENTED_EDGE('',*,*,#8613,.F.);
#11826=ORIENTED_EDGE('',*,*,#7798,.F.);
#11827=ORIENTED_EDGE('',*,*,#7802,.F.);
#11828=ORIENTED_EDGE('',*,*,#7805,.F.);
#11829=ORIENTED_EDGE('',*,*,#7808,.F.);
#11830=ORIENTED_EDGE('',*,*,#7811,.F.);
#11831=ORIENTED_EDGE('',*,*,#7814,.F.);
#11832=ORIENTED_EDGE('',*,*,#7817,.F.);
#11833=ORIENTED_EDGE('',*,*,#7820,.F.);
#11834=ORIENTED_EDGE('',*,*,#7823,.F.);
#11835=ORIENTED_EDGE('',*,*,#7826,.F.);
#11836=ORIENTED_EDGE('',*,*,#7829,.F.);
#11837=ORIENTED_EDGE('',*,*,#7832,.F.);
#11838=ORIENTED_EDGE('',*,*,#7835,.F.);
#11839=ORIENTED_EDGE('',*,*,#7838,.F.);
#11840=ORIENTED_EDGE('',*,*,#7841,.F.);
#11841=ORIENTED_EDGE('',*,*,#7844,.F.);
#11842=ORIENTED_EDGE('',*,*,#7847,.F.);
#11843=ORIENTED_EDGE('',*,*,#7850,.F.);
#11844=ORIENTED_EDGE('',*,*,#8614,.F.);
#11845=ORIENTED_EDGE('',*,*,#7855,.F.);
#11846=ORIENTED_EDGE('',*,*,#8616,.F.);
#11847=ORIENTED_EDGE('',*,*,#7794,.F.);
#11848=ORIENTED_EDGE('',*,*,#8617,.F.);
#11849=ORIENTED_EDGE('',*,*,#7792,.F.);
#11850=ORIENTED_EDGE('',*,*,#7789,.F.);
#11851=ORIENTED_EDGE('',*,*,#7786,.F.);
#11852=ORIENTED_EDGE('',*,*,#7783,.F.);
#11853=ORIENTED_EDGE('',*,*,#7780,.F.);
#11854=ORIENTED_EDGE('',*,*,#7777,.F.);
#11855=ORIENTED_EDGE('',*,*,#7774,.F.);
#11856=ORIENTED_EDGE('',*,*,#7771,.F.);
#11857=ORIENTED_EDGE('',*,*,#7768,.F.);
#11858=ORIENTED_EDGE('',*,*,#7765,.F.);
#11859=ORIENTED_EDGE('',*,*,#7762,.F.);
#11860=ORIENTED_EDGE('',*,*,#7759,.F.);
#11861=ORIENTED_EDGE('',*,*,#7756,.F.);
#11862=ORIENTED_EDGE('',*,*,#7753,.F.);
#11863=ORIENTED_EDGE('',*,*,#7750,.F.);
#11864=ORIENTED_EDGE('',*,*,#7747,.F.);
#11865=ORIENTED_EDGE('',*,*,#7744,.F.);
#11866=ORIENTED_EDGE('',*,*,#8612,.F.);
#11867=ORIENTED_EDGE('',*,*,#7739,.F.);
#11868=ORIENTED_EDGE('',*,*,#7746,.F.);
#11869=ORIENTED_EDGE('',*,*,#7749,.F.);
#11870=ORIENTED_EDGE('',*,*,#7752,.F.);
#11871=ORIENTED_EDGE('',*,*,#7755,.F.);
#11872=ORIENTED_EDGE('',*,*,#7758,.F.);
#11873=ORIENTED_EDGE('',*,*,#7761,.F.);
#11874=ORIENTED_EDGE('',*,*,#7764,.F.);
#11875=ORIENTED_EDGE('',*,*,#7767,.F.);
#11876=ORIENTED_EDGE('',*,*,#7770,.F.);
#11877=ORIENTED_EDGE('',*,*,#7773,.F.);
#11878=ORIENTED_EDGE('',*,*,#7776,.F.);
#11879=ORIENTED_EDGE('',*,*,#7779,.F.);
#11880=ORIENTED_EDGE('',*,*,#7782,.F.);
#11881=ORIENTED_EDGE('',*,*,#7785,.F.);
#11882=ORIENTED_EDGE('',*,*,#7788,.F.);
#11883=ORIENTED_EDGE('',*,*,#7791,.F.);
#11884=ORIENTED_EDGE('',*,*,#8618,.F.);
#11885=ORIENTED_EDGE('',*,*,#7796,.F.);
#11886=ORIENTED_EDGE('',*,*,#8619,.F.);
#11887=ORIENTED_EDGE('',*,*,#7853,.T.);
#11888=ORIENTED_EDGE('',*,*,#8615,.T.);
#11889=ORIENTED_EDGE('',*,*,#7851,.T.);
#11890=ORIENTED_EDGE('',*,*,#7848,.T.);
#11891=ORIENTED_EDGE('',*,*,#7845,.T.);
#11892=ORIENTED_EDGE('',*,*,#7842,.T.);
#11893=ORIENTED_EDGE('',*,*,#7839,.T.);
#11894=ORIENTED_EDGE('',*,*,#7836,.T.);
#11895=ORIENTED_EDGE('',*,*,#7833,.T.);
#11896=ORIENTED_EDGE('',*,*,#7830,.T.);
#11897=ORIENTED_EDGE('',*,*,#7827,.T.);
#11898=ORIENTED_EDGE('',*,*,#7824,.T.);
#11899=ORIENTED_EDGE('',*,*,#7821,.T.);
#11900=ORIENTED_EDGE('',*,*,#7818,.T.);
#11901=ORIENTED_EDGE('',*,*,#7815,.T.);
#11902=ORIENTED_EDGE('',*,*,#7812,.T.);
#11903=ORIENTED_EDGE('',*,*,#7809,.T.);
#11904=ORIENTED_EDGE('',*,*,#7806,.T.);
#11905=ORIENTED_EDGE('',*,*,#7803,.T.);
#11906=ORIENTED_EDGE('',*,*,#7800,.T.);
#11907=ORIENTED_EDGE('',*,*,#7793,.T.);
#11908=ORIENTED_EDGE('',*,*,#8618,.T.);
#11909=ORIENTED_EDGE('',*,*,#7790,.F.);
#11910=ORIENTED_EDGE('',*,*,#8617,.T.);
#11911=ORIENTED_EDGE('',*,*,#7622,.F.);
#11912=ORIENTED_EDGE('',*,*,#8620,.T.);
#11913=ORIENTED_EDGE('',*,*,#7681,.T.);
#11914=ORIENTED_EDGE('',*,*,#8621,.T.);
#11915=ORIENTED_EDGE('',*,*,#7625,.F.);
#11916=ORIENTED_EDGE('',*,*,#7734,.T.);
#11917=ORIENTED_EDGE('',*,*,#8622,.T.);
#11918=ORIENTED_EDGE('',*,*,#7731,.F.);
#11919=ORIENTED_EDGE('',*,*,#8623,.F.);
#11920=ORIENTED_EDGE('',*,*,#8621,.F.);
#11921=ORIENTED_EDGE('',*,*,#7680,.F.);
#11922=ORIENTED_EDGE('',*,*,#7684,.F.);
#11923=ORIENTED_EDGE('',*,*,#7687,.F.);
#11924=ORIENTED_EDGE('',*,*,#7690,.F.);
#11925=ORIENTED_EDGE('',*,*,#7693,.F.);
#11926=ORIENTED_EDGE('',*,*,#7696,.F.);
#11927=ORIENTED_EDGE('',*,*,#7699,.F.);
#11928=ORIENTED_EDGE('',*,*,#7702,.F.);
#11929=ORIENTED_EDGE('',*,*,#7705,.F.);
#11930=ORIENTED_EDGE('',*,*,#7708,.F.);
#11931=ORIENTED_EDGE('',*,*,#7711,.F.);
#11932=ORIENTED_EDGE('',*,*,#7714,.F.);
#11933=ORIENTED_EDGE('',*,*,#7717,.F.);
#11934=ORIENTED_EDGE('',*,*,#7720,.F.);
#11935=ORIENTED_EDGE('',*,*,#7723,.F.);
#11936=ORIENTED_EDGE('',*,*,#7726,.F.);
#11937=ORIENTED_EDGE('',*,*,#7729,.F.);
#11938=ORIENTED_EDGE('',*,*,#7732,.F.);
#11939=ORIENTED_EDGE('',*,*,#8622,.F.);
#11940=ORIENTED_EDGE('',*,*,#7737,.F.);
#11941=ORIENTED_EDGE('',*,*,#8624,.F.);
#11942=ORIENTED_EDGE('',*,*,#7676,.F.);
#11943=ORIENTED_EDGE('',*,*,#8625,.F.);
#11944=ORIENTED_EDGE('',*,*,#7674,.F.);
#11945=ORIENTED_EDGE('',*,*,#7671,.F.);
#11946=ORIENTED_EDGE('',*,*,#7668,.F.);
#11947=ORIENTED_EDGE('',*,*,#7665,.F.);
#11948=ORIENTED_EDGE('',*,*,#7662,.F.);
#11949=ORIENTED_EDGE('',*,*,#7659,.F.);
#11950=ORIENTED_EDGE('',*,*,#7656,.F.);
#11951=ORIENTED_EDGE('',*,*,#7653,.F.);
#11952=ORIENTED_EDGE('',*,*,#7650,.F.);
#11953=ORIENTED_EDGE('',*,*,#7647,.F.);
#11954=ORIENTED_EDGE('',*,*,#7644,.F.);
#11955=ORIENTED_EDGE('',*,*,#7641,.F.);
#11956=ORIENTED_EDGE('',*,*,#7638,.F.);
#11957=ORIENTED_EDGE('',*,*,#7635,.F.);
#11958=ORIENTED_EDGE('',*,*,#7632,.F.);
#11959=ORIENTED_EDGE('',*,*,#7629,.F.);
#11960=ORIENTED_EDGE('',*,*,#7626,.F.);
#11961=ORIENTED_EDGE('',*,*,#8620,.F.);
#11962=ORIENTED_EDGE('',*,*,#7621,.F.);
#11963=ORIENTED_EDGE('',*,*,#7628,.F.);
#11964=ORIENTED_EDGE('',*,*,#7631,.F.);
#11965=ORIENTED_EDGE('',*,*,#7634,.F.);
#11966=ORIENTED_EDGE('',*,*,#7637,.F.);
#11967=ORIENTED_EDGE('',*,*,#7640,.F.);
#11968=ORIENTED_EDGE('',*,*,#7643,.F.);
#11969=ORIENTED_EDGE('',*,*,#7646,.F.);
#11970=ORIENTED_EDGE('',*,*,#7649,.F.);
#11971=ORIENTED_EDGE('',*,*,#7652,.F.);
#11972=ORIENTED_EDGE('',*,*,#7655,.F.);
#11973=ORIENTED_EDGE('',*,*,#7658,.F.);
#11974=ORIENTED_EDGE('',*,*,#7661,.F.);
#11975=ORIENTED_EDGE('',*,*,#7664,.F.);
#11976=ORIENTED_EDGE('',*,*,#7667,.F.);
#11977=ORIENTED_EDGE('',*,*,#7670,.F.);
#11978=ORIENTED_EDGE('',*,*,#7673,.F.);
#11979=ORIENTED_EDGE('',*,*,#8626,.F.);
#11980=ORIENTED_EDGE('',*,*,#7678,.F.);
#11981=ORIENTED_EDGE('',*,*,#8627,.F.);
#11982=ORIENTED_EDGE('',*,*,#7735,.T.);
#11983=ORIENTED_EDGE('',*,*,#8623,.T.);
#11984=ORIENTED_EDGE('',*,*,#7733,.T.);
#11985=ORIENTED_EDGE('',*,*,#7730,.T.);
#11986=ORIENTED_EDGE('',*,*,#7727,.T.);
#11987=ORIENTED_EDGE('',*,*,#7724,.T.);
#11988=ORIENTED_EDGE('',*,*,#7721,.T.);
#11989=ORIENTED_EDGE('',*,*,#7718,.T.);
#11990=ORIENTED_EDGE('',*,*,#7715,.T.);
#11991=ORIENTED_EDGE('',*,*,#7712,.T.);
#11992=ORIENTED_EDGE('',*,*,#7709,.T.);
#11993=ORIENTED_EDGE('',*,*,#7706,.T.);
#11994=ORIENTED_EDGE('',*,*,#7703,.T.);
#11995=ORIENTED_EDGE('',*,*,#7700,.T.);
#11996=ORIENTED_EDGE('',*,*,#7697,.T.);
#11997=ORIENTED_EDGE('',*,*,#7694,.T.);
#11998=ORIENTED_EDGE('',*,*,#7691,.T.);
#11999=ORIENTED_EDGE('',*,*,#7688,.T.);
#12000=ORIENTED_EDGE('',*,*,#7685,.T.);
#12001=ORIENTED_EDGE('',*,*,#7682,.T.);
#12002=ORIENTED_EDGE('',*,*,#7675,.T.);
#12003=ORIENTED_EDGE('',*,*,#8626,.T.);
#12004=ORIENTED_EDGE('',*,*,#7672,.F.);
#12005=ORIENTED_EDGE('',*,*,#8625,.T.);
#12006=ORIENTED_EDGE('',*,*,#7624,.F.);
#12007=ORIENTED_EDGE('',*,*,#7978,.F.);
#12008=ORIENTED_EDGE('',*,*,#7860,.F.);
#12009=ORIENTED_EDGE('',*,*,#7742,.F.);
#12010=ORIENTED_EDGE('',*,*,#8628,.F.);
#12011=ORIENTED_EDGE('',*,*,#8629,.F.);
#12012=ORIENTED_EDGE('',*,*,#8630,.T.);
#12013=ORIENTED_EDGE('',*,*,#8631,.F.);
#12014=ORIENTED_EDGE('',*,*,#8632,.F.);
#12015=ORIENTED_EDGE('',*,*,#8633,.T.);
#12016=ORIENTED_EDGE('',*,*,#8634,.F.);
#12017=ORIENTED_EDGE('',*,*,#8630,.F.);
#12018=ORIENTED_EDGE('',*,*,#8635,.F.);
#12019=ORIENTED_EDGE('',*,*,#8636,.F.);
#12020=ORIENTED_EDGE('',*,*,#8633,.F.);
#12021=ORIENTED_EDGE('',*,*,#8637,.F.);
#12022=ORIENTED_EDGE('',*,*,#8631,.T.);
#12023=ORIENTED_EDGE('',*,*,#8634,.T.);
#12024=ORIENTED_EDGE('',*,*,#8636,.T.);
#12025=ORIENTED_EDGE('',*,*,#8638,.F.);
#12026=ORIENTED_EDGE('',*,*,#8603,.T.);
#12027=ORIENTED_EDGE('',*,*,#8031,.T.);
#12028=ORIENTED_EDGE('',*,*,#8600,.T.);
#12029=ORIENTED_EDGE('',*,*,#8090,.T.);
#12030=ORIENTED_EDGE('',*,*,#8611,.T.);
#12031=ORIENTED_EDGE('',*,*,#7913,.T.);
#12032=ORIENTED_EDGE('',*,*,#8608,.T.);
#12033=ORIENTED_EDGE('',*,*,#7972,.T.);
#12034=ORIENTED_EDGE('',*,*,#8619,.T.);
#12035=ORIENTED_EDGE('',*,*,#7795,.T.);
#12036=ORIENTED_EDGE('',*,*,#8616,.T.);
#12037=ORIENTED_EDGE('',*,*,#7854,.T.);
#12038=ORIENTED_EDGE('',*,*,#8627,.T.);
#12039=ORIENTED_EDGE('',*,*,#7677,.T.);
#12040=ORIENTED_EDGE('',*,*,#8624,.T.);
#12041=ORIENTED_EDGE('',*,*,#7736,.T.);
#12042=ORIENTED_EDGE('',*,*,#8639,.F.);
#12043=ORIENTED_EDGE('',*,*,#7616,.T.);
#12044=ORIENTED_EDGE('',*,*,#8640,.T.);
#12045=ORIENTED_EDGE('',*,*,#7613,.F.);
#12046=ORIENTED_EDGE('',*,*,#8641,.F.);
#12047=ORIENTED_EDGE('',*,*,#8642,.F.);
#12048=ORIENTED_EDGE('',*,*,#7598,.F.);
#12049=ORIENTED_EDGE('',*,*,#7602,.F.);
#12050=ORIENTED_EDGE('',*,*,#7605,.F.);
#12051=ORIENTED_EDGE('',*,*,#7608,.F.);
#12052=ORIENTED_EDGE('',*,*,#7611,.F.);
#12053=ORIENTED_EDGE('',*,*,#7614,.F.);
#12054=ORIENTED_EDGE('',*,*,#8640,.F.);
#12055=ORIENTED_EDGE('',*,*,#7619,.F.);
#12056=ORIENTED_EDGE('',*,*,#8643,.F.);
#12057=ORIENTED_EDGE('',*,*,#7594,.F.);
#12058=ORIENTED_EDGE('',*,*,#8644,.F.);
#12059=ORIENTED_EDGE('',*,*,#7592,.F.);
#12060=ORIENTED_EDGE('',*,*,#7589,.F.);
#12061=ORIENTED_EDGE('',*,*,#7586,.F.);
#12062=ORIENTED_EDGE('',*,*,#7583,.F.);
#12063=ORIENTED_EDGE('',*,*,#7580,.F.);
#12064=ORIENTED_EDGE('',*,*,#7576,.F.);
#12065=ORIENTED_EDGE('',*,*,#8645,.F.);
#12066=ORIENTED_EDGE('',*,*,#7578,.F.);
#12067=ORIENTED_EDGE('',*,*,#7582,.F.);
#12068=ORIENTED_EDGE('',*,*,#7585,.F.);
#12069=ORIENTED_EDGE('',*,*,#7588,.F.);
#12070=ORIENTED_EDGE('',*,*,#7591,.F.);
#12071=ORIENTED_EDGE('',*,*,#8646,.F.);
#12072=ORIENTED_EDGE('',*,*,#7596,.F.);
#12073=ORIENTED_EDGE('',*,*,#8647,.F.);
#12074=ORIENTED_EDGE('',*,*,#7617,.T.);
#12075=ORIENTED_EDGE('',*,*,#8641,.T.);
#12076=ORIENTED_EDGE('',*,*,#7615,.T.);
#12077=ORIENTED_EDGE('',*,*,#7612,.T.);
#12078=ORIENTED_EDGE('',*,*,#7609,.T.);
#12079=ORIENTED_EDGE('',*,*,#7606,.T.);
#12080=ORIENTED_EDGE('',*,*,#7603,.T.);
#12081=ORIENTED_EDGE('',*,*,#7600,.T.);
#12082=ORIENTED_EDGE('',*,*,#8648,.F.);
#12083=ORIENTED_EDGE('',*,*,#8649,.T.);
#12084=ORIENTED_EDGE('',*,*,#8650,.T.);
#12085=ORIENTED_EDGE('',*,*,#8651,.T.);
#12086=ORIENTED_EDGE('',*,*,#8643,.T.);
#12087=ORIENTED_EDGE('',*,*,#7618,.T.);
#12088=ORIENTED_EDGE('',*,*,#8647,.T.);
#12089=ORIENTED_EDGE('',*,*,#7595,.T.);
#12090=ORIENTED_EDGE('',*,*,#7593,.T.);
#12091=ORIENTED_EDGE('',*,*,#8646,.T.);
#12092=ORIENTED_EDGE('',*,*,#7590,.F.);
#12093=ORIENTED_EDGE('',*,*,#8644,.T.);
#12094=ORIENTED_EDGE('',*,*,#8652,.F.);
#12095=ORIENTED_EDGE('',*,*,#8653,.T.);
#12096=ORIENTED_EDGE('',*,*,#8654,.T.);
#12097=ORIENTED_EDGE('',*,*,#8649,.F.);
#12098=ORIENTED_EDGE('',*,*,#8655,.F.);
#12099=ORIENTED_EDGE('',*,*,#8651,.F.);
#12100=ORIENTED_EDGE('',*,*,#8656,.F.);
#12101=ORIENTED_EDGE('',*,*,#8657,.T.);
#12102=ORIENTED_EDGE('',*,*,#8658,.T.);
#12103=ORIENTED_EDGE('',*,*,#8656,.T.);
#12104=ORIENTED_EDGE('',*,*,#8650,.F.);
#12105=ORIENTED_EDGE('',*,*,#8654,.F.);
#12106=ORIENTED_EDGE('',*,*,#8659,.F.);
#12107=ORIENTED_EDGE('',*,*,#8657,.F.);
#12108=ORIENTED_EDGE('',*,*,#8658,.F.);
#12109=ORIENTED_EDGE('',*,*,#8653,.F.);
#12110=ORIENTED_EDGE('',*,*,#8642,.T.);
#12111=ORIENTED_EDGE('',*,*,#7575,.T.);
#12112=ORIENTED_EDGE('',*,*,#7579,.T.);
#12113=ORIENTED_EDGE('',*,*,#8645,.T.);
#12114=ORIENTED_EDGE('',*,*,#7599,.T.);
#12115=ORIENTED_EDGE('',*,*,#8660,.F.);
#12116=ORIENTED_EDGE('',*,*,#8661,.T.);
#12117=ORIENTED_EDGE('',*,*,#8662,.F.);
#12118=ORIENTED_EDGE('',*,*,#8663,.F.);
#12119=ORIENTED_EDGE('',*,*,#8661,.F.);
#12120=ORIENTED_EDGE('',*,*,#8664,.T.);
#12121=ORIENTED_EDGE('',*,*,#8663,.T.);
#12122=ORIENTED_EDGE('',*,*,#8664,.F.);
#12123=ORIENTED_EDGE('',*,*,#8662,.T.);
#12124=ORIENTED_EDGE('',*,*,#8665,.T.);
#12125=ORIENTED_EDGE('',*,*,#8666,.T.);
#12126=ORIENTED_EDGE('',*,*,#8665,.F.);
#12127=ORIENTED_EDGE('',*,*,#8666,.F.);
#12128=ORIENTED_EDGE('',*,*,#8667,.T.);
#12129=ORIENTED_EDGE('',*,*,#8668,.F.);
#12130=ORIENTED_EDGE('',*,*,#8669,.F.);
#12131=ORIENTED_EDGE('',*,*,#8667,.F.);
#12132=ORIENTED_EDGE('',*,*,#8670,.T.);
#12133=ORIENTED_EDGE('',*,*,#8669,.T.);
#12134=ORIENTED_EDGE('',*,*,#8670,.F.);
#12135=ORIENTED_EDGE('',*,*,#8668,.T.);
#12136=ORIENTED_EDGE('',*,*,#8671,.T.);
#12137=ORIENTED_EDGE('',*,*,#8639,.T.);
#12138=ORIENTED_EDGE('',*,*,#8671,.F.);
#12139=ORIENTED_EDGE('',*,*,#8672,.F.);
#12140=ORIENTED_EDGE('',*,*,#8673,.T.);
#12141=ORIENTED_EDGE('',*,*,#8660,.T.);
#12142=ORIENTED_EDGE('',*,*,#8673,.F.);
#12143=ORIENTED_EDGE('',*,*,#8628,.T.);
#12144=ORIENTED_EDGE('',*,*,#8638,.T.);
#12145=ORIENTED_EDGE('',*,*,#8635,.T.);
#12146=ORIENTED_EDGE('',*,*,#8674,.F.);
#12147=ORIENTED_EDGE('',*,*,#8652,.T.);
#12148=ORIENTED_EDGE('',*,*,#8648,.T.);
#12149=ORIENTED_EDGE('',*,*,#8655,.T.);
#12150=ORIENTED_EDGE('',*,*,#8659,.T.);
#12151=ORIENTED_EDGE('',*,*,#8629,.T.);
#12152=ORIENTED_EDGE('',*,*,#8674,.T.);
#12153=ORIENTED_EDGE('',*,*,#8637,.T.);
#12154=ORIENTED_EDGE('',*,*,#8632,.T.);
#12155=ORIENTED_EDGE('',*,*,#8571,.T.);
#12156=ORIENTED_EDGE('',*,*,#8503,.T.);
#12157=ORIENTED_EDGE('',*,*,#8568,.T.);
#12158=ORIENTED_EDGE('',*,*,#8562,.T.);
#12159=ORIENTED_EDGE('',*,*,#8579,.T.);
#12160=ORIENTED_EDGE('',*,*,#8385,.T.);
#12161=ORIENTED_EDGE('',*,*,#8576,.T.);
#12162=ORIENTED_EDGE('',*,*,#8444,.T.);
#12163=ORIENTED_EDGE('',*,*,#8587,.T.);
#12164=ORIENTED_EDGE('',*,*,#8267,.T.);
#12165=ORIENTED_EDGE('',*,*,#8584,.T.);
#12166=ORIENTED_EDGE('',*,*,#8326,.T.);
#12167=ORIENTED_EDGE('',*,*,#8595,.T.);
#12168=ORIENTED_EDGE('',*,*,#8149,.T.);
#12169=ORIENTED_EDGE('',*,*,#8592,.T.);
#12170=ORIENTED_EDGE('',*,*,#8208,.T.);
#12171=ORIENTED_EDGE('',*,*,#8672,.T.);
#12172=ORIENTED_EDGE('',*,*,#8675,.T.);
#12173=ORIENTED_EDGE('',*,*,#8676,.T.);
#12174=ORIENTED_EDGE('',*,*,#8677,.T.);
#12175=ORIENTED_EDGE('',*,*,#8678,.T.);
#12176=ORIENTED_EDGE('',*,*,#8679,.T.);
#12177=ORIENTED_EDGE('',*,*,#8680,.T.);
#12178=ORIENTED_EDGE('',*,*,#8681,.T.);
#12179=ORIENTED_EDGE('',*,*,#8675,.F.);
#12180=ORIENTED_EDGE('',*,*,#8682,.T.);
#12181=ORIENTED_EDGE('',*,*,#8683,.T.);
#12182=ORIENTED_EDGE('',*,*,#8684,.T.);
#12183=ORIENTED_EDGE('',*,*,#8680,.F.);
#12184=ORIENTED_EDGE('',*,*,#8685,.T.);
#12185=ORIENTED_EDGE('',*,*,#8686,.T.);
#12186=ORIENTED_EDGE('',*,*,#8687,.T.);
#12187=ORIENTED_EDGE('',*,*,#8683,.F.);
#12188=ORIENTED_EDGE('',*,*,#8688,.T.);
#12189=ORIENTED_EDGE('',*,*,#8689,.T.);
#12190=ORIENTED_EDGE('',*,*,#8690,.T.);
#12191=ORIENTED_EDGE('',*,*,#8686,.F.);
#12192=ORIENTED_EDGE('',*,*,#8691,.T.);
#12193=ORIENTED_EDGE('',*,*,#8692,.T.);
#12194=ORIENTED_EDGE('',*,*,#8693,.T.);
#12195=ORIENTED_EDGE('',*,*,#8689,.F.);
#12196=ORIENTED_EDGE('',*,*,#8694,.T.);
#12197=ORIENTED_EDGE('',*,*,#8695,.T.);
#12198=ORIENTED_EDGE('',*,*,#8696,.T.);
#12199=ORIENTED_EDGE('',*,*,#8692,.F.);
#12200=ORIENTED_EDGE('',*,*,#8697,.T.);
#12201=ORIENTED_EDGE('',*,*,#8698,.T.);
#12202=ORIENTED_EDGE('',*,*,#8699,.T.);
#12203=ORIENTED_EDGE('',*,*,#8695,.F.);
#12204=ORIENTED_EDGE('',*,*,#8700,.T.);
#12205=ORIENTED_EDGE('',*,*,#8701,.T.);
#12206=ORIENTED_EDGE('',*,*,#8702,.T.);
#12207=ORIENTED_EDGE('',*,*,#8698,.F.);
#12208=ORIENTED_EDGE('',*,*,#8703,.T.);
#12209=ORIENTED_EDGE('',*,*,#8704,.T.);
#12210=ORIENTED_EDGE('',*,*,#8705,.T.);
#12211=ORIENTED_EDGE('',*,*,#8701,.F.);
#12212=ORIENTED_EDGE('',*,*,#8706,.T.);
#12213=ORIENTED_EDGE('',*,*,#8707,.T.);
#12214=ORIENTED_EDGE('',*,*,#8708,.T.);
#12215=ORIENTED_EDGE('',*,*,#8704,.F.);
#12216=ORIENTED_EDGE('',*,*,#8709,.T.);
#12217=ORIENTED_EDGE('',*,*,#8710,.T.);
#12218=ORIENTED_EDGE('',*,*,#8711,.T.);
#12219=ORIENTED_EDGE('',*,*,#8707,.F.);
#12220=ORIENTED_EDGE('',*,*,#8712,.T.);
#12221=ORIENTED_EDGE('',*,*,#8713,.T.);
#12222=ORIENTED_EDGE('',*,*,#8714,.T.);
#12223=ORIENTED_EDGE('',*,*,#8710,.F.);
#12224=ORIENTED_EDGE('',*,*,#8715,.T.);
#12225=ORIENTED_EDGE('',*,*,#8716,.T.);
#12226=ORIENTED_EDGE('',*,*,#8717,.T.);
#12227=ORIENTED_EDGE('',*,*,#8713,.F.);
#12228=ORIENTED_EDGE('',*,*,#8718,.T.);
#12229=ORIENTED_EDGE('',*,*,#8719,.T.);
#12230=ORIENTED_EDGE('',*,*,#8720,.T.);
#12231=ORIENTED_EDGE('',*,*,#8716,.F.);
#12232=ORIENTED_EDGE('',*,*,#8721,.T.);
#12233=ORIENTED_EDGE('',*,*,#8722,.T.);
#12234=ORIENTED_EDGE('',*,*,#8723,.T.);
#12235=ORIENTED_EDGE('',*,*,#8719,.F.);
#12236=ORIENTED_EDGE('',*,*,#8724,.T.);
#12237=ORIENTED_EDGE('',*,*,#8725,.T.);
#12238=ORIENTED_EDGE('',*,*,#8726,.T.);
#12239=ORIENTED_EDGE('',*,*,#8722,.F.);
#12240=ORIENTED_EDGE('',*,*,#8727,.T.);
#12241=ORIENTED_EDGE('',*,*,#8728,.F.);
#12242=ORIENTED_EDGE('',*,*,#8729,.T.);
#12243=ORIENTED_EDGE('',*,*,#8730,.F.);
#12244=ORIENTED_EDGE('',*,*,#8731,.T.);
#12245=ORIENTED_EDGE('',*,*,#8732,.T.);
#12246=ORIENTED_EDGE('',*,*,#8733,.T.);
#12247=ORIENTED_EDGE('',*,*,#8734,.F.);
#12248=ORIENTED_EDGE('',*,*,#8735,.F.);
#12249=ORIENTED_EDGE('',*,*,#8736,.F.);
#12250=ORIENTED_EDGE('',*,*,#8737,.T.);
#12251=ORIENTED_EDGE('',*,*,#8738,.T.);
#12252=ORIENTED_EDGE('',*,*,#8732,.F.);
#12253=ORIENTED_EDGE('',*,*,#8739,.F.);
#12254=ORIENTED_EDGE('',*,*,#8740,.T.);
#12255=ORIENTED_EDGE('',*,*,#8741,.T.);
#12256=ORIENTED_EDGE('',*,*,#8737,.F.);
#12257=ORIENTED_EDGE('',*,*,#8742,.F.);
#12258=ORIENTED_EDGE('',*,*,#8743,.T.);
#12259=ORIENTED_EDGE('',*,*,#8744,.T.);
#12260=ORIENTED_EDGE('',*,*,#8740,.F.);
#12261=ORIENTED_EDGE('',*,*,#8745,.F.);
#12262=ORIENTED_EDGE('',*,*,#8746,.T.);
#12263=ORIENTED_EDGE('',*,*,#8747,.T.);
#12264=ORIENTED_EDGE('',*,*,#8743,.F.);
#12265=ORIENTED_EDGE('',*,*,#8748,.F.);
#12266=ORIENTED_EDGE('',*,*,#8749,.T.);
#12267=ORIENTED_EDGE('',*,*,#8750,.T.);
#12268=ORIENTED_EDGE('',*,*,#8746,.F.);
#12269=ORIENTED_EDGE('',*,*,#8751,.F.);
#12270=ORIENTED_EDGE('',*,*,#8752,.T.);
#12271=ORIENTED_EDGE('',*,*,#8753,.T.);
#12272=ORIENTED_EDGE('',*,*,#8749,.F.);
#12273=ORIENTED_EDGE('',*,*,#8754,.F.);
#12274=ORIENTED_EDGE('',*,*,#8755,.T.);
#12275=ORIENTED_EDGE('',*,*,#8756,.T.);
#12276=ORIENTED_EDGE('',*,*,#8752,.F.);
#12277=ORIENTED_EDGE('',*,*,#8757,.F.);
#12278=ORIENTED_EDGE('',*,*,#8758,.T.);
#12279=ORIENTED_EDGE('',*,*,#8759,.T.);
#12280=ORIENTED_EDGE('',*,*,#8755,.F.);
#12281=ORIENTED_EDGE('',*,*,#8760,.F.);
#12282=ORIENTED_EDGE('',*,*,#8761,.T.);
#12283=ORIENTED_EDGE('',*,*,#8762,.T.);
#12284=ORIENTED_EDGE('',*,*,#8758,.F.);
#12285=ORIENTED_EDGE('',*,*,#8763,.F.);
#12286=ORIENTED_EDGE('',*,*,#8764,.T.);
#12287=ORIENTED_EDGE('',*,*,#8765,.T.);
#12288=ORIENTED_EDGE('',*,*,#8761,.F.);
#12289=ORIENTED_EDGE('',*,*,#8766,.F.);
#12290=ORIENTED_EDGE('',*,*,#8767,.T.);
#12291=ORIENTED_EDGE('',*,*,#8768,.T.);
#12292=ORIENTED_EDGE('',*,*,#8764,.F.);
#12293=ORIENTED_EDGE('',*,*,#8769,.F.);
#12294=ORIENTED_EDGE('',*,*,#8770,.T.);
#12295=ORIENTED_EDGE('',*,*,#8771,.T.);
#12296=ORIENTED_EDGE('',*,*,#8767,.F.);
#12297=ORIENTED_EDGE('',*,*,#8772,.F.);
#12298=ORIENTED_EDGE('',*,*,#8773,.T.);
#12299=ORIENTED_EDGE('',*,*,#8774,.T.);
#12300=ORIENTED_EDGE('',*,*,#8770,.F.);
#12301=ORIENTED_EDGE('',*,*,#8775,.F.);
#12302=ORIENTED_EDGE('',*,*,#8776,.T.);
#12303=ORIENTED_EDGE('',*,*,#8777,.T.);
#12304=ORIENTED_EDGE('',*,*,#8773,.F.);
#12305=ORIENTED_EDGE('',*,*,#8778,.F.);
#12306=ORIENTED_EDGE('',*,*,#8779,.T.);
#12307=ORIENTED_EDGE('',*,*,#8780,.T.);
#12308=ORIENTED_EDGE('',*,*,#8776,.F.);
#12309=ORIENTED_EDGE('',*,*,#8781,.F.);
#12310=ORIENTED_EDGE('',*,*,#8782,.T.);
#12311=ORIENTED_EDGE('',*,*,#8783,.T.);
#12312=ORIENTED_EDGE('',*,*,#8779,.F.);
#12313=ORIENTED_EDGE('',*,*,#8784,.F.);
#12314=ORIENTED_EDGE('',*,*,#8785,.F.);
#12315=ORIENTED_EDGE('',*,*,#8786,.F.);
#12316=ORIENTED_EDGE('',*,*,#8787,.F.);
#12317=ORIENTED_EDGE('',*,*,#8788,.F.);
#12318=ORIENTED_EDGE('',*,*,#8789,.T.);
#12319=ORIENTED_EDGE('',*,*,#8790,.T.);
#12320=ORIENTED_EDGE('',*,*,#8791,.T.);
#12321=ORIENTED_EDGE('',*,*,#8792,.F.);
#12322=ORIENTED_EDGE('',*,*,#8791,.F.);
#12323=ORIENTED_EDGE('',*,*,#8793,.F.);
#12324=ORIENTED_EDGE('',*,*,#8790,.F.);
#12325=ORIENTED_EDGE('',*,*,#8794,.F.);
#12326=ORIENTED_EDGE('',*,*,#8792,.T.);
#12327=ORIENTED_EDGE('',*,*,#8795,.F.);
#12328=ORIENTED_EDGE('',*,*,#8796,.T.);
#12329=ORIENTED_EDGE('',*,*,#8794,.T.);
#12330=ORIENTED_EDGE('',*,*,#8796,.F.);
#12331=ORIENTED_EDGE('',*,*,#8797,.F.);
#12332=ORIENTED_EDGE('',*,*,#8798,.F.);
#12333=ORIENTED_EDGE('',*,*,#8799,.F.);
#12334=ORIENTED_EDGE('',*,*,#8800,.F.);
#12335=ORIENTED_EDGE('',*,*,#8801,.T.);
#12336=ORIENTED_EDGE('',*,*,#8799,.T.);
#12337=ORIENTED_EDGE('',*,*,#8802,.T.);
#12338=ORIENTED_EDGE('',*,*,#8803,.T.);
#12339=ORIENTED_EDGE('',*,*,#8804,.F.);
#12340=ORIENTED_EDGE('',*,*,#8800,.T.);
#12341=ORIENTED_EDGE('',*,*,#8801,.F.);
#12342=ORIENTED_EDGE('',*,*,#8805,.T.);
#12343=ORIENTED_EDGE('',*,*,#8806,.F.);
#12344=ORIENTED_EDGE('',*,*,#8805,.F.);
#12345=ORIENTED_EDGE('',*,*,#8803,.F.);
#12346=ORIENTED_EDGE('',*,*,#8807,.F.);
#12347=ORIENTED_EDGE('',*,*,#8795,.T.);
#12348=ORIENTED_EDGE('',*,*,#8808,.T.);
#12349=ORIENTED_EDGE('',*,*,#8809,.T.);
#12350=ORIENTED_EDGE('',*,*,#8807,.T.);
#12351=ORIENTED_EDGE('',*,*,#8802,.F.);
#12352=ORIENTED_EDGE('',*,*,#8798,.T.);
#12353=ORIENTED_EDGE('',*,*,#8810,.F.);
#12354=ORIENTED_EDGE('',*,*,#8729,.F.);
#12355=ORIENTED_EDGE('',*,*,#8811,.F.);
#12356=ORIENTED_EDGE('',*,*,#8727,.F.);
#12357=ORIENTED_EDGE('',*,*,#8724,.F.);
#12358=ORIENTED_EDGE('',*,*,#8721,.F.);
#12359=ORIENTED_EDGE('',*,*,#8718,.F.);
#12360=ORIENTED_EDGE('',*,*,#8715,.F.);
#12361=ORIENTED_EDGE('',*,*,#8712,.F.);
#12362=ORIENTED_EDGE('',*,*,#8709,.F.);
#12363=ORIENTED_EDGE('',*,*,#8706,.F.);
#12364=ORIENTED_EDGE('',*,*,#8703,.F.);
#12365=ORIENTED_EDGE('',*,*,#8700,.F.);
#12366=ORIENTED_EDGE('',*,*,#8697,.F.);
#12367=ORIENTED_EDGE('',*,*,#8694,.F.);
#12368=ORIENTED_EDGE('',*,*,#8691,.F.);
#12369=ORIENTED_EDGE('',*,*,#8688,.F.);
#12370=ORIENTED_EDGE('',*,*,#8685,.F.);
#12371=ORIENTED_EDGE('',*,*,#8682,.F.);
#12372=ORIENTED_EDGE('',*,*,#8679,.F.);
#12373=ORIENTED_EDGE('',*,*,#8812,.F.);
#12374=ORIENTED_EDGE('',*,*,#8733,.F.);
#12375=ORIENTED_EDGE('',*,*,#8738,.F.);
#12376=ORIENTED_EDGE('',*,*,#8741,.F.);
#12377=ORIENTED_EDGE('',*,*,#8744,.F.);
#12378=ORIENTED_EDGE('',*,*,#8747,.F.);
#12379=ORIENTED_EDGE('',*,*,#8750,.F.);
#12380=ORIENTED_EDGE('',*,*,#8753,.F.);
#12381=ORIENTED_EDGE('',*,*,#8756,.F.);
#12382=ORIENTED_EDGE('',*,*,#8759,.F.);
#12383=ORIENTED_EDGE('',*,*,#8762,.F.);
#12384=ORIENTED_EDGE('',*,*,#8765,.F.);
#12385=ORIENTED_EDGE('',*,*,#8768,.F.);
#12386=ORIENTED_EDGE('',*,*,#8771,.F.);
#12387=ORIENTED_EDGE('',*,*,#8774,.F.);
#12388=ORIENTED_EDGE('',*,*,#8777,.F.);
#12389=ORIENTED_EDGE('',*,*,#8780,.F.);
#12390=ORIENTED_EDGE('',*,*,#8783,.F.);
#12391=ORIENTED_EDGE('',*,*,#8813,.F.);
#12392=ORIENTED_EDGE('',*,*,#8789,.F.);
#12393=ORIENTED_EDGE('',*,*,#8785,.T.);
#12394=ORIENTED_EDGE('',*,*,#8813,.T.);
#12395=ORIENTED_EDGE('',*,*,#8782,.F.);
#12396=ORIENTED_EDGE('',*,*,#8814,.F.);
#12397=ORIENTED_EDGE('',*,*,#8815,.F.);
#12398=ORIENTED_EDGE('',*,*,#8786,.T.);
#12399=ORIENTED_EDGE('',*,*,#8814,.T.);
#12400=ORIENTED_EDGE('',*,*,#8784,.T.);
#12401=ORIENTED_EDGE('',*,*,#8781,.T.);
#12402=ORIENTED_EDGE('',*,*,#8778,.T.);
#12403=ORIENTED_EDGE('',*,*,#8775,.T.);
#12404=ORIENTED_EDGE('',*,*,#8772,.T.);
#12405=ORIENTED_EDGE('',*,*,#8769,.T.);
#12406=ORIENTED_EDGE('',*,*,#8766,.T.);
#12407=ORIENTED_EDGE('',*,*,#8763,.T.);
#12408=ORIENTED_EDGE('',*,*,#8760,.T.);
#12409=ORIENTED_EDGE('',*,*,#8757,.T.);
#12410=ORIENTED_EDGE('',*,*,#8754,.T.);
#12411=ORIENTED_EDGE('',*,*,#8751,.T.);
#12412=ORIENTED_EDGE('',*,*,#8748,.T.);
#12413=ORIENTED_EDGE('',*,*,#8745,.T.);
#12414=ORIENTED_EDGE('',*,*,#8742,.T.);
#12415=ORIENTED_EDGE('',*,*,#8739,.T.);
#12416=ORIENTED_EDGE('',*,*,#8736,.T.);
#12417=ORIENTED_EDGE('',*,*,#8816,.F.);
#12418=ORIENTED_EDGE('',*,*,#8676,.F.);
#12419=ORIENTED_EDGE('',*,*,#8681,.F.);
#12420=ORIENTED_EDGE('',*,*,#8684,.F.);
#12421=ORIENTED_EDGE('',*,*,#8687,.F.);
#12422=ORIENTED_EDGE('',*,*,#8690,.F.);
#12423=ORIENTED_EDGE('',*,*,#8693,.F.);
#12424=ORIENTED_EDGE('',*,*,#8696,.F.);
#12425=ORIENTED_EDGE('',*,*,#8699,.F.);
#12426=ORIENTED_EDGE('',*,*,#8702,.F.);
#12427=ORIENTED_EDGE('',*,*,#8705,.F.);
#12428=ORIENTED_EDGE('',*,*,#8708,.F.);
#12429=ORIENTED_EDGE('',*,*,#8711,.F.);
#12430=ORIENTED_EDGE('',*,*,#8714,.F.);
#12431=ORIENTED_EDGE('',*,*,#8717,.F.);
#12432=ORIENTED_EDGE('',*,*,#8720,.F.);
#12433=ORIENTED_EDGE('',*,*,#8723,.F.);
#12434=ORIENTED_EDGE('',*,*,#8726,.F.);
#12435=ORIENTED_EDGE('',*,*,#8817,.F.);
#12436=ORIENTED_EDGE('',*,*,#8731,.F.);
#12437=ORIENTED_EDGE('',*,*,#8818,.T.);
#12438=ORIENTED_EDGE('',*,*,#8734,.T.);
#12439=ORIENTED_EDGE('',*,*,#8812,.T.);
#12440=ORIENTED_EDGE('',*,*,#8678,.F.);
#12441=ORIENTED_EDGE('',*,*,#8728,.T.);
#12442=ORIENTED_EDGE('',*,*,#8817,.T.);
#12443=ORIENTED_EDGE('',*,*,#8725,.F.);
#12444=ORIENTED_EDGE('',*,*,#8811,.T.);
#12445=ORIENTED_EDGE('',*,*,#8819,.F.);
#12446=ORIENTED_EDGE('',*,*,#8677,.F.);
#12447=ORIENTED_EDGE('',*,*,#8816,.T.);
#12448=ORIENTED_EDGE('',*,*,#8735,.T.);
#12449=ORIENTED_EDGE('',*,*,#8820,.F.);
#12450=ORIENTED_EDGE('',*,*,#8821,.T.);
#12451=ORIENTED_EDGE('',*,*,#8818,.F.);
#12452=ORIENTED_EDGE('',*,*,#8822,.T.);
#12453=ORIENTED_EDGE('',*,*,#8823,.T.);
#12454=ORIENTED_EDGE('',*,*,#8822,.F.);
#12455=ORIENTED_EDGE('',*,*,#8819,.T.);
#12456=ORIENTED_EDGE('',*,*,#8821,.F.);
#12457=ORIENTED_EDGE('',*,*,#8823,.F.);
#12458=ORIENTED_EDGE('',*,*,#8824,.F.);
#12459=ORIENTED_EDGE('',*,*,#8825,.T.);
#12460=ORIENTED_EDGE('',*,*,#8808,.F.);
#12461=ORIENTED_EDGE('',*,*,#8797,.T.);
#12462=ORIENTED_EDGE('',*,*,#8804,.T.);
#12463=ORIENTED_EDGE('',*,*,#8806,.T.);
#12464=ORIENTED_EDGE('',*,*,#8809,.F.);
#12465=ORIENTED_EDGE('',*,*,#8825,.F.);
#12466=ORIENTED_EDGE('',*,*,#8824,.T.);
#12467=ORIENTED_EDGE('',*,*,#8826,.T.);
#12468=ORIENTED_EDGE('',*,*,#8827,.F.);
#12469=ORIENTED_EDGE('',*,*,#8828,.F.);
#12470=ORIENTED_EDGE('',*,*,#8829,.F.);
#12471=ORIENTED_EDGE('',*,*,#8826,.F.);
#12472=ORIENTED_EDGE('',*,*,#8830,.T.);
#12473=ORIENTED_EDGE('',*,*,#8828,.T.);
#12474=ORIENTED_EDGE('',*,*,#8830,.F.);
#12475=ORIENTED_EDGE('',*,*,#8829,.T.);
#12476=ORIENTED_EDGE('',*,*,#8831,.T.);
#12477=ORIENTED_EDGE('',*,*,#8832,.T.);
#12478=ORIENTED_EDGE('',*,*,#8831,.F.);
#12479=ORIENTED_EDGE('',*,*,#8833,.T.);
#12480=ORIENTED_EDGE('',*,*,#8832,.F.);
#12481=ORIENTED_EDGE('',*,*,#8833,.F.);
#12482=ORIENTED_EDGE('',*,*,#8834,.T.);
#12483=ORIENTED_EDGE('',*,*,#8835,.T.);
#12484=ORIENTED_EDGE('',*,*,#8834,.F.);
#12485=ORIENTED_EDGE('',*,*,#8815,.T.);
#12486=ORIENTED_EDGE('',*,*,#8730,.T.);
#12487=ORIENTED_EDGE('',*,*,#8810,.T.);
#12488=ORIENTED_EDGE('',*,*,#8788,.T.);
#12489=ORIENTED_EDGE('',*,*,#8787,.T.);
#12490=ORIENTED_EDGE('',*,*,#8835,.F.);
#12491=ORIENTED_EDGE('',*,*,#8820,.T.);
#12492=ORIENTED_EDGE('',*,*,#8793,.T.);
#12493=ORIENTED_EDGE('',*,*,#8836,.T.);
#12494=ORIENTED_EDGE('',*,*,#8827,.T.);
#12495=ORIENTED_EDGE('',*,*,#8836,.F.);
#12496=ORIENTED_EDGE('',*,*,#8837,.F.);
#12497=ORIENTED_EDGE('',*,*,#8838,.T.);
#12498=ORIENTED_EDGE('',*,*,#8839,.T.);
#12499=ORIENTED_EDGE('',*,*,#8838,.F.);
#12500=ORIENTED_EDGE('',*,*,#8840,.F.);
#12501=ORIENTED_EDGE('',*,*,#8841,.T.);
#12502=ORIENTED_EDGE('',*,*,#8842,.T.);
#12503=ORIENTED_EDGE('',*,*,#8841,.F.);
#12504=ORIENTED_EDGE('',*,*,#8840,.T.);
#12505=ORIENTED_EDGE('',*,*,#8837,.T.);
#12506=ORIENTED_EDGE('',*,*,#8842,.F.);
#12507=ORIENTED_EDGE('',*,*,#8839,.F.);
#12508=ORIENTED_EDGE('',*,*,#8843,.F.);
#12509=ORIENTED_EDGE('',*,*,#8844,.T.);
#12510=ORIENTED_EDGE('',*,*,#8845,.T.);
#12511=ORIENTED_EDGE('',*,*,#8844,.F.);
#12512=ORIENTED_EDGE('',*,*,#8846,.F.);
#12513=ORIENTED_EDGE('',*,*,#8847,.T.);
#12514=ORIENTED_EDGE('',*,*,#8848,.T.);
#12515=ORIENTED_EDGE('',*,*,#8847,.F.);
#12516=ORIENTED_EDGE('',*,*,#8846,.T.);
#12517=ORIENTED_EDGE('',*,*,#8843,.T.);
#12518=ORIENTED_EDGE('',*,*,#8848,.F.);
#12519=ORIENTED_EDGE('',*,*,#8845,.F.);
#12520=ORIENTED_EDGE('',*,*,#8849,.F.);
#12521=ORIENTED_EDGE('',*,*,#8850,.F.);
#12522=ORIENTED_EDGE('',*,*,#8851,.F.);
#12523=ORIENTED_EDGE('',*,*,#8852,.F.);
#12524=ORIENTED_EDGE('',*,*,#8853,.F.);
#12525=ORIENTED_EDGE('',*,*,#8854,.F.);
#12526=ORIENTED_EDGE('',*,*,#8855,.F.);
#12527=ORIENTED_EDGE('',*,*,#8856,.F.);
#12528=ORIENTED_EDGE('',*,*,#8856,.T.);
#12529=ORIENTED_EDGE('',*,*,#8857,.F.);
#12530=ORIENTED_EDGE('',*,*,#8850,.T.);
#12531=ORIENTED_EDGE('',*,*,#8858,.F.);
#12532=ORIENTED_EDGE('',*,*,#8853,.T.);
#12533=ORIENTED_EDGE('',*,*,#8858,.T.);
#12534=ORIENTED_EDGE('',*,*,#8849,.T.);
#12535=ORIENTED_EDGE('',*,*,#8859,.F.);
#12536=ORIENTED_EDGE('',*,*,#8855,.T.);
#12537=ORIENTED_EDGE('',*,*,#8860,.F.);
#12538=ORIENTED_EDGE('',*,*,#8851,.T.);
#12539=ORIENTED_EDGE('',*,*,#8857,.T.);
#12540=ORIENTED_EDGE('',*,*,#8854,.T.);
#12541=ORIENTED_EDGE('',*,*,#8859,.T.);
#12542=ORIENTED_EDGE('',*,*,#8852,.T.);
#12543=ORIENTED_EDGE('',*,*,#8860,.T.);
#12544=ORIENTED_EDGE('',*,*,#8861,.T.);
#12545=ORIENTED_EDGE('',*,*,#8862,.T.);
#12546=ORIENTED_EDGE('',*,*,#8863,.F.);
#12547=ORIENTED_EDGE('',*,*,#8864,.F.);
#12548=ORIENTED_EDGE('',*,*,#8865,.T.);
#12549=ORIENTED_EDGE('',*,*,#8864,.T.);
#12550=ORIENTED_EDGE('',*,*,#8866,.F.);
#12551=ORIENTED_EDGE('',*,*,#8867,.F.);
#12552=ORIENTED_EDGE('',*,*,#8868,.T.);
#12553=ORIENTED_EDGE('',*,*,#8867,.T.);
#12554=ORIENTED_EDGE('',*,*,#8869,.F.);
#12555=ORIENTED_EDGE('',*,*,#8870,.F.);
#12556=ORIENTED_EDGE('',*,*,#8871,.T.);
#12557=ORIENTED_EDGE('',*,*,#8870,.T.);
#12558=ORIENTED_EDGE('',*,*,#8872,.F.);
#12559=ORIENTED_EDGE('',*,*,#8862,.F.);
#12560=ORIENTED_EDGE('',*,*,#8872,.T.);
#12561=ORIENTED_EDGE('',*,*,#8869,.T.);
#12562=ORIENTED_EDGE('',*,*,#8866,.T.);
#12563=ORIENTED_EDGE('',*,*,#8863,.T.);
#12564=ORIENTED_EDGE('',*,*,#8871,.F.);
#12565=ORIENTED_EDGE('',*,*,#8861,.F.);
#12566=ORIENTED_EDGE('',*,*,#8865,.F.);
#12567=ORIENTED_EDGE('',*,*,#8868,.F.);
#12568=ORIENTED_EDGE('',*,*,#8873,.F.);
#12569=ORIENTED_EDGE('',*,*,#8874,.T.);
#12570=ORIENTED_EDGE('',*,*,#8875,.T.);
#12571=ORIENTED_EDGE('',*,*,#8876,.T.);
#12572=ORIENTED_EDGE('',*,*,#8877,.F.);
#12573=ORIENTED_EDGE('',*,*,#8878,.T.);
#12574=ORIENTED_EDGE('',*,*,#8873,.T.);
#12575=ORIENTED_EDGE('',*,*,#8879,.T.);
#12576=ORIENTED_EDGE('',*,*,#8880,.F.);
#12577=ORIENTED_EDGE('',*,*,#8881,.T.);
#12578=ORIENTED_EDGE('',*,*,#8877,.T.);
#12579=ORIENTED_EDGE('',*,*,#8882,.T.);
#12580=ORIENTED_EDGE('',*,*,#8883,.F.);
#12581=ORIENTED_EDGE('',*,*,#8884,.T.);
#12582=ORIENTED_EDGE('',*,*,#8880,.T.);
#12583=ORIENTED_EDGE('',*,*,#8885,.T.);
#12584=ORIENTED_EDGE('',*,*,#8886,.F.);
#12585=ORIENTED_EDGE('',*,*,#8887,.T.);
#12586=ORIENTED_EDGE('',*,*,#8883,.T.);
#12587=ORIENTED_EDGE('',*,*,#8888,.T.);
#12588=ORIENTED_EDGE('',*,*,#8889,.F.);
#12589=ORIENTED_EDGE('',*,*,#8890,.T.);
#12590=ORIENTED_EDGE('',*,*,#8886,.T.);
#12591=ORIENTED_EDGE('',*,*,#8891,.T.);
#12592=ORIENTED_EDGE('',*,*,#8892,.F.);
#12593=ORIENTED_EDGE('',*,*,#8893,.T.);
#12594=ORIENTED_EDGE('',*,*,#8889,.T.);
#12595=ORIENTED_EDGE('',*,*,#8894,.T.);
#12596=ORIENTED_EDGE('',*,*,#8895,.F.);
#12597=ORIENTED_EDGE('',*,*,#8896,.T.);
#12598=ORIENTED_EDGE('',*,*,#8892,.T.);
#12599=ORIENTED_EDGE('',*,*,#8897,.T.);
#12600=ORIENTED_EDGE('',*,*,#8898,.F.);
#12601=ORIENTED_EDGE('',*,*,#8899,.T.);
#12602=ORIENTED_EDGE('',*,*,#8895,.T.);
#12603=ORIENTED_EDGE('',*,*,#8900,.T.);
#12604=ORIENTED_EDGE('',*,*,#8901,.F.);
#12605=ORIENTED_EDGE('',*,*,#8902,.T.);
#12606=ORIENTED_EDGE('',*,*,#8898,.T.);
#12607=ORIENTED_EDGE('',*,*,#8903,.T.);
#12608=ORIENTED_EDGE('',*,*,#8904,.F.);
#12609=ORIENTED_EDGE('',*,*,#8905,.T.);
#12610=ORIENTED_EDGE('',*,*,#8901,.T.);
#12611=ORIENTED_EDGE('',*,*,#8906,.T.);
#12612=ORIENTED_EDGE('',*,*,#8907,.F.);
#12613=ORIENTED_EDGE('',*,*,#8908,.T.);
#12614=ORIENTED_EDGE('',*,*,#8904,.T.);
#12615=ORIENTED_EDGE('',*,*,#8909,.T.);
#12616=ORIENTED_EDGE('',*,*,#8910,.F.);
#12617=ORIENTED_EDGE('',*,*,#8911,.T.);
#12618=ORIENTED_EDGE('',*,*,#8907,.T.);
#12619=ORIENTED_EDGE('',*,*,#8912,.T.);
#12620=ORIENTED_EDGE('',*,*,#8913,.F.);
#12621=ORIENTED_EDGE('',*,*,#8914,.T.);
#12622=ORIENTED_EDGE('',*,*,#8910,.T.);
#12623=ORIENTED_EDGE('',*,*,#8915,.T.);
#12624=ORIENTED_EDGE('',*,*,#8916,.F.);
#12625=ORIENTED_EDGE('',*,*,#8917,.T.);
#12626=ORIENTED_EDGE('',*,*,#8913,.T.);
#12627=ORIENTED_EDGE('',*,*,#8918,.T.);
#12628=ORIENTED_EDGE('',*,*,#8919,.F.);
#12629=ORIENTED_EDGE('',*,*,#8920,.T.);
#12630=ORIENTED_EDGE('',*,*,#8916,.T.);
#12631=ORIENTED_EDGE('',*,*,#8921,.T.);
#12632=ORIENTED_EDGE('',*,*,#8922,.F.);
#12633=ORIENTED_EDGE('',*,*,#8923,.T.);
#12634=ORIENTED_EDGE('',*,*,#8919,.T.);
#12635=ORIENTED_EDGE('',*,*,#8924,.T.);
#12636=ORIENTED_EDGE('',*,*,#8925,.F.);
#12637=ORIENTED_EDGE('',*,*,#8926,.T.);
#12638=ORIENTED_EDGE('',*,*,#8922,.T.);
#12639=ORIENTED_EDGE('',*,*,#8927,.T.);
#12640=ORIENTED_EDGE('',*,*,#8928,.F.);
#12641=ORIENTED_EDGE('',*,*,#8929,.T.);
#12642=ORIENTED_EDGE('',*,*,#8925,.T.);
#12643=ORIENTED_EDGE('',*,*,#8930,.T.);
#12644=ORIENTED_EDGE('',*,*,#8931,.F.);
#12645=ORIENTED_EDGE('',*,*,#8932,.T.);
#12646=ORIENTED_EDGE('',*,*,#8928,.T.);
#12647=ORIENTED_EDGE('',*,*,#8933,.T.);
#12648=ORIENTED_EDGE('',*,*,#8934,.F.);
#12649=ORIENTED_EDGE('',*,*,#8935,.T.);
#12650=ORIENTED_EDGE('',*,*,#8931,.T.);
#12651=ORIENTED_EDGE('',*,*,#8936,.T.);
#12652=ORIENTED_EDGE('',*,*,#8937,.F.);
#12653=ORIENTED_EDGE('',*,*,#8938,.T.);
#12654=ORIENTED_EDGE('',*,*,#8934,.T.);
#12655=ORIENTED_EDGE('',*,*,#8939,.T.);
#12656=ORIENTED_EDGE('',*,*,#8940,.F.);
#12657=ORIENTED_EDGE('',*,*,#8941,.T.);
#12658=ORIENTED_EDGE('',*,*,#8937,.T.);
#12659=ORIENTED_EDGE('',*,*,#8942,.T.);
#12660=ORIENTED_EDGE('',*,*,#8943,.F.);
#12661=ORIENTED_EDGE('',*,*,#8944,.T.);
#12662=ORIENTED_EDGE('',*,*,#8940,.T.);
#12663=ORIENTED_EDGE('',*,*,#8945,.T.);
#12664=ORIENTED_EDGE('',*,*,#8946,.F.);
#12665=ORIENTED_EDGE('',*,*,#8947,.T.);
#12666=ORIENTED_EDGE('',*,*,#8943,.T.);
#12667=ORIENTED_EDGE('',*,*,#8948,.T.);
#12668=ORIENTED_EDGE('',*,*,#8949,.F.);
#12669=ORIENTED_EDGE('',*,*,#8950,.T.);
#12670=ORIENTED_EDGE('',*,*,#8946,.T.);
#12671=ORIENTED_EDGE('',*,*,#8951,.T.);
#12672=ORIENTED_EDGE('',*,*,#8952,.F.);
#12673=ORIENTED_EDGE('',*,*,#8953,.T.);
#12674=ORIENTED_EDGE('',*,*,#8949,.T.);
#12675=ORIENTED_EDGE('',*,*,#8954,.T.);
#12676=ORIENTED_EDGE('',*,*,#8955,.F.);
#12677=ORIENTED_EDGE('',*,*,#8956,.T.);
#12678=ORIENTED_EDGE('',*,*,#8952,.T.);
#12679=ORIENTED_EDGE('',*,*,#8957,.T.);
#12680=ORIENTED_EDGE('',*,*,#8958,.F.);
#12681=ORIENTED_EDGE('',*,*,#8959,.T.);
#12682=ORIENTED_EDGE('',*,*,#8955,.T.);
#12683=ORIENTED_EDGE('',*,*,#8960,.T.);
#12684=ORIENTED_EDGE('',*,*,#8961,.F.);
#12685=ORIENTED_EDGE('',*,*,#8962,.T.);
#12686=ORIENTED_EDGE('',*,*,#8958,.T.);
#12687=ORIENTED_EDGE('',*,*,#8963,.T.);
#12688=ORIENTED_EDGE('',*,*,#8964,.F.);
#12689=ORIENTED_EDGE('',*,*,#8965,.T.);
#12690=ORIENTED_EDGE('',*,*,#8961,.T.);
#12691=ORIENTED_EDGE('',*,*,#8966,.T.);
#12692=ORIENTED_EDGE('',*,*,#8967,.F.);
#12693=ORIENTED_EDGE('',*,*,#8968,.T.);
#12694=ORIENTED_EDGE('',*,*,#8964,.T.);
#12695=ORIENTED_EDGE('',*,*,#8969,.T.);
#12696=ORIENTED_EDGE('',*,*,#8970,.F.);
#12697=ORIENTED_EDGE('',*,*,#8971,.T.);
#12698=ORIENTED_EDGE('',*,*,#8967,.T.);
#12699=ORIENTED_EDGE('',*,*,#8972,.T.);
#12700=ORIENTED_EDGE('',*,*,#8973,.F.);
#12701=ORIENTED_EDGE('',*,*,#8974,.T.);
#12702=ORIENTED_EDGE('',*,*,#8970,.T.);
#12703=ORIENTED_EDGE('',*,*,#8975,.T.);
#12704=ORIENTED_EDGE('',*,*,#8976,.F.);
#12705=ORIENTED_EDGE('',*,*,#8977,.T.);
#12706=ORIENTED_EDGE('',*,*,#8973,.T.);
#12707=ORIENTED_EDGE('',*,*,#8978,.T.);
#12708=ORIENTED_EDGE('',*,*,#8979,.F.);
#12709=ORIENTED_EDGE('',*,*,#8980,.T.);
#12710=ORIENTED_EDGE('',*,*,#8976,.T.);
#12711=ORIENTED_EDGE('',*,*,#8981,.T.);
#12712=ORIENTED_EDGE('',*,*,#8982,.F.);
#12713=ORIENTED_EDGE('',*,*,#8983,.T.);
#12714=ORIENTED_EDGE('',*,*,#8979,.T.);
#12715=ORIENTED_EDGE('',*,*,#8984,.T.);
#12716=ORIENTED_EDGE('',*,*,#8985,.F.);
#12717=ORIENTED_EDGE('',*,*,#8986,.T.);
#12718=ORIENTED_EDGE('',*,*,#8982,.T.);
#12719=ORIENTED_EDGE('',*,*,#8987,.T.);
#12720=ORIENTED_EDGE('',*,*,#8988,.F.);
#12721=ORIENTED_EDGE('',*,*,#8989,.T.);
#12722=ORIENTED_EDGE('',*,*,#8985,.T.);
#12723=ORIENTED_EDGE('',*,*,#8990,.T.);
#12724=ORIENTED_EDGE('',*,*,#8991,.F.);
#12725=ORIENTED_EDGE('',*,*,#8992,.T.);
#12726=ORIENTED_EDGE('',*,*,#8988,.T.);
#12727=ORIENTED_EDGE('',*,*,#8993,.T.);
#12728=ORIENTED_EDGE('',*,*,#8994,.F.);
#12729=ORIENTED_EDGE('',*,*,#8995,.T.);
#12730=ORIENTED_EDGE('',*,*,#8991,.T.);
#12731=ORIENTED_EDGE('',*,*,#8996,.T.);
#12732=ORIENTED_EDGE('',*,*,#8997,.F.);
#12733=ORIENTED_EDGE('',*,*,#8998,.T.);
#12734=ORIENTED_EDGE('',*,*,#8994,.T.);
#12735=ORIENTED_EDGE('',*,*,#8999,.T.);
#12736=ORIENTED_EDGE('',*,*,#9000,.F.);
#12737=ORIENTED_EDGE('',*,*,#9001,.T.);
#12738=ORIENTED_EDGE('',*,*,#8997,.T.);
#12739=ORIENTED_EDGE('',*,*,#9002,.T.);
#12740=ORIENTED_EDGE('',*,*,#9003,.F.);
#12741=ORIENTED_EDGE('',*,*,#9004,.T.);
#12742=ORIENTED_EDGE('',*,*,#9000,.T.);
#12743=ORIENTED_EDGE('',*,*,#9005,.T.);
#12744=ORIENTED_EDGE('',*,*,#9006,.F.);
#12745=ORIENTED_EDGE('',*,*,#9007,.T.);
#12746=ORIENTED_EDGE('',*,*,#9003,.T.);
#12747=ORIENTED_EDGE('',*,*,#9008,.T.);
#12748=ORIENTED_EDGE('',*,*,#9009,.F.);
#12749=ORIENTED_EDGE('',*,*,#9010,.T.);
#12750=ORIENTED_EDGE('',*,*,#9006,.T.);
#12751=ORIENTED_EDGE('',*,*,#9011,.T.);
#12752=ORIENTED_EDGE('',*,*,#9012,.F.);
#12753=ORIENTED_EDGE('',*,*,#9013,.T.);
#12754=ORIENTED_EDGE('',*,*,#9009,.T.);
#12755=ORIENTED_EDGE('',*,*,#9014,.T.);
#12756=ORIENTED_EDGE('',*,*,#9015,.F.);
#12757=ORIENTED_EDGE('',*,*,#9016,.T.);
#12758=ORIENTED_EDGE('',*,*,#9012,.T.);
#12759=ORIENTED_EDGE('',*,*,#9017,.T.);
#12760=ORIENTED_EDGE('',*,*,#9018,.F.);
#12761=ORIENTED_EDGE('',*,*,#9019,.T.);
#12762=ORIENTED_EDGE('',*,*,#9015,.T.);
#12763=ORIENTED_EDGE('',*,*,#9020,.T.);
#12764=ORIENTED_EDGE('',*,*,#9021,.F.);
#12765=ORIENTED_EDGE('',*,*,#9022,.T.);
#12766=ORIENTED_EDGE('',*,*,#9018,.T.);
#12767=ORIENTED_EDGE('',*,*,#9023,.T.);
#12768=ORIENTED_EDGE('',*,*,#9024,.F.);
#12769=ORIENTED_EDGE('',*,*,#9025,.T.);
#12770=ORIENTED_EDGE('',*,*,#9021,.T.);
#12771=ORIENTED_EDGE('',*,*,#9026,.T.);
#12772=ORIENTED_EDGE('',*,*,#9027,.F.);
#12773=ORIENTED_EDGE('',*,*,#9028,.T.);
#12774=ORIENTED_EDGE('',*,*,#9024,.T.);
#12775=ORIENTED_EDGE('',*,*,#9029,.T.);
#12776=ORIENTED_EDGE('',*,*,#9030,.F.);
#12777=ORIENTED_EDGE('',*,*,#9031,.T.);
#12778=ORIENTED_EDGE('',*,*,#9027,.T.);
#12779=ORIENTED_EDGE('',*,*,#9032,.T.);
#12780=ORIENTED_EDGE('',*,*,#9033,.F.);
#12781=ORIENTED_EDGE('',*,*,#9034,.T.);
#12782=ORIENTED_EDGE('',*,*,#9030,.T.);
#12783=ORIENTED_EDGE('',*,*,#9035,.T.);
#12784=ORIENTED_EDGE('',*,*,#9036,.F.);
#12785=ORIENTED_EDGE('',*,*,#9037,.T.);
#12786=ORIENTED_EDGE('',*,*,#9033,.T.);
#12787=ORIENTED_EDGE('',*,*,#9038,.T.);
#12788=ORIENTED_EDGE('',*,*,#9039,.F.);
#12789=ORIENTED_EDGE('',*,*,#9040,.T.);
#12790=ORIENTED_EDGE('',*,*,#9036,.T.);
#12791=ORIENTED_EDGE('',*,*,#9041,.T.);
#12792=ORIENTED_EDGE('',*,*,#9042,.F.);
#12793=ORIENTED_EDGE('',*,*,#9043,.T.);
#12794=ORIENTED_EDGE('',*,*,#9039,.T.);
#12795=ORIENTED_EDGE('',*,*,#9044,.T.);
#12796=ORIENTED_EDGE('',*,*,#9045,.F.);
#12797=ORIENTED_EDGE('',*,*,#9046,.T.);
#12798=ORIENTED_EDGE('',*,*,#9042,.T.);
#12799=ORIENTED_EDGE('',*,*,#9047,.T.);
#12800=ORIENTED_EDGE('',*,*,#9048,.F.);
#12801=ORIENTED_EDGE('',*,*,#9049,.T.);
#12802=ORIENTED_EDGE('',*,*,#9045,.T.);
#12803=ORIENTED_EDGE('',*,*,#9050,.T.);
#12804=ORIENTED_EDGE('',*,*,#9051,.F.);
#12805=ORIENTED_EDGE('',*,*,#9052,.T.);
#12806=ORIENTED_EDGE('',*,*,#9048,.T.);
#12807=ORIENTED_EDGE('',*,*,#9053,.T.);
#12808=ORIENTED_EDGE('',*,*,#9054,.F.);
#12809=ORIENTED_EDGE('',*,*,#9055,.T.);
#12810=ORIENTED_EDGE('',*,*,#9051,.T.);
#12811=ORIENTED_EDGE('',*,*,#9056,.T.);
#12812=ORIENTED_EDGE('',*,*,#9057,.F.);
#12813=ORIENTED_EDGE('',*,*,#9058,.T.);
#12814=ORIENTED_EDGE('',*,*,#9054,.T.);
#12815=ORIENTED_EDGE('',*,*,#9059,.T.);
#12816=ORIENTED_EDGE('',*,*,#9060,.F.);
#12817=ORIENTED_EDGE('',*,*,#9061,.T.);
#12818=ORIENTED_EDGE('',*,*,#9057,.T.);
#12819=ORIENTED_EDGE('',*,*,#9062,.T.);
#12820=ORIENTED_EDGE('',*,*,#9063,.F.);
#12821=ORIENTED_EDGE('',*,*,#9064,.T.);
#12822=ORIENTED_EDGE('',*,*,#9060,.T.);
#12823=ORIENTED_EDGE('',*,*,#9065,.T.);
#12824=ORIENTED_EDGE('',*,*,#9066,.F.);
#12825=ORIENTED_EDGE('',*,*,#9067,.T.);
#12826=ORIENTED_EDGE('',*,*,#9063,.T.);
#12827=ORIENTED_EDGE('',*,*,#9068,.T.);
#12828=ORIENTED_EDGE('',*,*,#9069,.F.);
#12829=ORIENTED_EDGE('',*,*,#9070,.T.);
#12830=ORIENTED_EDGE('',*,*,#9066,.T.);
#12831=ORIENTED_EDGE('',*,*,#9071,.T.);
#12832=ORIENTED_EDGE('',*,*,#9072,.F.);
#12833=ORIENTED_EDGE('',*,*,#9073,.T.);
#12834=ORIENTED_EDGE('',*,*,#9069,.T.);
#12835=ORIENTED_EDGE('',*,*,#9074,.T.);
#12836=ORIENTED_EDGE('',*,*,#9075,.F.);
#12837=ORIENTED_EDGE('',*,*,#9076,.T.);
#12838=ORIENTED_EDGE('',*,*,#9072,.T.);
#12839=ORIENTED_EDGE('',*,*,#9077,.T.);
#12840=ORIENTED_EDGE('',*,*,#9078,.F.);
#12841=ORIENTED_EDGE('',*,*,#9079,.T.);
#12842=ORIENTED_EDGE('',*,*,#9075,.T.);
#12843=ORIENTED_EDGE('',*,*,#9080,.T.);
#12844=ORIENTED_EDGE('',*,*,#9081,.F.);
#12845=ORIENTED_EDGE('',*,*,#9082,.T.);
#12846=ORIENTED_EDGE('',*,*,#9078,.T.);
#12847=ORIENTED_EDGE('',*,*,#9083,.T.);
#12848=ORIENTED_EDGE('',*,*,#9084,.F.);
#12849=ORIENTED_EDGE('',*,*,#9085,.T.);
#12850=ORIENTED_EDGE('',*,*,#9081,.T.);
#12851=ORIENTED_EDGE('',*,*,#9086,.T.);
#12852=ORIENTED_EDGE('',*,*,#9087,.F.);
#12853=ORIENTED_EDGE('',*,*,#9088,.T.);
#12854=ORIENTED_EDGE('',*,*,#9084,.T.);
#12855=ORIENTED_EDGE('',*,*,#9089,.T.);
#12856=ORIENTED_EDGE('',*,*,#9090,.F.);
#12857=ORIENTED_EDGE('',*,*,#9091,.T.);
#12858=ORIENTED_EDGE('',*,*,#9087,.T.);
#12859=ORIENTED_EDGE('',*,*,#9092,.T.);
#12860=ORIENTED_EDGE('',*,*,#9093,.F.);
#12861=ORIENTED_EDGE('',*,*,#9094,.T.);
#12862=ORIENTED_EDGE('',*,*,#9090,.T.);
#12863=ORIENTED_EDGE('',*,*,#9095,.T.);
#12864=ORIENTED_EDGE('',*,*,#9096,.F.);
#12865=ORIENTED_EDGE('',*,*,#9097,.T.);
#12866=ORIENTED_EDGE('',*,*,#9093,.T.);
#12867=ORIENTED_EDGE('',*,*,#9098,.T.);
#12868=ORIENTED_EDGE('',*,*,#9099,.F.);
#12869=ORIENTED_EDGE('',*,*,#9100,.T.);
#12870=ORIENTED_EDGE('',*,*,#9096,.T.);
#12871=ORIENTED_EDGE('',*,*,#9101,.T.);
#12872=ORIENTED_EDGE('',*,*,#9102,.F.);
#12873=ORIENTED_EDGE('',*,*,#9103,.T.);
#12874=ORIENTED_EDGE('',*,*,#9099,.T.);
#12875=ORIENTED_EDGE('',*,*,#9104,.T.);
#12876=ORIENTED_EDGE('',*,*,#9105,.F.);
#12877=ORIENTED_EDGE('',*,*,#9106,.T.);
#12878=ORIENTED_EDGE('',*,*,#9102,.T.);
#12879=ORIENTED_EDGE('',*,*,#9107,.T.);
#12880=ORIENTED_EDGE('',*,*,#9108,.T.);
#12881=ORIENTED_EDGE('',*,*,#9109,.T.);
#12882=ORIENTED_EDGE('',*,*,#9110,.T.);
#12883=ORIENTED_EDGE('',*,*,#9111,.T.);
#12884=ORIENTED_EDGE('',*,*,#9112,.T.);
#12885=ORIENTED_EDGE('',*,*,#9113,.T.);
#12886=ORIENTED_EDGE('',*,*,#9114,.T.);
#12887=ORIENTED_EDGE('',*,*,#9109,.F.);
#12888=ORIENTED_EDGE('',*,*,#9115,.F.);
#12889=ORIENTED_EDGE('',*,*,#9116,.T.);
#12890=ORIENTED_EDGE('',*,*,#9117,.F.);
#12891=ORIENTED_EDGE('',*,*,#9118,.F.);
#12892=ORIENTED_EDGE('',*,*,#9119,.F.);
#12893=ORIENTED_EDGE('',*,*,#9120,.T.);
#12894=ORIENTED_EDGE('',*,*,#9115,.T.);
#12895=ORIENTED_EDGE('',*,*,#9121,.F.);
#12896=ORIENTED_EDGE('',*,*,#9122,.F.);
#12897=ORIENTED_EDGE('',*,*,#9123,.T.);
#12898=ORIENTED_EDGE('',*,*,#9119,.T.);
#12899=ORIENTED_EDGE('',*,*,#9124,.F.);
#12900=ORIENTED_EDGE('',*,*,#9125,.F.);
#12901=ORIENTED_EDGE('',*,*,#9126,.T.);
#12902=ORIENTED_EDGE('',*,*,#9122,.T.);
#12903=ORIENTED_EDGE('',*,*,#9127,.F.);
#12904=ORIENTED_EDGE('',*,*,#9128,.F.);
#12905=ORIENTED_EDGE('',*,*,#9129,.T.);
#12906=ORIENTED_EDGE('',*,*,#9125,.T.);
#12907=ORIENTED_EDGE('',*,*,#9130,.F.);
#12908=ORIENTED_EDGE('',*,*,#9131,.F.);
#12909=ORIENTED_EDGE('',*,*,#9132,.T.);
#12910=ORIENTED_EDGE('',*,*,#9128,.T.);
#12911=ORIENTED_EDGE('',*,*,#9133,.F.);
#12912=ORIENTED_EDGE('',*,*,#9134,.F.);
#12913=ORIENTED_EDGE('',*,*,#9135,.T.);
#12914=ORIENTED_EDGE('',*,*,#9131,.T.);
#12915=ORIENTED_EDGE('',*,*,#9136,.F.);
#12916=ORIENTED_EDGE('',*,*,#9137,.F.);
#12917=ORIENTED_EDGE('',*,*,#9138,.T.);
#12918=ORIENTED_EDGE('',*,*,#9134,.T.);
#12919=ORIENTED_EDGE('',*,*,#9139,.F.);
#12920=ORIENTED_EDGE('',*,*,#9140,.F.);
#12921=ORIENTED_EDGE('',*,*,#9141,.T.);
#12922=ORIENTED_EDGE('',*,*,#9137,.T.);
#12923=ORIENTED_EDGE('',*,*,#9142,.F.);
#12924=ORIENTED_EDGE('',*,*,#9143,.F.);
#12925=ORIENTED_EDGE('',*,*,#9144,.T.);
#12926=ORIENTED_EDGE('',*,*,#9140,.T.);
#12927=ORIENTED_EDGE('',*,*,#9145,.F.);
#12928=ORIENTED_EDGE('',*,*,#9146,.F.);
#12929=ORIENTED_EDGE('',*,*,#9147,.T.);
#12930=ORIENTED_EDGE('',*,*,#9143,.T.);
#12931=ORIENTED_EDGE('',*,*,#9148,.F.);
#12932=ORIENTED_EDGE('',*,*,#9149,.F.);
#12933=ORIENTED_EDGE('',*,*,#9150,.T.);
#12934=ORIENTED_EDGE('',*,*,#9146,.T.);
#12935=ORIENTED_EDGE('',*,*,#9151,.F.);
#12936=ORIENTED_EDGE('',*,*,#9152,.F.);
#12937=ORIENTED_EDGE('',*,*,#9153,.T.);
#12938=ORIENTED_EDGE('',*,*,#9149,.T.);
#12939=ORIENTED_EDGE('',*,*,#9154,.F.);
#12940=ORIENTED_EDGE('',*,*,#9155,.F.);
#12941=ORIENTED_EDGE('',*,*,#9156,.T.);
#12942=ORIENTED_EDGE('',*,*,#9152,.T.);
#12943=ORIENTED_EDGE('',*,*,#9157,.F.);
#12944=ORIENTED_EDGE('',*,*,#9158,.F.);
#12945=ORIENTED_EDGE('',*,*,#9159,.T.);
#12946=ORIENTED_EDGE('',*,*,#9155,.T.);
#12947=ORIENTED_EDGE('',*,*,#9160,.F.);
#12948=ORIENTED_EDGE('',*,*,#9161,.F.);
#12949=ORIENTED_EDGE('',*,*,#9162,.T.);
#12950=ORIENTED_EDGE('',*,*,#9158,.T.);
#12951=ORIENTED_EDGE('',*,*,#9163,.F.);
#12952=ORIENTED_EDGE('',*,*,#9164,.F.);
#12953=ORIENTED_EDGE('',*,*,#9165,.T.);
#12954=ORIENTED_EDGE('',*,*,#9161,.T.);
#12955=ORIENTED_EDGE('',*,*,#9166,.F.);
#12956=ORIENTED_EDGE('',*,*,#9167,.F.);
#12957=ORIENTED_EDGE('',*,*,#9168,.T.);
#12958=ORIENTED_EDGE('',*,*,#9164,.T.);
#12959=ORIENTED_EDGE('',*,*,#9169,.F.);
#12960=ORIENTED_EDGE('',*,*,#9170,.F.);
#12961=ORIENTED_EDGE('',*,*,#9171,.T.);
#12962=ORIENTED_EDGE('',*,*,#9167,.T.);
#12963=ORIENTED_EDGE('',*,*,#9172,.F.);
#12964=ORIENTED_EDGE('',*,*,#9173,.F.);
#12965=ORIENTED_EDGE('',*,*,#9174,.T.);
#12966=ORIENTED_EDGE('',*,*,#9170,.T.);
#12967=ORIENTED_EDGE('',*,*,#9175,.F.);
#12968=ORIENTED_EDGE('',*,*,#9176,.F.);
#12969=ORIENTED_EDGE('',*,*,#9177,.T.);
#12970=ORIENTED_EDGE('',*,*,#9173,.T.);
#12971=ORIENTED_EDGE('',*,*,#9178,.F.);
#12972=ORIENTED_EDGE('',*,*,#9179,.F.);
#12973=ORIENTED_EDGE('',*,*,#9180,.T.);
#12974=ORIENTED_EDGE('',*,*,#9176,.T.);
#12975=ORIENTED_EDGE('',*,*,#9181,.F.);
#12976=ORIENTED_EDGE('',*,*,#9182,.F.);
#12977=ORIENTED_EDGE('',*,*,#9183,.T.);
#12978=ORIENTED_EDGE('',*,*,#9179,.T.);
#12979=ORIENTED_EDGE('',*,*,#9184,.F.);
#12980=ORIENTED_EDGE('',*,*,#9185,.F.);
#12981=ORIENTED_EDGE('',*,*,#9186,.T.);
#12982=ORIENTED_EDGE('',*,*,#9182,.T.);
#12983=ORIENTED_EDGE('',*,*,#9187,.F.);
#12984=ORIENTED_EDGE('',*,*,#9188,.F.);
#12985=ORIENTED_EDGE('',*,*,#9189,.T.);
#12986=ORIENTED_EDGE('',*,*,#9185,.T.);
#12987=ORIENTED_EDGE('',*,*,#9190,.F.);
#12988=ORIENTED_EDGE('',*,*,#9191,.F.);
#12989=ORIENTED_EDGE('',*,*,#9192,.T.);
#12990=ORIENTED_EDGE('',*,*,#9188,.T.);
#12991=ORIENTED_EDGE('',*,*,#9193,.F.);
#12992=ORIENTED_EDGE('',*,*,#9194,.F.);
#12993=ORIENTED_EDGE('',*,*,#9195,.T.);
#12994=ORIENTED_EDGE('',*,*,#9191,.T.);
#12995=ORIENTED_EDGE('',*,*,#9196,.F.);
#12996=ORIENTED_EDGE('',*,*,#9197,.F.);
#12997=ORIENTED_EDGE('',*,*,#9198,.T.);
#12998=ORIENTED_EDGE('',*,*,#9194,.T.);
#12999=ORIENTED_EDGE('',*,*,#9199,.F.);
#13000=ORIENTED_EDGE('',*,*,#9200,.F.);
#13001=ORIENTED_EDGE('',*,*,#9201,.T.);
#13002=ORIENTED_EDGE('',*,*,#9197,.T.);
#13003=ORIENTED_EDGE('',*,*,#9202,.F.);
#13004=ORIENTED_EDGE('',*,*,#9203,.F.);
#13005=ORIENTED_EDGE('',*,*,#9204,.T.);
#13006=ORIENTED_EDGE('',*,*,#9200,.T.);
#13007=ORIENTED_EDGE('',*,*,#9205,.F.);
#13008=ORIENTED_EDGE('',*,*,#9206,.F.);
#13009=ORIENTED_EDGE('',*,*,#9207,.T.);
#13010=ORIENTED_EDGE('',*,*,#9203,.T.);
#13011=ORIENTED_EDGE('',*,*,#9208,.F.);
#13012=ORIENTED_EDGE('',*,*,#9209,.F.);
#13013=ORIENTED_EDGE('',*,*,#9210,.T.);
#13014=ORIENTED_EDGE('',*,*,#9206,.T.);
#13015=ORIENTED_EDGE('',*,*,#9211,.F.);
#13016=ORIENTED_EDGE('',*,*,#9212,.F.);
#13017=ORIENTED_EDGE('',*,*,#9213,.T.);
#13018=ORIENTED_EDGE('',*,*,#9209,.T.);
#13019=ORIENTED_EDGE('',*,*,#9214,.F.);
#13020=ORIENTED_EDGE('',*,*,#9215,.F.);
#13021=ORIENTED_EDGE('',*,*,#9216,.T.);
#13022=ORIENTED_EDGE('',*,*,#9212,.T.);
#13023=ORIENTED_EDGE('',*,*,#9217,.F.);
#13024=ORIENTED_EDGE('',*,*,#9218,.F.);
#13025=ORIENTED_EDGE('',*,*,#9219,.T.);
#13026=ORIENTED_EDGE('',*,*,#9215,.T.);
#13027=ORIENTED_EDGE('',*,*,#9220,.F.);
#13028=ORIENTED_EDGE('',*,*,#9221,.F.);
#13029=ORIENTED_EDGE('',*,*,#9222,.T.);
#13030=ORIENTED_EDGE('',*,*,#9218,.T.);
#13031=ORIENTED_EDGE('',*,*,#9223,.F.);
#13032=ORIENTED_EDGE('',*,*,#9224,.F.);
#13033=ORIENTED_EDGE('',*,*,#9225,.T.);
#13034=ORIENTED_EDGE('',*,*,#9221,.T.);
#13035=ORIENTED_EDGE('',*,*,#9226,.F.);
#13036=ORIENTED_EDGE('',*,*,#9227,.F.);
#13037=ORIENTED_EDGE('',*,*,#9228,.T.);
#13038=ORIENTED_EDGE('',*,*,#9224,.T.);
#13039=ORIENTED_EDGE('',*,*,#9229,.F.);
#13040=ORIENTED_EDGE('',*,*,#9230,.F.);
#13041=ORIENTED_EDGE('',*,*,#9231,.T.);
#13042=ORIENTED_EDGE('',*,*,#9227,.T.);
#13043=ORIENTED_EDGE('',*,*,#9232,.F.);
#13044=ORIENTED_EDGE('',*,*,#9233,.F.);
#13045=ORIENTED_EDGE('',*,*,#9234,.T.);
#13046=ORIENTED_EDGE('',*,*,#9230,.T.);
#13047=ORIENTED_EDGE('',*,*,#9235,.F.);
#13048=ORIENTED_EDGE('',*,*,#9236,.F.);
#13049=ORIENTED_EDGE('',*,*,#9237,.T.);
#13050=ORIENTED_EDGE('',*,*,#9233,.T.);
#13051=ORIENTED_EDGE('',*,*,#9238,.F.);
#13052=ORIENTED_EDGE('',*,*,#9239,.F.);
#13053=ORIENTED_EDGE('',*,*,#9240,.T.);
#13054=ORIENTED_EDGE('',*,*,#9236,.T.);
#13055=ORIENTED_EDGE('',*,*,#9241,.F.);
#13056=ORIENTED_EDGE('',*,*,#9242,.F.);
#13057=ORIENTED_EDGE('',*,*,#9243,.T.);
#13058=ORIENTED_EDGE('',*,*,#9239,.T.);
#13059=ORIENTED_EDGE('',*,*,#9244,.F.);
#13060=ORIENTED_EDGE('',*,*,#9245,.F.);
#13061=ORIENTED_EDGE('',*,*,#9246,.T.);
#13062=ORIENTED_EDGE('',*,*,#9242,.T.);
#13063=ORIENTED_EDGE('',*,*,#9247,.F.);
#13064=ORIENTED_EDGE('',*,*,#9248,.F.);
#13065=ORIENTED_EDGE('',*,*,#9249,.T.);
#13066=ORIENTED_EDGE('',*,*,#9245,.T.);
#13067=ORIENTED_EDGE('',*,*,#9250,.F.);
#13068=ORIENTED_EDGE('',*,*,#9251,.F.);
#13069=ORIENTED_EDGE('',*,*,#9252,.T.);
#13070=ORIENTED_EDGE('',*,*,#9248,.T.);
#13071=ORIENTED_EDGE('',*,*,#9253,.F.);
#13072=ORIENTED_EDGE('',*,*,#9254,.F.);
#13073=ORIENTED_EDGE('',*,*,#9255,.T.);
#13074=ORIENTED_EDGE('',*,*,#9251,.T.);
#13075=ORIENTED_EDGE('',*,*,#9256,.F.);
#13076=ORIENTED_EDGE('',*,*,#9257,.F.);
#13077=ORIENTED_EDGE('',*,*,#9258,.T.);
#13078=ORIENTED_EDGE('',*,*,#9254,.T.);
#13079=ORIENTED_EDGE('',*,*,#9259,.F.);
#13080=ORIENTED_EDGE('',*,*,#9260,.F.);
#13081=ORIENTED_EDGE('',*,*,#9261,.T.);
#13082=ORIENTED_EDGE('',*,*,#9257,.T.);
#13083=ORIENTED_EDGE('',*,*,#9262,.F.);
#13084=ORIENTED_EDGE('',*,*,#9263,.F.);
#13085=ORIENTED_EDGE('',*,*,#9264,.T.);
#13086=ORIENTED_EDGE('',*,*,#9260,.T.);
#13087=ORIENTED_EDGE('',*,*,#9265,.F.);
#13088=ORIENTED_EDGE('',*,*,#9266,.F.);
#13089=ORIENTED_EDGE('',*,*,#9267,.T.);
#13090=ORIENTED_EDGE('',*,*,#9263,.T.);
#13091=ORIENTED_EDGE('',*,*,#9268,.F.);
#13092=ORIENTED_EDGE('',*,*,#9269,.F.);
#13093=ORIENTED_EDGE('',*,*,#9270,.T.);
#13094=ORIENTED_EDGE('',*,*,#9266,.T.);
#13095=ORIENTED_EDGE('',*,*,#9271,.F.);
#13096=ORIENTED_EDGE('',*,*,#9272,.F.);
#13097=ORIENTED_EDGE('',*,*,#9273,.T.);
#13098=ORIENTED_EDGE('',*,*,#9269,.T.);
#13099=ORIENTED_EDGE('',*,*,#9274,.F.);
#13100=ORIENTED_EDGE('',*,*,#9275,.F.);
#13101=ORIENTED_EDGE('',*,*,#9276,.T.);
#13102=ORIENTED_EDGE('',*,*,#9272,.T.);
#13103=ORIENTED_EDGE('',*,*,#9277,.F.);
#13104=ORIENTED_EDGE('',*,*,#9278,.F.);
#13105=ORIENTED_EDGE('',*,*,#9279,.T.);
#13106=ORIENTED_EDGE('',*,*,#9275,.T.);
#13107=ORIENTED_EDGE('',*,*,#9280,.F.);
#13108=ORIENTED_EDGE('',*,*,#9281,.F.);
#13109=ORIENTED_EDGE('',*,*,#9282,.T.);
#13110=ORIENTED_EDGE('',*,*,#9278,.T.);
#13111=ORIENTED_EDGE('',*,*,#9283,.F.);
#13112=ORIENTED_EDGE('',*,*,#9284,.F.);
#13113=ORIENTED_EDGE('',*,*,#9285,.T.);
#13114=ORIENTED_EDGE('',*,*,#9281,.T.);
#13115=ORIENTED_EDGE('',*,*,#9286,.F.);
#13116=ORIENTED_EDGE('',*,*,#9287,.F.);
#13117=ORIENTED_EDGE('',*,*,#9288,.T.);
#13118=ORIENTED_EDGE('',*,*,#9284,.T.);
#13119=ORIENTED_EDGE('',*,*,#9289,.F.);
#13120=ORIENTED_EDGE('',*,*,#9290,.F.);
#13121=ORIENTED_EDGE('',*,*,#9291,.T.);
#13122=ORIENTED_EDGE('',*,*,#9287,.T.);
#13123=ORIENTED_EDGE('',*,*,#9292,.F.);
#13124=ORIENTED_EDGE('',*,*,#9293,.F.);
#13125=ORIENTED_EDGE('',*,*,#9294,.T.);
#13126=ORIENTED_EDGE('',*,*,#9290,.T.);
#13127=ORIENTED_EDGE('',*,*,#9295,.F.);
#13128=ORIENTED_EDGE('',*,*,#9296,.F.);
#13129=ORIENTED_EDGE('',*,*,#9297,.T.);
#13130=ORIENTED_EDGE('',*,*,#9293,.T.);
#13131=ORIENTED_EDGE('',*,*,#9298,.F.);
#13132=ORIENTED_EDGE('',*,*,#9299,.F.);
#13133=ORIENTED_EDGE('',*,*,#9300,.T.);
#13134=ORIENTED_EDGE('',*,*,#9296,.T.);
#13135=ORIENTED_EDGE('',*,*,#9301,.F.);
#13136=ORIENTED_EDGE('',*,*,#9302,.F.);
#13137=ORIENTED_EDGE('',*,*,#9303,.T.);
#13138=ORIENTED_EDGE('',*,*,#9299,.T.);
#13139=ORIENTED_EDGE('',*,*,#9304,.F.);
#13140=ORIENTED_EDGE('',*,*,#9305,.F.);
#13141=ORIENTED_EDGE('',*,*,#9306,.T.);
#13142=ORIENTED_EDGE('',*,*,#9302,.T.);
#13143=ORIENTED_EDGE('',*,*,#9307,.F.);
#13144=ORIENTED_EDGE('',*,*,#9308,.F.);
#13145=ORIENTED_EDGE('',*,*,#9309,.T.);
#13146=ORIENTED_EDGE('',*,*,#9305,.T.);
#13147=ORIENTED_EDGE('',*,*,#9310,.F.);
#13148=ORIENTED_EDGE('',*,*,#9311,.F.);
#13149=ORIENTED_EDGE('',*,*,#9312,.T.);
#13150=ORIENTED_EDGE('',*,*,#9308,.T.);
#13151=ORIENTED_EDGE('',*,*,#9313,.F.);
#13152=ORIENTED_EDGE('',*,*,#9314,.F.);
#13153=ORIENTED_EDGE('',*,*,#9315,.T.);
#13154=ORIENTED_EDGE('',*,*,#9311,.T.);
#13155=ORIENTED_EDGE('',*,*,#9316,.F.);
#13156=ORIENTED_EDGE('',*,*,#9317,.F.);
#13157=ORIENTED_EDGE('',*,*,#9318,.T.);
#13158=ORIENTED_EDGE('',*,*,#9314,.T.);
#13159=ORIENTED_EDGE('',*,*,#9319,.F.);
#13160=ORIENTED_EDGE('',*,*,#9320,.F.);
#13161=ORIENTED_EDGE('',*,*,#9321,.T.);
#13162=ORIENTED_EDGE('',*,*,#9317,.T.);
#13163=ORIENTED_EDGE('',*,*,#9322,.F.);
#13164=ORIENTED_EDGE('',*,*,#9323,.F.);
#13165=ORIENTED_EDGE('',*,*,#9324,.T.);
#13166=ORIENTED_EDGE('',*,*,#9320,.T.);
#13167=ORIENTED_EDGE('',*,*,#9325,.F.);
#13168=ORIENTED_EDGE('',*,*,#9326,.F.);
#13169=ORIENTED_EDGE('',*,*,#9327,.T.);
#13170=ORIENTED_EDGE('',*,*,#9323,.T.);
#13171=ORIENTED_EDGE('',*,*,#9328,.F.);
#13172=ORIENTED_EDGE('',*,*,#9329,.F.);
#13173=ORIENTED_EDGE('',*,*,#9330,.T.);
#13174=ORIENTED_EDGE('',*,*,#9326,.T.);
#13175=ORIENTED_EDGE('',*,*,#9331,.F.);
#13176=ORIENTED_EDGE('',*,*,#9332,.F.);
#13177=ORIENTED_EDGE('',*,*,#9333,.T.);
#13178=ORIENTED_EDGE('',*,*,#9329,.T.);
#13179=ORIENTED_EDGE('',*,*,#9334,.F.);
#13180=ORIENTED_EDGE('',*,*,#9335,.F.);
#13181=ORIENTED_EDGE('',*,*,#9336,.T.);
#13182=ORIENTED_EDGE('',*,*,#9332,.T.);
#13183=ORIENTED_EDGE('',*,*,#9337,.F.);
#13184=ORIENTED_EDGE('',*,*,#9338,.F.);
#13185=ORIENTED_EDGE('',*,*,#9339,.T.);
#13186=ORIENTED_EDGE('',*,*,#9335,.T.);
#13187=ORIENTED_EDGE('',*,*,#9340,.F.);
#13188=ORIENTED_EDGE('',*,*,#9341,.F.);
#13189=ORIENTED_EDGE('',*,*,#9342,.T.);
#13190=ORIENTED_EDGE('',*,*,#9338,.T.);
#13191=ORIENTED_EDGE('',*,*,#9343,.F.);
#13192=ORIENTED_EDGE('',*,*,#9344,.F.);
#13193=ORIENTED_EDGE('',*,*,#9345,.T.);
#13194=ORIENTED_EDGE('',*,*,#9341,.T.);
#13195=ORIENTED_EDGE('',*,*,#9346,.F.);
#13196=ORIENTED_EDGE('',*,*,#9347,.F.);
#13197=ORIENTED_EDGE('',*,*,#9348,.T.);
#13198=ORIENTED_EDGE('',*,*,#9344,.T.);
#13199=ORIENTED_EDGE('',*,*,#9349,.F.);
#13200=ORIENTED_EDGE('',*,*,#9350,.F.);
#13201=ORIENTED_EDGE('',*,*,#9351,.T.);
#13202=ORIENTED_EDGE('',*,*,#9347,.T.);
#13203=ORIENTED_EDGE('',*,*,#9352,.F.);
#13204=ORIENTED_EDGE('',*,*,#9353,.F.);
#13205=ORIENTED_EDGE('',*,*,#9354,.T.);
#13206=ORIENTED_EDGE('',*,*,#9350,.T.);
#13207=ORIENTED_EDGE('',*,*,#9355,.F.);
#13208=ORIENTED_EDGE('',*,*,#9356,.F.);
#13209=ORIENTED_EDGE('',*,*,#8875,.F.);
#13210=ORIENTED_EDGE('',*,*,#9357,.F.);
#13211=ORIENTED_EDGE('',*,*,#9358,.F.);
#13212=ORIENTED_EDGE('',*,*,#9358,.T.);
#13213=ORIENTED_EDGE('',*,*,#9359,.T.);
#13214=ORIENTED_EDGE('',*,*,#9360,.T.);
#13215=ORIENTED_EDGE('',*,*,#9361,.T.);
#13216=ORIENTED_EDGE('',*,*,#9362,.T.);
#13217=ORIENTED_EDGE('',*,*,#9363,.T.);
#13218=ORIENTED_EDGE('',*,*,#9364,.F.);
#13219=ORIENTED_EDGE('',*,*,#9363,.F.);
#13220=ORIENTED_EDGE('',*,*,#9108,.F.);
#13221=ORIENTED_EDGE('',*,*,#9362,.F.);
#13222=ORIENTED_EDGE('',*,*,#9365,.F.);
#13223=ORIENTED_EDGE('',*,*,#9364,.T.);
#13224=ORIENTED_EDGE('',*,*,#9366,.T.);
#13225=ORIENTED_EDGE('',*,*,#9367,.T.);
#13226=ORIENTED_EDGE('',*,*,#9365,.T.);
#13227=ORIENTED_EDGE('',*,*,#9367,.F.);
#13228=ORIENTED_EDGE('',*,*,#9117,.T.);
#13229=ORIENTED_EDGE('',*,*,#9368,.T.);
#13230=ORIENTED_EDGE('',*,*,#9110,.F.);
#13231=ORIENTED_EDGE('',*,*,#9114,.F.);
#13232=ORIENTED_EDGE('',*,*,#9369,.T.);
#13233=ORIENTED_EDGE('',*,*,#9356,.T.);
#13234=ORIENTED_EDGE('',*,*,#9361,.F.);
#13235=ORIENTED_EDGE('',*,*,#9370,.T.);
#13236=ORIENTED_EDGE('',*,*,#9355,.T.);
#13237=ORIENTED_EDGE('',*,*,#9352,.T.);
#13238=ORIENTED_EDGE('',*,*,#9349,.T.);
#13239=ORIENTED_EDGE('',*,*,#9346,.T.);
#13240=ORIENTED_EDGE('',*,*,#9343,.T.);
#13241=ORIENTED_EDGE('',*,*,#9340,.T.);
#13242=ORIENTED_EDGE('',*,*,#9337,.T.);
#13243=ORIENTED_EDGE('',*,*,#9334,.T.);
#13244=ORIENTED_EDGE('',*,*,#9331,.T.);
#13245=ORIENTED_EDGE('',*,*,#9328,.T.);
#13246=ORIENTED_EDGE('',*,*,#9325,.T.);
#13247=ORIENTED_EDGE('',*,*,#9322,.T.);
#13248=ORIENTED_EDGE('',*,*,#9319,.T.);
#13249=ORIENTED_EDGE('',*,*,#9316,.T.);
#13250=ORIENTED_EDGE('',*,*,#9313,.T.);
#13251=ORIENTED_EDGE('',*,*,#9310,.T.);
#13252=ORIENTED_EDGE('',*,*,#9307,.T.);
#13253=ORIENTED_EDGE('',*,*,#9304,.T.);
#13254=ORIENTED_EDGE('',*,*,#9301,.T.);
#13255=ORIENTED_EDGE('',*,*,#9298,.T.);
#13256=ORIENTED_EDGE('',*,*,#9295,.T.);
#13257=ORIENTED_EDGE('',*,*,#9292,.T.);
#13258=ORIENTED_EDGE('',*,*,#9289,.T.);
#13259=ORIENTED_EDGE('',*,*,#9286,.T.);
#13260=ORIENTED_EDGE('',*,*,#9283,.T.);
#13261=ORIENTED_EDGE('',*,*,#9280,.T.);
#13262=ORIENTED_EDGE('',*,*,#9277,.T.);
#13263=ORIENTED_EDGE('',*,*,#9274,.T.);
#13264=ORIENTED_EDGE('',*,*,#9271,.T.);
#13265=ORIENTED_EDGE('',*,*,#9268,.T.);
#13266=ORIENTED_EDGE('',*,*,#9265,.T.);
#13267=ORIENTED_EDGE('',*,*,#9262,.T.);
#13268=ORIENTED_EDGE('',*,*,#9259,.T.);
#13269=ORIENTED_EDGE('',*,*,#9256,.T.);
#13270=ORIENTED_EDGE('',*,*,#9253,.T.);
#13271=ORIENTED_EDGE('',*,*,#9250,.T.);
#13272=ORIENTED_EDGE('',*,*,#9247,.T.);
#13273=ORIENTED_EDGE('',*,*,#9244,.T.);
#13274=ORIENTED_EDGE('',*,*,#9241,.T.);
#13275=ORIENTED_EDGE('',*,*,#9238,.T.);
#13276=ORIENTED_EDGE('',*,*,#9235,.T.);
#13277=ORIENTED_EDGE('',*,*,#9232,.T.);
#13278=ORIENTED_EDGE('',*,*,#9229,.T.);
#13279=ORIENTED_EDGE('',*,*,#9226,.T.);
#13280=ORIENTED_EDGE('',*,*,#9223,.T.);
#13281=ORIENTED_EDGE('',*,*,#9220,.T.);
#13282=ORIENTED_EDGE('',*,*,#9217,.T.);
#13283=ORIENTED_EDGE('',*,*,#9214,.T.);
#13284=ORIENTED_EDGE('',*,*,#9211,.T.);
#13285=ORIENTED_EDGE('',*,*,#9208,.T.);
#13286=ORIENTED_EDGE('',*,*,#9205,.T.);
#13287=ORIENTED_EDGE('',*,*,#9202,.T.);
#13288=ORIENTED_EDGE('',*,*,#9199,.T.);
#13289=ORIENTED_EDGE('',*,*,#9196,.T.);
#13290=ORIENTED_EDGE('',*,*,#9193,.T.);
#13291=ORIENTED_EDGE('',*,*,#9190,.T.);
#13292=ORIENTED_EDGE('',*,*,#9187,.T.);
#13293=ORIENTED_EDGE('',*,*,#9184,.T.);
#13294=ORIENTED_EDGE('',*,*,#9181,.T.);
#13295=ORIENTED_EDGE('',*,*,#9178,.T.);
#13296=ORIENTED_EDGE('',*,*,#9175,.T.);
#13297=ORIENTED_EDGE('',*,*,#9172,.T.);
#13298=ORIENTED_EDGE('',*,*,#9169,.T.);
#13299=ORIENTED_EDGE('',*,*,#9166,.T.);
#13300=ORIENTED_EDGE('',*,*,#9163,.T.);
#13301=ORIENTED_EDGE('',*,*,#9160,.T.);
#13302=ORIENTED_EDGE('',*,*,#9157,.T.);
#13303=ORIENTED_EDGE('',*,*,#9154,.T.);
#13304=ORIENTED_EDGE('',*,*,#9151,.T.);
#13305=ORIENTED_EDGE('',*,*,#9148,.T.);
#13306=ORIENTED_EDGE('',*,*,#9145,.T.);
#13307=ORIENTED_EDGE('',*,*,#9142,.T.);
#13308=ORIENTED_EDGE('',*,*,#9139,.T.);
#13309=ORIENTED_EDGE('',*,*,#9136,.T.);
#13310=ORIENTED_EDGE('',*,*,#9133,.T.);
#13311=ORIENTED_EDGE('',*,*,#9130,.T.);
#13312=ORIENTED_EDGE('',*,*,#9127,.T.);
#13313=ORIENTED_EDGE('',*,*,#9124,.T.);
#13314=ORIENTED_EDGE('',*,*,#9121,.T.);
#13315=ORIENTED_EDGE('',*,*,#9118,.T.);
#13316=ORIENTED_EDGE('',*,*,#9369,.F.);
#13317=ORIENTED_EDGE('',*,*,#9113,.F.);
#13318=ORIENTED_EDGE('',*,*,#9371,.F.);
#13319=ORIENTED_EDGE('',*,*,#9107,.F.);
#13320=ORIENTED_EDGE('',*,*,#9104,.F.);
#13321=ORIENTED_EDGE('',*,*,#9101,.F.);
#13322=ORIENTED_EDGE('',*,*,#9098,.F.);
#13323=ORIENTED_EDGE('',*,*,#9095,.F.);
#13324=ORIENTED_EDGE('',*,*,#9092,.F.);
#13325=ORIENTED_EDGE('',*,*,#9089,.F.);
#13326=ORIENTED_EDGE('',*,*,#9086,.F.);
#13327=ORIENTED_EDGE('',*,*,#9083,.F.);
#13328=ORIENTED_EDGE('',*,*,#9080,.F.);
#13329=ORIENTED_EDGE('',*,*,#9077,.F.);
#13330=ORIENTED_EDGE('',*,*,#9074,.F.);
#13331=ORIENTED_EDGE('',*,*,#9071,.F.);
#13332=ORIENTED_EDGE('',*,*,#9068,.F.);
#13333=ORIENTED_EDGE('',*,*,#9065,.F.);
#13334=ORIENTED_EDGE('',*,*,#9062,.F.);
#13335=ORIENTED_EDGE('',*,*,#9059,.F.);
#13336=ORIENTED_EDGE('',*,*,#9056,.F.);
#13337=ORIENTED_EDGE('',*,*,#9053,.F.);
#13338=ORIENTED_EDGE('',*,*,#9050,.F.);
#13339=ORIENTED_EDGE('',*,*,#9047,.F.);
#13340=ORIENTED_EDGE('',*,*,#9044,.F.);
#13341=ORIENTED_EDGE('',*,*,#9041,.F.);
#13342=ORIENTED_EDGE('',*,*,#9038,.F.);
#13343=ORIENTED_EDGE('',*,*,#9035,.F.);
#13344=ORIENTED_EDGE('',*,*,#9032,.F.);
#13345=ORIENTED_EDGE('',*,*,#9029,.F.);
#13346=ORIENTED_EDGE('',*,*,#9026,.F.);
#13347=ORIENTED_EDGE('',*,*,#9023,.F.);
#13348=ORIENTED_EDGE('',*,*,#9020,.F.);
#13349=ORIENTED_EDGE('',*,*,#9017,.F.);
#13350=ORIENTED_EDGE('',*,*,#9014,.F.);
#13351=ORIENTED_EDGE('',*,*,#9011,.F.);
#13352=ORIENTED_EDGE('',*,*,#9008,.F.);
#13353=ORIENTED_EDGE('',*,*,#9005,.F.);
#13354=ORIENTED_EDGE('',*,*,#9002,.F.);
#13355=ORIENTED_EDGE('',*,*,#8999,.F.);
#13356=ORIENTED_EDGE('',*,*,#8996,.F.);
#13357=ORIENTED_EDGE('',*,*,#8993,.F.);
#13358=ORIENTED_EDGE('',*,*,#8990,.F.);
#13359=ORIENTED_EDGE('',*,*,#8987,.F.);
#13360=ORIENTED_EDGE('',*,*,#8984,.F.);
#13361=ORIENTED_EDGE('',*,*,#8981,.F.);
#13362=ORIENTED_EDGE('',*,*,#8978,.F.);
#13363=ORIENTED_EDGE('',*,*,#8975,.F.);
#13364=ORIENTED_EDGE('',*,*,#8972,.F.);
#13365=ORIENTED_EDGE('',*,*,#8969,.F.);
#13366=ORIENTED_EDGE('',*,*,#8966,.F.);
#13367=ORIENTED_EDGE('',*,*,#8963,.F.);
#13368=ORIENTED_EDGE('',*,*,#8960,.F.);
#13369=ORIENTED_EDGE('',*,*,#8957,.F.);
#13370=ORIENTED_EDGE('',*,*,#8954,.F.);
#13371=ORIENTED_EDGE('',*,*,#8951,.F.);
#13372=ORIENTED_EDGE('',*,*,#8948,.F.);
#13373=ORIENTED_EDGE('',*,*,#8945,.F.);
#13374=ORIENTED_EDGE('',*,*,#8942,.F.);
#13375=ORIENTED_EDGE('',*,*,#8939,.F.);
#13376=ORIENTED_EDGE('',*,*,#8936,.F.);
#13377=ORIENTED_EDGE('',*,*,#8933,.F.);
#13378=ORIENTED_EDGE('',*,*,#8930,.F.);
#13379=ORIENTED_EDGE('',*,*,#8927,.F.);
#13380=ORIENTED_EDGE('',*,*,#8924,.F.);
#13381=ORIENTED_EDGE('',*,*,#8921,.F.);
#13382=ORIENTED_EDGE('',*,*,#8918,.F.);
#13383=ORIENTED_EDGE('',*,*,#8915,.F.);
#13384=ORIENTED_EDGE('',*,*,#8912,.F.);
#13385=ORIENTED_EDGE('',*,*,#8909,.F.);
#13386=ORIENTED_EDGE('',*,*,#8906,.F.);
#13387=ORIENTED_EDGE('',*,*,#8903,.F.);
#13388=ORIENTED_EDGE('',*,*,#8900,.F.);
#13389=ORIENTED_EDGE('',*,*,#8897,.F.);
#13390=ORIENTED_EDGE('',*,*,#8894,.F.);
#13391=ORIENTED_EDGE('',*,*,#8891,.F.);
#13392=ORIENTED_EDGE('',*,*,#8888,.F.);
#13393=ORIENTED_EDGE('',*,*,#8885,.F.);
#13394=ORIENTED_EDGE('',*,*,#8882,.F.);
#13395=ORIENTED_EDGE('',*,*,#8879,.F.);
#13396=ORIENTED_EDGE('',*,*,#8876,.F.);
#13397=ORIENTED_EDGE('',*,*,#9353,.T.);
#13398=ORIENTED_EDGE('',*,*,#9370,.F.);
#13399=ORIENTED_EDGE('',*,*,#9360,.F.);
#13400=ORIENTED_EDGE('',*,*,#9372,.T.);
#13401=ORIENTED_EDGE('',*,*,#9357,.T.);
#13402=ORIENTED_EDGE('',*,*,#8874,.F.);
#13403=ORIENTED_EDGE('',*,*,#8878,.F.);
#13404=ORIENTED_EDGE('',*,*,#8881,.F.);
#13405=ORIENTED_EDGE('',*,*,#8884,.F.);
#13406=ORIENTED_EDGE('',*,*,#8887,.F.);
#13407=ORIENTED_EDGE('',*,*,#8890,.F.);
#13408=ORIENTED_EDGE('',*,*,#8893,.F.);
#13409=ORIENTED_EDGE('',*,*,#8896,.F.);
#13410=ORIENTED_EDGE('',*,*,#8899,.F.);
#13411=ORIENTED_EDGE('',*,*,#8902,.F.);
#13412=ORIENTED_EDGE('',*,*,#8905,.F.);
#13413=ORIENTED_EDGE('',*,*,#8908,.F.);
#13414=ORIENTED_EDGE('',*,*,#8911,.F.);
#13415=ORIENTED_EDGE('',*,*,#8914,.F.);
#13416=ORIENTED_EDGE('',*,*,#8917,.F.);
#13417=ORIENTED_EDGE('',*,*,#8920,.F.);
#13418=ORIENTED_EDGE('',*,*,#8923,.F.);
#13419=ORIENTED_EDGE('',*,*,#8926,.F.);
#13420=ORIENTED_EDGE('',*,*,#8929,.F.);
#13421=ORIENTED_EDGE('',*,*,#8932,.F.);
#13422=ORIENTED_EDGE('',*,*,#8935,.F.);
#13423=ORIENTED_EDGE('',*,*,#8938,.F.);
#13424=ORIENTED_EDGE('',*,*,#8941,.F.);
#13425=ORIENTED_EDGE('',*,*,#8944,.F.);
#13426=ORIENTED_EDGE('',*,*,#8947,.F.);
#13427=ORIENTED_EDGE('',*,*,#8950,.F.);
#13428=ORIENTED_EDGE('',*,*,#8953,.F.);
#13429=ORIENTED_EDGE('',*,*,#8956,.F.);
#13430=ORIENTED_EDGE('',*,*,#8959,.F.);
#13431=ORIENTED_EDGE('',*,*,#8962,.F.);
#13432=ORIENTED_EDGE('',*,*,#8965,.F.);
#13433=ORIENTED_EDGE('',*,*,#8968,.F.);
#13434=ORIENTED_EDGE('',*,*,#8971,.F.);
#13435=ORIENTED_EDGE('',*,*,#8974,.F.);
#13436=ORIENTED_EDGE('',*,*,#8977,.F.);
#13437=ORIENTED_EDGE('',*,*,#8980,.F.);
#13438=ORIENTED_EDGE('',*,*,#8983,.F.);
#13439=ORIENTED_EDGE('',*,*,#8986,.F.);
#13440=ORIENTED_EDGE('',*,*,#8989,.F.);
#13441=ORIENTED_EDGE('',*,*,#8992,.F.);
#13442=ORIENTED_EDGE('',*,*,#8995,.F.);
#13443=ORIENTED_EDGE('',*,*,#8998,.F.);
#13444=ORIENTED_EDGE('',*,*,#9001,.F.);
#13445=ORIENTED_EDGE('',*,*,#9004,.F.);
#13446=ORIENTED_EDGE('',*,*,#9007,.F.);
#13447=ORIENTED_EDGE('',*,*,#9010,.F.);
#13448=ORIENTED_EDGE('',*,*,#9013,.F.);
#13449=ORIENTED_EDGE('',*,*,#9016,.F.);
#13450=ORIENTED_EDGE('',*,*,#9019,.F.);
#13451=ORIENTED_EDGE('',*,*,#9022,.F.);
#13452=ORIENTED_EDGE('',*,*,#9025,.F.);
#13453=ORIENTED_EDGE('',*,*,#9028,.F.);
#13454=ORIENTED_EDGE('',*,*,#9031,.F.);
#13455=ORIENTED_EDGE('',*,*,#9034,.F.);
#13456=ORIENTED_EDGE('',*,*,#9037,.F.);
#13457=ORIENTED_EDGE('',*,*,#9040,.F.);
#13458=ORIENTED_EDGE('',*,*,#9043,.F.);
#13459=ORIENTED_EDGE('',*,*,#9046,.F.);
#13460=ORIENTED_EDGE('',*,*,#9049,.F.);
#13461=ORIENTED_EDGE('',*,*,#9052,.F.);
#13462=ORIENTED_EDGE('',*,*,#9055,.F.);
#13463=ORIENTED_EDGE('',*,*,#9058,.F.);
#13464=ORIENTED_EDGE('',*,*,#9061,.F.);
#13465=ORIENTED_EDGE('',*,*,#9064,.F.);
#13466=ORIENTED_EDGE('',*,*,#9067,.F.);
#13467=ORIENTED_EDGE('',*,*,#9070,.F.);
#13468=ORIENTED_EDGE('',*,*,#9073,.F.);
#13469=ORIENTED_EDGE('',*,*,#9076,.F.);
#13470=ORIENTED_EDGE('',*,*,#9079,.F.);
#13471=ORIENTED_EDGE('',*,*,#9082,.F.);
#13472=ORIENTED_EDGE('',*,*,#9085,.F.);
#13473=ORIENTED_EDGE('',*,*,#9088,.F.);
#13474=ORIENTED_EDGE('',*,*,#9091,.F.);
#13475=ORIENTED_EDGE('',*,*,#9094,.F.);
#13476=ORIENTED_EDGE('',*,*,#9097,.F.);
#13477=ORIENTED_EDGE('',*,*,#9100,.F.);
#13478=ORIENTED_EDGE('',*,*,#9103,.F.);
#13479=ORIENTED_EDGE('',*,*,#9106,.F.);
#13480=ORIENTED_EDGE('',*,*,#9373,.F.);
#13481=ORIENTED_EDGE('',*,*,#9111,.F.);
#13482=ORIENTED_EDGE('',*,*,#9368,.F.);
#13483=ORIENTED_EDGE('',*,*,#9116,.F.);
#13484=ORIENTED_EDGE('',*,*,#9120,.F.);
#13485=ORIENTED_EDGE('',*,*,#9123,.F.);
#13486=ORIENTED_EDGE('',*,*,#9126,.F.);
#13487=ORIENTED_EDGE('',*,*,#9129,.F.);
#13488=ORIENTED_EDGE('',*,*,#9132,.F.);
#13489=ORIENTED_EDGE('',*,*,#9135,.F.);
#13490=ORIENTED_EDGE('',*,*,#9138,.F.);
#13491=ORIENTED_EDGE('',*,*,#9141,.F.);
#13492=ORIENTED_EDGE('',*,*,#9144,.F.);
#13493=ORIENTED_EDGE('',*,*,#9147,.F.);
#13494=ORIENTED_EDGE('',*,*,#9150,.F.);
#13495=ORIENTED_EDGE('',*,*,#9153,.F.);
#13496=ORIENTED_EDGE('',*,*,#9156,.F.);
#13497=ORIENTED_EDGE('',*,*,#9159,.F.);
#13498=ORIENTED_EDGE('',*,*,#9162,.F.);
#13499=ORIENTED_EDGE('',*,*,#9165,.F.);
#13500=ORIENTED_EDGE('',*,*,#9168,.F.);
#13501=ORIENTED_EDGE('',*,*,#9171,.F.);
#13502=ORIENTED_EDGE('',*,*,#9174,.F.);
#13503=ORIENTED_EDGE('',*,*,#9177,.F.);
#13504=ORIENTED_EDGE('',*,*,#9180,.F.);
#13505=ORIENTED_EDGE('',*,*,#9183,.F.);
#13506=ORIENTED_EDGE('',*,*,#9186,.F.);
#13507=ORIENTED_EDGE('',*,*,#9189,.F.);
#13508=ORIENTED_EDGE('',*,*,#9192,.F.);
#13509=ORIENTED_EDGE('',*,*,#9195,.F.);
#13510=ORIENTED_EDGE('',*,*,#9198,.F.);
#13511=ORIENTED_EDGE('',*,*,#9201,.F.);
#13512=ORIENTED_EDGE('',*,*,#9204,.F.);
#13513=ORIENTED_EDGE('',*,*,#9207,.F.);
#13514=ORIENTED_EDGE('',*,*,#9210,.F.);
#13515=ORIENTED_EDGE('',*,*,#9213,.F.);
#13516=ORIENTED_EDGE('',*,*,#9216,.F.);
#13517=ORIENTED_EDGE('',*,*,#9219,.F.);
#13518=ORIENTED_EDGE('',*,*,#9222,.F.);
#13519=ORIENTED_EDGE('',*,*,#9225,.F.);
#13520=ORIENTED_EDGE('',*,*,#9228,.F.);
#13521=ORIENTED_EDGE('',*,*,#9231,.F.);
#13522=ORIENTED_EDGE('',*,*,#9234,.F.);
#13523=ORIENTED_EDGE('',*,*,#9237,.F.);
#13524=ORIENTED_EDGE('',*,*,#9240,.F.);
#13525=ORIENTED_EDGE('',*,*,#9243,.F.);
#13526=ORIENTED_EDGE('',*,*,#9246,.F.);
#13527=ORIENTED_EDGE('',*,*,#9249,.F.);
#13528=ORIENTED_EDGE('',*,*,#9252,.F.);
#13529=ORIENTED_EDGE('',*,*,#9255,.F.);
#13530=ORIENTED_EDGE('',*,*,#9258,.F.);
#13531=ORIENTED_EDGE('',*,*,#9261,.F.);
#13532=ORIENTED_EDGE('',*,*,#9264,.F.);
#13533=ORIENTED_EDGE('',*,*,#9267,.F.);
#13534=ORIENTED_EDGE('',*,*,#9270,.F.);
#13535=ORIENTED_EDGE('',*,*,#9273,.F.);
#13536=ORIENTED_EDGE('',*,*,#9276,.F.);
#13537=ORIENTED_EDGE('',*,*,#9279,.F.);
#13538=ORIENTED_EDGE('',*,*,#9282,.F.);
#13539=ORIENTED_EDGE('',*,*,#9285,.F.);
#13540=ORIENTED_EDGE('',*,*,#9288,.F.);
#13541=ORIENTED_EDGE('',*,*,#9291,.F.);
#13542=ORIENTED_EDGE('',*,*,#9294,.F.);
#13543=ORIENTED_EDGE('',*,*,#9297,.F.);
#13544=ORIENTED_EDGE('',*,*,#9300,.F.);
#13545=ORIENTED_EDGE('',*,*,#9303,.F.);
#13546=ORIENTED_EDGE('',*,*,#9306,.F.);
#13547=ORIENTED_EDGE('',*,*,#9309,.F.);
#13548=ORIENTED_EDGE('',*,*,#9312,.F.);
#13549=ORIENTED_EDGE('',*,*,#9315,.F.);
#13550=ORIENTED_EDGE('',*,*,#9318,.F.);
#13551=ORIENTED_EDGE('',*,*,#9321,.F.);
#13552=ORIENTED_EDGE('',*,*,#9324,.F.);
#13553=ORIENTED_EDGE('',*,*,#9327,.F.);
#13554=ORIENTED_EDGE('',*,*,#9330,.F.);
#13555=ORIENTED_EDGE('',*,*,#9333,.F.);
#13556=ORIENTED_EDGE('',*,*,#9336,.F.);
#13557=ORIENTED_EDGE('',*,*,#9339,.F.);
#13558=ORIENTED_EDGE('',*,*,#9342,.F.);
#13559=ORIENTED_EDGE('',*,*,#9345,.F.);
#13560=ORIENTED_EDGE('',*,*,#9348,.F.);
#13561=ORIENTED_EDGE('',*,*,#9351,.F.);
#13562=ORIENTED_EDGE('',*,*,#9354,.F.);
#13563=ORIENTED_EDGE('',*,*,#9372,.F.);
#13564=ORIENTED_EDGE('',*,*,#9359,.F.);
#13565=ORIENTED_EDGE('',*,*,#9112,.F.);
#13566=ORIENTED_EDGE('',*,*,#9373,.T.);
#13567=ORIENTED_EDGE('',*,*,#9105,.T.);
#13568=ORIENTED_EDGE('',*,*,#9371,.T.);
#13569=ORIENTED_EDGE('',*,*,#9374,.F.);
#13570=ORIENTED_EDGE('',*,*,#9375,.T.);
#13571=ORIENTED_EDGE('',*,*,#9376,.F.);
#13572=ORIENTED_EDGE('',*,*,#9375,.F.);
#13573=ORIENTED_EDGE('',*,*,#9377,.F.);
#13574=ORIENTED_EDGE('',*,*,#9378,.T.);
#13575=ORIENTED_EDGE('',*,*,#9379,.F.);
#13576=ORIENTED_EDGE('',*,*,#9378,.F.);
#13577=ORIENTED_EDGE('',*,*,#9380,.F.);
#13578=ORIENTED_EDGE('',*,*,#9381,.T.);
#13579=ORIENTED_EDGE('',*,*,#9382,.F.);
#13580=ORIENTED_EDGE('',*,*,#9381,.F.);
#13581=ORIENTED_EDGE('',*,*,#9383,.F.);
#13582=ORIENTED_EDGE('',*,*,#9384,.T.);
#13583=ORIENTED_EDGE('',*,*,#9385,.F.);
#13584=ORIENTED_EDGE('',*,*,#9384,.F.);
#13585=ORIENTED_EDGE('',*,*,#9386,.F.);
#13586=ORIENTED_EDGE('',*,*,#9387,.T.);
#13587=ORIENTED_EDGE('',*,*,#9388,.F.);
#13588=ORIENTED_EDGE('',*,*,#9387,.F.);
#13589=ORIENTED_EDGE('',*,*,#9389,.F.);
#13590=ORIENTED_EDGE('',*,*,#9390,.T.);
#13591=ORIENTED_EDGE('',*,*,#9391,.F.);
#13592=ORIENTED_EDGE('',*,*,#9390,.F.);
#13593=ORIENTED_EDGE('',*,*,#9392,.F.);
#13594=ORIENTED_EDGE('',*,*,#9393,.T.);
#13595=ORIENTED_EDGE('',*,*,#9391,.T.);
#13596=ORIENTED_EDGE('',*,*,#9388,.T.);
#13597=ORIENTED_EDGE('',*,*,#9385,.T.);
#13598=ORIENTED_EDGE('',*,*,#9382,.T.);
#13599=ORIENTED_EDGE('',*,*,#9379,.T.);
#13600=ORIENTED_EDGE('',*,*,#9376,.T.);
#13601=ORIENTED_EDGE('',*,*,#9394,.F.);
#13602=ORIENTED_EDGE('',*,*,#9395,.T.);
#13603=ORIENTED_EDGE('',*,*,#9392,.T.);
#13604=ORIENTED_EDGE('',*,*,#9395,.F.);
#13605=ORIENTED_EDGE('',*,*,#9394,.T.);
#13606=ORIENTED_EDGE('',*,*,#9389,.T.);
#13607=ORIENTED_EDGE('',*,*,#9386,.T.);
#13608=ORIENTED_EDGE('',*,*,#9383,.T.);
#13609=ORIENTED_EDGE('',*,*,#9380,.T.);
#13610=ORIENTED_EDGE('',*,*,#9377,.T.);
#13611=ORIENTED_EDGE('',*,*,#9374,.T.);
#13612=ORIENTED_EDGE('',*,*,#9396,.F.);
#13613=ORIENTED_EDGE('',*,*,#9366,.F.);
#13614=ORIENTED_EDGE('',*,*,#9393,.F.);
#13615=ORIENTED_EDGE('',*,*,#9397,.T.);
#13616=ORIENTED_EDGE('',*,*,#9396,.T.);
#13617=ORIENTED_EDGE('',*,*,#9397,.F.);
#13618=ORIENTED_EDGE('',*,*,#9398,.F.);
#13619=ORIENTED_EDGE('',*,*,#9399,.T.);
#13620=ORIENTED_EDGE('',*,*,#9400,.T.);
#13621=ORIENTED_EDGE('',*,*,#9399,.F.);
#13622=ORIENTED_EDGE('',*,*,#9401,.F.);
#13623=ORIENTED_EDGE('',*,*,#9402,.T.);
#13624=ORIENTED_EDGE('',*,*,#9403,.T.);
#13625=ORIENTED_EDGE('',*,*,#9402,.F.);
#13626=ORIENTED_EDGE('',*,*,#9401,.T.);
#13627=ORIENTED_EDGE('',*,*,#9398,.T.);
#13628=ORIENTED_EDGE('',*,*,#9403,.F.);
#13629=ORIENTED_EDGE('',*,*,#9400,.F.);
#13630=ORIENTED_EDGE('',*,*,#9404,.F.);
#13631=ORIENTED_EDGE('',*,*,#9405,.F.);
#13632=ORIENTED_EDGE('',*,*,#9406,.F.);
#13633=ORIENTED_EDGE('',*,*,#9407,.F.);
#13634=ORIENTED_EDGE('',*,*,#9408,.F.);
#13635=ORIENTED_EDGE('',*,*,#9409,.F.);
#13636=ORIENTED_EDGE('',*,*,#9410,.F.);
#13637=ORIENTED_EDGE('',*,*,#9411,.F.);
#13638=ORIENTED_EDGE('',*,*,#9411,.T.);
#13639=ORIENTED_EDGE('',*,*,#9412,.F.);
#13640=ORIENTED_EDGE('',*,*,#9405,.T.);
#13641=ORIENTED_EDGE('',*,*,#9413,.F.);
#13642=ORIENTED_EDGE('',*,*,#9408,.T.);
#13643=ORIENTED_EDGE('',*,*,#9413,.T.);
#13644=ORIENTED_EDGE('',*,*,#9404,.T.);
#13645=ORIENTED_EDGE('',*,*,#9414,.F.);
#13646=ORIENTED_EDGE('',*,*,#9410,.T.);
#13647=ORIENTED_EDGE('',*,*,#9415,.F.);
#13648=ORIENTED_EDGE('',*,*,#9406,.T.);
#13649=ORIENTED_EDGE('',*,*,#9412,.T.);
#13650=ORIENTED_EDGE('',*,*,#9409,.T.);
#13651=ORIENTED_EDGE('',*,*,#9414,.T.);
#13652=ORIENTED_EDGE('',*,*,#9407,.T.);
#13653=ORIENTED_EDGE('',*,*,#9415,.T.);
#13654=ORIENTED_EDGE('',*,*,#9416,.F.);
#13655=ORIENTED_EDGE('',*,*,#9417,.T.);
#13656=ORIENTED_EDGE('',*,*,#9418,.T.);
#13657=ORIENTED_EDGE('',*,*,#9419,.T.);
#13658=ORIENTED_EDGE('',*,*,#9420,.F.);
#13659=ORIENTED_EDGE('',*,*,#9421,.T.);
#13660=ORIENTED_EDGE('',*,*,#9416,.T.);
#13661=ORIENTED_EDGE('',*,*,#9422,.T.);
#13662=ORIENTED_EDGE('',*,*,#9423,.F.);
#13663=ORIENTED_EDGE('',*,*,#9424,.T.);
#13664=ORIENTED_EDGE('',*,*,#9420,.T.);
#13665=ORIENTED_EDGE('',*,*,#9425,.T.);
#13666=ORIENTED_EDGE('',*,*,#9426,.F.);
#13667=ORIENTED_EDGE('',*,*,#9427,.T.);
#13668=ORIENTED_EDGE('',*,*,#9423,.T.);
#13669=ORIENTED_EDGE('',*,*,#9428,.T.);
#13670=ORIENTED_EDGE('',*,*,#9429,.F.);
#13671=ORIENTED_EDGE('',*,*,#9430,.T.);
#13672=ORIENTED_EDGE('',*,*,#9426,.T.);
#13673=ORIENTED_EDGE('',*,*,#9431,.T.);
#13674=ORIENTED_EDGE('',*,*,#9432,.F.);
#13675=ORIENTED_EDGE('',*,*,#9433,.T.);
#13676=ORIENTED_EDGE('',*,*,#9429,.T.);
#13677=ORIENTED_EDGE('',*,*,#9434,.T.);
#13678=ORIENTED_EDGE('',*,*,#9435,.F.);
#13679=ORIENTED_EDGE('',*,*,#9436,.T.);
#13680=ORIENTED_EDGE('',*,*,#9432,.T.);
#13681=ORIENTED_EDGE('',*,*,#9437,.T.);
#13682=ORIENTED_EDGE('',*,*,#9438,.F.);
#13683=ORIENTED_EDGE('',*,*,#9439,.T.);
#13684=ORIENTED_EDGE('',*,*,#9435,.T.);
#13685=ORIENTED_EDGE('',*,*,#9440,.T.);
#13686=ORIENTED_EDGE('',*,*,#9441,.F.);
#13687=ORIENTED_EDGE('',*,*,#9442,.T.);
#13688=ORIENTED_EDGE('',*,*,#9438,.T.);
#13689=ORIENTED_EDGE('',*,*,#9443,.T.);
#13690=ORIENTED_EDGE('',*,*,#9444,.F.);
#13691=ORIENTED_EDGE('',*,*,#9445,.T.);
#13692=ORIENTED_EDGE('',*,*,#9441,.T.);
#13693=ORIENTED_EDGE('',*,*,#9446,.T.);
#13694=ORIENTED_EDGE('',*,*,#9447,.F.);
#13695=ORIENTED_EDGE('',*,*,#9448,.T.);
#13696=ORIENTED_EDGE('',*,*,#9444,.T.);
#13697=ORIENTED_EDGE('',*,*,#9449,.T.);
#13698=ORIENTED_EDGE('',*,*,#9450,.F.);
#13699=ORIENTED_EDGE('',*,*,#9451,.T.);
#13700=ORIENTED_EDGE('',*,*,#9447,.T.);
#13701=ORIENTED_EDGE('',*,*,#9452,.T.);
#13702=ORIENTED_EDGE('',*,*,#9453,.F.);
#13703=ORIENTED_EDGE('',*,*,#9454,.T.);
#13704=ORIENTED_EDGE('',*,*,#9450,.T.);
#13705=ORIENTED_EDGE('',*,*,#9455,.T.);
#13706=ORIENTED_EDGE('',*,*,#9456,.F.);
#13707=ORIENTED_EDGE('',*,*,#9457,.T.);
#13708=ORIENTED_EDGE('',*,*,#9453,.T.);
#13709=ORIENTED_EDGE('',*,*,#9458,.T.);
#13710=ORIENTED_EDGE('',*,*,#9459,.F.);
#13711=ORIENTED_EDGE('',*,*,#9460,.T.);
#13712=ORIENTED_EDGE('',*,*,#9456,.T.);
#13713=ORIENTED_EDGE('',*,*,#9461,.T.);
#13714=ORIENTED_EDGE('',*,*,#9462,.F.);
#13715=ORIENTED_EDGE('',*,*,#9463,.T.);
#13716=ORIENTED_EDGE('',*,*,#9459,.T.);
#13717=ORIENTED_EDGE('',*,*,#9464,.T.);
#13718=ORIENTED_EDGE('',*,*,#9465,.F.);
#13719=ORIENTED_EDGE('',*,*,#9466,.T.);
#13720=ORIENTED_EDGE('',*,*,#9462,.T.);
#13721=ORIENTED_EDGE('',*,*,#9467,.T.);
#13722=ORIENTED_EDGE('',*,*,#9468,.F.);
#13723=ORIENTED_EDGE('',*,*,#9469,.T.);
#13724=ORIENTED_EDGE('',*,*,#9465,.T.);
#13725=ORIENTED_EDGE('',*,*,#9470,.T.);
#13726=ORIENTED_EDGE('',*,*,#9471,.F.);
#13727=ORIENTED_EDGE('',*,*,#9472,.T.);
#13728=ORIENTED_EDGE('',*,*,#9473,.F.);
#13729=ORIENTED_EDGE('',*,*,#9474,.F.);
#13730=ORIENTED_EDGE('',*,*,#9475,.F.);
#13731=ORIENTED_EDGE('',*,*,#9476,.T.);
#13732=ORIENTED_EDGE('',*,*,#9471,.T.);
#13733=ORIENTED_EDGE('',*,*,#9477,.F.);
#13734=ORIENTED_EDGE('',*,*,#9478,.F.);
#13735=ORIENTED_EDGE('',*,*,#9479,.T.);
#13736=ORIENTED_EDGE('',*,*,#9475,.T.);
#13737=ORIENTED_EDGE('',*,*,#9480,.F.);
#13738=ORIENTED_EDGE('',*,*,#9481,.F.);
#13739=ORIENTED_EDGE('',*,*,#9482,.T.);
#13740=ORIENTED_EDGE('',*,*,#9478,.T.);
#13741=ORIENTED_EDGE('',*,*,#9483,.F.);
#13742=ORIENTED_EDGE('',*,*,#9484,.F.);
#13743=ORIENTED_EDGE('',*,*,#9485,.T.);
#13744=ORIENTED_EDGE('',*,*,#9481,.T.);
#13745=ORIENTED_EDGE('',*,*,#9486,.F.);
#13746=ORIENTED_EDGE('',*,*,#9487,.F.);
#13747=ORIENTED_EDGE('',*,*,#9488,.T.);
#13748=ORIENTED_EDGE('',*,*,#9484,.T.);
#13749=ORIENTED_EDGE('',*,*,#9489,.F.);
#13750=ORIENTED_EDGE('',*,*,#9490,.F.);
#13751=ORIENTED_EDGE('',*,*,#9491,.T.);
#13752=ORIENTED_EDGE('',*,*,#9487,.T.);
#13753=ORIENTED_EDGE('',*,*,#9492,.F.);
#13754=ORIENTED_EDGE('',*,*,#9493,.F.);
#13755=ORIENTED_EDGE('',*,*,#9494,.T.);
#13756=ORIENTED_EDGE('',*,*,#9490,.T.);
#13757=ORIENTED_EDGE('',*,*,#9495,.F.);
#13758=ORIENTED_EDGE('',*,*,#9496,.F.);
#13759=ORIENTED_EDGE('',*,*,#9497,.T.);
#13760=ORIENTED_EDGE('',*,*,#9493,.T.);
#13761=ORIENTED_EDGE('',*,*,#9498,.F.);
#13762=ORIENTED_EDGE('',*,*,#9499,.F.);
#13763=ORIENTED_EDGE('',*,*,#9500,.T.);
#13764=ORIENTED_EDGE('',*,*,#9496,.T.);
#13765=ORIENTED_EDGE('',*,*,#9501,.F.);
#13766=ORIENTED_EDGE('',*,*,#9502,.F.);
#13767=ORIENTED_EDGE('',*,*,#9503,.T.);
#13768=ORIENTED_EDGE('',*,*,#9499,.T.);
#13769=ORIENTED_EDGE('',*,*,#9504,.F.);
#13770=ORIENTED_EDGE('',*,*,#9505,.F.);
#13771=ORIENTED_EDGE('',*,*,#9506,.T.);
#13772=ORIENTED_EDGE('',*,*,#9502,.T.);
#13773=ORIENTED_EDGE('',*,*,#9507,.F.);
#13774=ORIENTED_EDGE('',*,*,#9508,.F.);
#13775=ORIENTED_EDGE('',*,*,#9509,.T.);
#13776=ORIENTED_EDGE('',*,*,#9505,.T.);
#13777=ORIENTED_EDGE('',*,*,#9510,.F.);
#13778=ORIENTED_EDGE('',*,*,#9511,.F.);
#13779=ORIENTED_EDGE('',*,*,#9512,.T.);
#13780=ORIENTED_EDGE('',*,*,#9508,.T.);
#13781=ORIENTED_EDGE('',*,*,#9513,.F.);
#13782=ORIENTED_EDGE('',*,*,#9514,.F.);
#13783=ORIENTED_EDGE('',*,*,#9515,.T.);
#13784=ORIENTED_EDGE('',*,*,#9511,.T.);
#13785=ORIENTED_EDGE('',*,*,#9516,.F.);
#13786=ORIENTED_EDGE('',*,*,#9517,.F.);
#13787=ORIENTED_EDGE('',*,*,#9518,.T.);
#13788=ORIENTED_EDGE('',*,*,#9514,.T.);
#13789=ORIENTED_EDGE('',*,*,#9519,.F.);
#13790=ORIENTED_EDGE('',*,*,#9520,.F.);
#13791=ORIENTED_EDGE('',*,*,#9521,.T.);
#13792=ORIENTED_EDGE('',*,*,#9517,.T.);
#13793=ORIENTED_EDGE('',*,*,#9522,.F.);
#13794=ORIENTED_EDGE('',*,*,#9523,.F.);
#13795=ORIENTED_EDGE('',*,*,#9524,.T.);
#13796=ORIENTED_EDGE('',*,*,#9520,.T.);
#13797=ORIENTED_EDGE('',*,*,#9525,.F.);
#13798=ORIENTED_EDGE('',*,*,#9526,.F.);
#13799=ORIENTED_EDGE('',*,*,#9527,.T.);
#13800=ORIENTED_EDGE('',*,*,#9528,.T.);
#13801=ORIENTED_EDGE('',*,*,#9529,.F.);
#13802=ORIENTED_EDGE('',*,*,#9530,.F.);
#13803=ORIENTED_EDGE('',*,*,#9531,.T.);
#13804=ORIENTED_EDGE('',*,*,#9532,.T.);
#13805=ORIENTED_EDGE('',*,*,#9527,.F.);
#13806=ORIENTED_EDGE('',*,*,#9533,.F.);
#13807=ORIENTED_EDGE('',*,*,#9534,.T.);
#13808=ORIENTED_EDGE('',*,*,#9535,.T.);
#13809=ORIENTED_EDGE('',*,*,#9531,.F.);
#13810=ORIENTED_EDGE('',*,*,#9536,.F.);
#13811=ORIENTED_EDGE('',*,*,#9537,.T.);
#13812=ORIENTED_EDGE('',*,*,#9538,.T.);
#13813=ORIENTED_EDGE('',*,*,#9534,.F.);
#13814=ORIENTED_EDGE('',*,*,#9539,.F.);
#13815=ORIENTED_EDGE('',*,*,#9540,.T.);
#13816=ORIENTED_EDGE('',*,*,#9541,.T.);
#13817=ORIENTED_EDGE('',*,*,#9537,.F.);
#13818=ORIENTED_EDGE('',*,*,#9542,.F.);
#13819=ORIENTED_EDGE('',*,*,#9529,.T.);
#13820=ORIENTED_EDGE('',*,*,#9543,.T.);
#13821=ORIENTED_EDGE('',*,*,#9540,.F.);
#13822=ORIENTED_EDGE('',*,*,#9543,.F.);
#13823=ORIENTED_EDGE('',*,*,#9528,.F.);
#13824=ORIENTED_EDGE('',*,*,#9532,.F.);
#13825=ORIENTED_EDGE('',*,*,#9535,.F.);
#13826=ORIENTED_EDGE('',*,*,#9538,.F.);
#13827=ORIENTED_EDGE('',*,*,#9541,.F.);
#13828=ORIENTED_EDGE('',*,*,#9544,.F.);
#13829=ORIENTED_EDGE('',*,*,#9545,.F.);
#13830=ORIENTED_EDGE('',*,*,#9470,.F.);
#13831=ORIENTED_EDGE('',*,*,#9467,.F.);
#13832=ORIENTED_EDGE('',*,*,#9464,.F.);
#13833=ORIENTED_EDGE('',*,*,#9461,.F.);
#13834=ORIENTED_EDGE('',*,*,#9458,.F.);
#13835=ORIENTED_EDGE('',*,*,#9455,.F.);
#13836=ORIENTED_EDGE('',*,*,#9452,.F.);
#13837=ORIENTED_EDGE('',*,*,#9449,.F.);
#13838=ORIENTED_EDGE('',*,*,#9446,.F.);
#13839=ORIENTED_EDGE('',*,*,#9443,.F.);
#13840=ORIENTED_EDGE('',*,*,#9440,.F.);
#13841=ORIENTED_EDGE('',*,*,#9437,.F.);
#13842=ORIENTED_EDGE('',*,*,#9434,.F.);
#13843=ORIENTED_EDGE('',*,*,#9431,.F.);
#13844=ORIENTED_EDGE('',*,*,#9428,.F.);
#13845=ORIENTED_EDGE('',*,*,#9425,.F.);
#13846=ORIENTED_EDGE('',*,*,#9422,.F.);
#13847=ORIENTED_EDGE('',*,*,#9419,.F.);
#13848=ORIENTED_EDGE('',*,*,#9546,.F.);
#13849=ORIENTED_EDGE('',*,*,#9547,.T.);
#13850=ORIENTED_EDGE('',*,*,#9525,.T.);
#13851=ORIENTED_EDGE('',*,*,#9522,.T.);
#13852=ORIENTED_EDGE('',*,*,#9519,.T.);
#13853=ORIENTED_EDGE('',*,*,#9516,.T.);
#13854=ORIENTED_EDGE('',*,*,#9513,.T.);
#13855=ORIENTED_EDGE('',*,*,#9510,.T.);
#13856=ORIENTED_EDGE('',*,*,#9507,.T.);
#13857=ORIENTED_EDGE('',*,*,#9504,.T.);
#13858=ORIENTED_EDGE('',*,*,#9501,.T.);
#13859=ORIENTED_EDGE('',*,*,#9498,.T.);
#13860=ORIENTED_EDGE('',*,*,#9495,.T.);
#13861=ORIENTED_EDGE('',*,*,#9492,.T.);
#13862=ORIENTED_EDGE('',*,*,#9489,.T.);
#13863=ORIENTED_EDGE('',*,*,#9486,.T.);
#13864=ORIENTED_EDGE('',*,*,#9483,.T.);
#13865=ORIENTED_EDGE('',*,*,#9480,.T.);
#13866=ORIENTED_EDGE('',*,*,#9477,.T.);
#13867=ORIENTED_EDGE('',*,*,#9474,.T.);
#13868=ORIENTED_EDGE('',*,*,#9523,.T.);
#13869=ORIENTED_EDGE('',*,*,#9547,.F.);
#13870=ORIENTED_EDGE('',*,*,#9548,.F.);
#13871=ORIENTED_EDGE('',*,*,#9549,.T.);
#13872=ORIENTED_EDGE('',*,*,#9550,.F.);
#13873=ORIENTED_EDGE('',*,*,#9472,.F.);
#13874=ORIENTED_EDGE('',*,*,#9476,.F.);
#13875=ORIENTED_EDGE('',*,*,#9479,.F.);
#13876=ORIENTED_EDGE('',*,*,#9482,.F.);
#13877=ORIENTED_EDGE('',*,*,#9485,.F.);
#13878=ORIENTED_EDGE('',*,*,#9488,.F.);
#13879=ORIENTED_EDGE('',*,*,#9491,.F.);
#13880=ORIENTED_EDGE('',*,*,#9494,.F.);
#13881=ORIENTED_EDGE('',*,*,#9497,.F.);
#13882=ORIENTED_EDGE('',*,*,#9500,.F.);
#13883=ORIENTED_EDGE('',*,*,#9503,.F.);
#13884=ORIENTED_EDGE('',*,*,#9506,.F.);
#13885=ORIENTED_EDGE('',*,*,#9509,.F.);
#13886=ORIENTED_EDGE('',*,*,#9512,.F.);
#13887=ORIENTED_EDGE('',*,*,#9515,.F.);
#13888=ORIENTED_EDGE('',*,*,#9518,.F.);
#13889=ORIENTED_EDGE('',*,*,#9521,.F.);
#13890=ORIENTED_EDGE('',*,*,#9524,.F.);
#13891=ORIENTED_EDGE('',*,*,#9549,.F.);
#13892=ORIENTED_EDGE('',*,*,#9551,.F.);
#13893=ORIENTED_EDGE('',*,*,#9417,.F.);
#13894=ORIENTED_EDGE('',*,*,#9421,.F.);
#13895=ORIENTED_EDGE('',*,*,#9424,.F.);
#13896=ORIENTED_EDGE('',*,*,#9427,.F.);
#13897=ORIENTED_EDGE('',*,*,#9430,.F.);
#13898=ORIENTED_EDGE('',*,*,#9433,.F.);
#13899=ORIENTED_EDGE('',*,*,#9436,.F.);
#13900=ORIENTED_EDGE('',*,*,#9439,.F.);
#13901=ORIENTED_EDGE('',*,*,#9442,.F.);
#13902=ORIENTED_EDGE('',*,*,#9445,.F.);
#13903=ORIENTED_EDGE('',*,*,#9448,.F.);
#13904=ORIENTED_EDGE('',*,*,#9451,.F.);
#13905=ORIENTED_EDGE('',*,*,#9454,.F.);
#13906=ORIENTED_EDGE('',*,*,#9457,.F.);
#13907=ORIENTED_EDGE('',*,*,#9460,.F.);
#13908=ORIENTED_EDGE('',*,*,#9463,.F.);
#13909=ORIENTED_EDGE('',*,*,#9466,.F.);
#13910=ORIENTED_EDGE('',*,*,#9469,.F.);
#13911=ORIENTED_EDGE('',*,*,#9552,.F.);
#13912=ORIENTED_EDGE('',*,*,#9544,.T.);
#13913=ORIENTED_EDGE('',*,*,#9473,.T.);
#13914=ORIENTED_EDGE('',*,*,#9550,.T.);
#13915=ORIENTED_EDGE('',*,*,#9553,.T.);
#13916=ORIENTED_EDGE('',*,*,#9468,.T.);
#13917=ORIENTED_EDGE('',*,*,#9545,.T.);
#13918=ORIENTED_EDGE('',*,*,#9553,.F.);
#13919=ORIENTED_EDGE('',*,*,#9552,.T.);
#13920=ORIENTED_EDGE('',*,*,#9546,.T.);
#13921=ORIENTED_EDGE('',*,*,#9418,.F.);
#13922=ORIENTED_EDGE('',*,*,#9551,.T.);
#13923=ORIENTED_EDGE('',*,*,#9548,.T.);
#13924=ORIENTED_EDGE('',*,*,#9526,.T.);
#13925=ORIENTED_EDGE('',*,*,#9542,.T.);
#13926=ORIENTED_EDGE('',*,*,#9539,.T.);
#13927=ORIENTED_EDGE('',*,*,#9536,.T.);
#13928=ORIENTED_EDGE('',*,*,#9533,.T.);
#13929=ORIENTED_EDGE('',*,*,#9530,.T.);
#13930=ORIENTED_EDGE('',*,*,#9554,.F.);
#13931=ORIENTED_EDGE('',*,*,#9555,.T.);
#13932=ORIENTED_EDGE('',*,*,#9556,.F.);
#13933=ORIENTED_EDGE('',*,*,#9557,.T.);
#13934=ORIENTED_EDGE('',*,*,#9554,.T.);
#13935=ORIENTED_EDGE('',*,*,#9557,.F.);
#13936=ORIENTED_EDGE('',*,*,#9555,.F.);
#13937=ORIENTED_EDGE('',*,*,#9558,.T.);
#13938=ORIENTED_EDGE('',*,*,#9559,.F.);
#13939=ORIENTED_EDGE('',*,*,#9558,.F.);
#13940=ORIENTED_EDGE('',*,*,#9560,.F.);
#13941=ORIENTED_EDGE('',*,*,#9561,.T.);
#13942=ORIENTED_EDGE('',*,*,#9562,.F.);
#13943=ORIENTED_EDGE('',*,*,#9563,.T.);
#13944=ORIENTED_EDGE('',*,*,#9560,.T.);
#13945=ORIENTED_EDGE('',*,*,#9563,.F.);
#13946=ORIENTED_EDGE('',*,*,#9561,.F.);
#13947=ORIENTED_EDGE('',*,*,#9564,.T.);
#13948=ORIENTED_EDGE('',*,*,#9565,.F.);
#13949=ORIENTED_EDGE('',*,*,#9564,.F.);
#13950=ORIENTED_EDGE('',*,*,#9566,.F.);
#13951=ORIENTED_EDGE('',*,*,#9567,.T.);
#13952=ORIENTED_EDGE('',*,*,#9568,.F.);
#13953=ORIENTED_EDGE('',*,*,#9569,.T.);
#13954=ORIENTED_EDGE('',*,*,#9566,.T.);
#13955=ORIENTED_EDGE('',*,*,#9569,.F.);
#13956=ORIENTED_EDGE('',*,*,#9567,.F.);
#13957=ORIENTED_EDGE('',*,*,#9570,.T.);
#13958=ORIENTED_EDGE('',*,*,#9571,.F.);
#13959=ORIENTED_EDGE('',*,*,#9570,.F.);
#13960=ORIENTED_EDGE('',*,*,#9572,.F.);
#13961=ORIENTED_EDGE('',*,*,#9573,.T.);
#13962=ORIENTED_EDGE('',*,*,#9574,.F.);
#13963=ORIENTED_EDGE('',*,*,#9575,.T.);
#13964=ORIENTED_EDGE('',*,*,#9572,.T.);
#13965=ORIENTED_EDGE('',*,*,#9575,.F.);
#13966=ORIENTED_EDGE('',*,*,#9573,.F.);
#13967=ORIENTED_EDGE('',*,*,#9576,.T.);
#13968=ORIENTED_EDGE('',*,*,#9577,.F.);
#13969=ORIENTED_EDGE('',*,*,#9576,.F.);
#13970=ORIENTED_EDGE('',*,*,#9578,.F.);
#13971=ORIENTED_EDGE('',*,*,#9579,.T.);
#13972=ORIENTED_EDGE('',*,*,#9580,.T.);
#13973=ORIENTED_EDGE('',*,*,#9579,.F.);
#13974=ORIENTED_EDGE('',*,*,#9581,.F.);
#13975=ORIENTED_EDGE('',*,*,#9582,.T.);
#13976=ORIENTED_EDGE('',*,*,#9583,.T.);
#13977=ORIENTED_EDGE('',*,*,#9582,.F.);
#13978=ORIENTED_EDGE('',*,*,#9581,.T.);
#13979=ORIENTED_EDGE('',*,*,#9578,.T.);
#13980=ORIENTED_EDGE('',*,*,#9574,.T.);
#13981=ORIENTED_EDGE('',*,*,#9568,.T.);
#13982=ORIENTED_EDGE('',*,*,#9562,.T.);
#13983=ORIENTED_EDGE('',*,*,#9556,.T.);
#13984=ORIENTED_EDGE('',*,*,#9583,.F.);
#13985=ORIENTED_EDGE('',*,*,#9580,.F.);
#13986=ORIENTED_EDGE('',*,*,#9577,.T.);
#13987=ORIENTED_EDGE('',*,*,#9571,.T.);
#13988=ORIENTED_EDGE('',*,*,#9565,.T.);
#13989=ORIENTED_EDGE('',*,*,#9559,.T.);
#13990=ORIENTED_EDGE('',*,*,#9584,.F.);
#13991=ORIENTED_EDGE('',*,*,#9585,.T.);
#13992=ORIENTED_EDGE('',*,*,#9586,.F.);
#13993=ORIENTED_EDGE('',*,*,#9585,.F.);
#13994=ORIENTED_EDGE('',*,*,#9586,.T.);
#13995=ORIENTED_EDGE('',*,*,#9587,.T.);
#13996=ORIENTED_EDGE('',*,*,#9588,.T.);
#13997=ORIENTED_EDGE('',*,*,#9587,.F.);
#13998=ORIENTED_EDGE('',*,*,#9589,.F.);
#13999=ORIENTED_EDGE('',*,*,#9590,.T.);
#14000=ORIENTED_EDGE('',*,*,#9591,.T.);
#14001=ORIENTED_EDGE('',*,*,#9590,.F.);
#14002=ORIENTED_EDGE('',*,*,#9592,.F.);
#14003=ORIENTED_EDGE('',*,*,#9593,.T.);
#14004=ORIENTED_EDGE('',*,*,#9584,.T.);
#14005=ORIENTED_EDGE('',*,*,#9593,.F.);
#14006=ORIENTED_EDGE('',*,*,#9592,.T.);
#14007=ORIENTED_EDGE('',*,*,#9589,.T.);
#14008=ORIENTED_EDGE('',*,*,#9588,.F.);
#14009=ORIENTED_EDGE('',*,*,#9591,.F.);
#14010=ORIENTED_EDGE('',*,*,#9594,.F.);
#14011=ORIENTED_EDGE('',*,*,#9595,.T.);
#14012=ORIENTED_EDGE('',*,*,#9596,.F.);
#14013=ORIENTED_EDGE('',*,*,#9595,.F.);
#14014=ORIENTED_EDGE('',*,*,#9597,.F.);
#14015=ORIENTED_EDGE('',*,*,#9598,.T.);
#14016=ORIENTED_EDGE('',*,*,#9596,.T.);
#14017=ORIENTED_EDGE('',*,*,#9598,.F.);
#14018=ORIENTED_EDGE('',*,*,#9594,.T.);
#14019=ORIENTED_EDGE('',*,*,#9599,.T.);
#14020=ORIENTED_EDGE('',*,*,#9600,.T.);
#14021=ORIENTED_EDGE('',*,*,#9599,.F.);
#14022=ORIENTED_EDGE('',*,*,#9601,.F.);
#14023=ORIENTED_EDGE('',*,*,#9602,.T.);
#14024=ORIENTED_EDGE('',*,*,#9603,.T.);
#14025=ORIENTED_EDGE('',*,*,#9602,.F.);
#14026=ORIENTED_EDGE('',*,*,#9601,.T.);
#14027=ORIENTED_EDGE('',*,*,#9597,.T.);
#14028=ORIENTED_EDGE('',*,*,#9603,.F.);
#14029=ORIENTED_EDGE('',*,*,#9600,.F.);
#14030=ORIENTED_EDGE('',*,*,#9604,.T.);
#14031=ORIENTED_EDGE('',*,*,#9604,.F.);
#14032=ORIENTED_EDGE('',*,*,#9605,.F.);
#14033=ORIENTED_EDGE('',*,*,#9606,.F.);
#14034=ORIENTED_EDGE('',*,*,#9607,.F.);
#14035=ORIENTED_EDGE('',*,*,#9608,.T.);
#14036=ORIENTED_EDGE('',*,*,#9608,.F.);
#14037=ORIENTED_EDGE('',*,*,#9609,.F.);
#14038=ORIENTED_EDGE('',*,*,#9610,.F.);
#14039=ORIENTED_EDGE('',*,*,#9611,.F.);
#14040=ORIENTED_EDGE('',*,*,#9612,.T.);
#14041=ORIENTED_EDGE('',*,*,#9613,.T.);
#14042=ORIENTED_EDGE('',*,*,#9614,.T.);
#14043=ORIENTED_EDGE('',*,*,#9615,.T.);
#14044=ORIENTED_EDGE('',*,*,#9616,.T.);
#14045=ORIENTED_EDGE('',*,*,#9617,.T.);
#14046=ORIENTED_EDGE('',*,*,#9618,.T.);
#14047=ORIENTED_EDGE('',*,*,#9619,.T.);
#14048=ORIENTED_EDGE('',*,*,#9620,.T.);
#14049=ORIENTED_EDGE('',*,*,#9621,.T.);
#14050=ORIENTED_EDGE('',*,*,#9622,.T.);
#14051=ORIENTED_EDGE('',*,*,#9623,.T.);
#14052=ORIENTED_EDGE('',*,*,#9624,.T.);
#14053=ORIENTED_EDGE('',*,*,#9625,.T.);
#14054=ORIENTED_EDGE('',*,*,#9626,.T.);
#14055=ORIENTED_EDGE('',*,*,#9627,.T.);
#14056=ORIENTED_EDGE('',*,*,#9628,.T.);
#14057=ORIENTED_EDGE('',*,*,#9629,.T.);
#14058=ORIENTED_EDGE('',*,*,#9609,.T.);
#14059=ORIENTED_EDGE('',*,*,#9607,.T.);
#14060=ORIENTED_EDGE('',*,*,#9630,.T.);
#14061=ORIENTED_EDGE('',*,*,#9631,.T.);
#14062=ORIENTED_EDGE('',*,*,#9632,.T.);
#14063=ORIENTED_EDGE('',*,*,#9633,.T.);
#14064=ORIENTED_EDGE('',*,*,#9634,.T.);
#14065=ORIENTED_EDGE('',*,*,#9635,.T.);
#14066=ORIENTED_EDGE('',*,*,#9636,.T.);
#14067=ORIENTED_EDGE('',*,*,#9637,.T.);
#14068=ORIENTED_EDGE('',*,*,#9638,.T.);
#14069=ORIENTED_EDGE('',*,*,#9639,.T.);
#14070=ORIENTED_EDGE('',*,*,#9640,.T.);
#14071=ORIENTED_EDGE('',*,*,#9612,.F.);
#14072=ORIENTED_EDGE('',*,*,#9606,.T.);
#14073=ORIENTED_EDGE('',*,*,#9641,.F.);
#14074=ORIENTED_EDGE('',*,*,#9642,.T.);
#14075=ORIENTED_EDGE('',*,*,#9630,.F.);
#14076=ORIENTED_EDGE('',*,*,#9643,.F.);
#14077=ORIENTED_EDGE('',*,*,#9644,.F.);
#14078=ORIENTED_EDGE('',*,*,#9632,.F.);
#14079=ORIENTED_EDGE('',*,*,#9645,.T.);
#14080=ORIENTED_EDGE('',*,*,#9645,.F.);
#14081=ORIENTED_EDGE('',*,*,#9631,.F.);
#14082=ORIENTED_EDGE('',*,*,#9642,.F.);
#14083=ORIENTED_EDGE('',*,*,#9644,.T.);
#14084=ORIENTED_EDGE('',*,*,#9646,.F.);
#14085=ORIENTED_EDGE('',*,*,#9647,.T.);
#14086=ORIENTED_EDGE('',*,*,#9633,.F.);
#14087=ORIENTED_EDGE('',*,*,#9648,.F.);
#14088=ORIENTED_EDGE('',*,*,#9649,.F.);
#14089=ORIENTED_EDGE('',*,*,#9650,.T.);
#14090=ORIENTED_EDGE('',*,*,#9650,.F.);
#14091=ORIENTED_EDGE('',*,*,#9651,.F.);
#14092=ORIENTED_EDGE('',*,*,#9634,.F.);
#14093=ORIENTED_EDGE('',*,*,#9647,.F.);
#14094=ORIENTED_EDGE('',*,*,#9651,.T.);
#14095=ORIENTED_EDGE('',*,*,#9649,.T.);
#14096=ORIENTED_EDGE('',*,*,#9652,.F.);
#14097=ORIENTED_EDGE('',*,*,#9653,.T.);
#14098=ORIENTED_EDGE('',*,*,#9635,.F.);
#14099=ORIENTED_EDGE('',*,*,#9654,.F.);
#14100=ORIENTED_EDGE('',*,*,#9655,.F.);
#14101=ORIENTED_EDGE('',*,*,#9636,.F.);
#14102=ORIENTED_EDGE('',*,*,#9653,.F.);
#14103=ORIENTED_EDGE('',*,*,#9656,.F.);
#14104=ORIENTED_EDGE('',*,*,#9657,.T.);
#14105=ORIENTED_EDGE('',*,*,#9657,.F.);
#14106=ORIENTED_EDGE('',*,*,#9655,.T.);
#14107=ORIENTED_EDGE('',*,*,#9658,.F.);
#14108=ORIENTED_EDGE('',*,*,#9659,.T.);
#14109=ORIENTED_EDGE('',*,*,#9637,.F.);
#14110=ORIENTED_EDGE('',*,*,#9660,.F.);
#14111=ORIENTED_EDGE('',*,*,#9661,.F.);
#14112=ORIENTED_EDGE('',*,*,#9638,.F.);
#14113=ORIENTED_EDGE('',*,*,#9659,.F.);
#14114=ORIENTED_EDGE('',*,*,#9662,.F.);
#14115=ORIENTED_EDGE('',*,*,#9663,.T.);
#14116=ORIENTED_EDGE('',*,*,#9663,.F.);
#14117=ORIENTED_EDGE('',*,*,#9661,.T.);
#14118=ORIENTED_EDGE('',*,*,#9664,.F.);
#14119=ORIENTED_EDGE('',*,*,#9665,.T.);
#14120=ORIENTED_EDGE('',*,*,#9639,.F.);
#14121=ORIENTED_EDGE('',*,*,#9666,.F.);
#14122=ORIENTED_EDGE('',*,*,#9667,.F.);
#14123=ORIENTED_EDGE('',*,*,#9613,.F.);
#14124=ORIENTED_EDGE('',*,*,#9640,.F.);
#14125=ORIENTED_EDGE('',*,*,#9665,.F.);
#14126=ORIENTED_EDGE('',*,*,#9668,.F.);
#14127=ORIENTED_EDGE('',*,*,#9669,.T.);
#14128=ORIENTED_EDGE('',*,*,#9669,.F.);
#14129=ORIENTED_EDGE('',*,*,#9667,.T.);
#14130=ORIENTED_EDGE('',*,*,#9670,.F.);
#14131=ORIENTED_EDGE('',*,*,#9671,.T.);
#14132=ORIENTED_EDGE('',*,*,#9614,.F.);
#14133=ORIENTED_EDGE('',*,*,#9672,.F.);
#14134=ORIENTED_EDGE('',*,*,#9673,.F.);
#14135=ORIENTED_EDGE('',*,*,#9615,.F.);
#14136=ORIENTED_EDGE('',*,*,#9671,.F.);
#14137=ORIENTED_EDGE('',*,*,#9674,.F.);
#14138=ORIENTED_EDGE('',*,*,#9675,.T.);
#14139=ORIENTED_EDGE('',*,*,#9675,.F.);
#14140=ORIENTED_EDGE('',*,*,#9673,.T.);
#14141=ORIENTED_EDGE('',*,*,#9676,.F.);
#14142=ORIENTED_EDGE('',*,*,#9677,.T.);
#14143=ORIENTED_EDGE('',*,*,#9616,.F.);
#14144=ORIENTED_EDGE('',*,*,#9678,.F.);
#14145=ORIENTED_EDGE('',*,*,#9679,.F.);
#14146=ORIENTED_EDGE('',*,*,#9617,.F.);
#14147=ORIENTED_EDGE('',*,*,#9677,.F.);
#14148=ORIENTED_EDGE('',*,*,#9680,.F.);
#14149=ORIENTED_EDGE('',*,*,#9681,.T.);
#14150=ORIENTED_EDGE('',*,*,#9681,.F.);
#14151=ORIENTED_EDGE('',*,*,#9679,.T.);
#14152=ORIENTED_EDGE('',*,*,#9682,.F.);
#14153=ORIENTED_EDGE('',*,*,#9683,.T.);
#14154=ORIENTED_EDGE('',*,*,#9684,.T.);
#14155=ORIENTED_EDGE('',*,*,#9618,.F.);
#14156=ORIENTED_EDGE('',*,*,#9685,.F.);
#14157=ORIENTED_EDGE('',*,*,#9686,.F.);
#14158=ORIENTED_EDGE('',*,*,#9619,.F.);
#14159=ORIENTED_EDGE('',*,*,#9684,.F.);
#14160=ORIENTED_EDGE('',*,*,#9687,.T.);
#14161=ORIENTED_EDGE('',*,*,#9687,.F.);
#14162=ORIENTED_EDGE('',*,*,#9683,.F.);
#14163=ORIENTED_EDGE('',*,*,#9686,.T.);
#14164=ORIENTED_EDGE('',*,*,#9688,.F.);
#14165=ORIENTED_EDGE('',*,*,#9689,.T.);
#14166=ORIENTED_EDGE('',*,*,#9620,.F.);
#14167=ORIENTED_EDGE('',*,*,#9690,.F.);
#14168=ORIENTED_EDGE('',*,*,#9691,.F.);
#14169=ORIENTED_EDGE('',*,*,#9622,.F.);
#14170=ORIENTED_EDGE('',*,*,#9692,.T.);
#14171=ORIENTED_EDGE('',*,*,#9692,.F.);
#14172=ORIENTED_EDGE('',*,*,#9621,.F.);
#14173=ORIENTED_EDGE('',*,*,#9689,.F.);
#14174=ORIENTED_EDGE('',*,*,#9691,.T.);
#14175=ORIENTED_EDGE('',*,*,#9693,.F.);
#14176=ORIENTED_EDGE('',*,*,#9694,.T.);
#14177=ORIENTED_EDGE('',*,*,#9623,.F.);
#14178=ORIENTED_EDGE('',*,*,#9695,.F.);
#14179=ORIENTED_EDGE('',*,*,#9696,.F.);
#14180=ORIENTED_EDGE('',*,*,#9625,.F.);
#14181=ORIENTED_EDGE('',*,*,#9697,.T.);
#14182=ORIENTED_EDGE('',*,*,#9697,.F.);
#14183=ORIENTED_EDGE('',*,*,#9624,.F.);
#14184=ORIENTED_EDGE('',*,*,#9694,.F.);
#14185=ORIENTED_EDGE('',*,*,#9696,.T.);
#14186=ORIENTED_EDGE('',*,*,#9698,.F.);
#14187=ORIENTED_EDGE('',*,*,#9699,.T.);
#14188=ORIENTED_EDGE('',*,*,#9626,.F.);
#14189=ORIENTED_EDGE('',*,*,#9700,.F.);
#14190=ORIENTED_EDGE('',*,*,#9701,.F.);
#14191=ORIENTED_EDGE('',*,*,#9628,.F.);
#14192=ORIENTED_EDGE('',*,*,#9702,.T.);
#14193=ORIENTED_EDGE('',*,*,#9702,.F.);
#14194=ORIENTED_EDGE('',*,*,#9627,.F.);
#14195=ORIENTED_EDGE('',*,*,#9699,.F.);
#14196=ORIENTED_EDGE('',*,*,#9703,.F.);
#14197=ORIENTED_EDGE('',*,*,#9704,.T.);
#14198=ORIENTED_EDGE('',*,*,#9668,.T.);
#14199=ORIENTED_EDGE('',*,*,#9664,.T.);
#14200=ORIENTED_EDGE('',*,*,#9660,.T.);
#14201=ORIENTED_EDGE('',*,*,#9662,.T.);
#14202=ORIENTED_EDGE('',*,*,#9658,.T.);
#14203=ORIENTED_EDGE('',*,*,#9654,.T.);
#14204=ORIENTED_EDGE('',*,*,#9656,.T.);
#14205=ORIENTED_EDGE('',*,*,#9652,.T.);
#14206=ORIENTED_EDGE('',*,*,#9648,.T.);
#14207=ORIENTED_EDGE('',*,*,#9646,.T.);
#14208=ORIENTED_EDGE('',*,*,#9643,.T.);
#14209=ORIENTED_EDGE('',*,*,#9641,.T.);
#14210=ORIENTED_EDGE('',*,*,#9605,.T.);
#14211=ORIENTED_EDGE('',*,*,#9705,.T.);
#14212=ORIENTED_EDGE('',*,*,#9700,.T.);
#14213=ORIENTED_EDGE('',*,*,#9698,.T.);
#14214=ORIENTED_EDGE('',*,*,#9695,.T.);
#14215=ORIENTED_EDGE('',*,*,#9693,.T.);
#14216=ORIENTED_EDGE('',*,*,#9690,.T.);
#14217=ORIENTED_EDGE('',*,*,#9688,.T.);
#14218=ORIENTED_EDGE('',*,*,#9685,.T.);
#14219=ORIENTED_EDGE('',*,*,#9682,.T.);
#14220=ORIENTED_EDGE('',*,*,#9678,.T.);
#14221=ORIENTED_EDGE('',*,*,#9680,.T.);
#14222=ORIENTED_EDGE('',*,*,#9676,.T.);
#14223=ORIENTED_EDGE('',*,*,#9672,.T.);
#14224=ORIENTED_EDGE('',*,*,#9674,.T.);
#14225=ORIENTED_EDGE('',*,*,#9670,.T.);
#14226=ORIENTED_EDGE('',*,*,#9666,.T.);
#14227=ORIENTED_EDGE('',*,*,#9704,.F.);
#14228=ORIENTED_EDGE('',*,*,#9703,.T.);
#14229=ORIENTED_EDGE('',*,*,#9611,.T.);
#14230=ORIENTED_EDGE('',*,*,#9610,.T.);
#14231=ORIENTED_EDGE('',*,*,#9629,.F.);
#14232=ORIENTED_EDGE('',*,*,#9701,.T.);
#14233=ORIENTED_EDGE('',*,*,#9705,.F.);
#14234=ORIENTED_EDGE('',*,*,#9706,.F.);
#14235=ORIENTED_EDGE('',*,*,#9707,.T.);
#14236=ORIENTED_EDGE('',*,*,#9708,.T.);
#14237=ORIENTED_EDGE('',*,*,#9707,.F.);
#14238=ORIENTED_EDGE('',*,*,#9709,.F.);
#14239=ORIENTED_EDGE('',*,*,#9710,.T.);
#14240=ORIENTED_EDGE('',*,*,#9711,.T.);
#14241=ORIENTED_EDGE('',*,*,#9710,.F.);
#14242=ORIENTED_EDGE('',*,*,#9709,.T.);
#14243=ORIENTED_EDGE('',*,*,#9706,.T.);
#14244=ORIENTED_EDGE('',*,*,#9711,.F.);
#14245=ORIENTED_EDGE('',*,*,#9708,.F.);
#14246=ORIENTED_EDGE('',*,*,#9712,.F.);
#14247=ORIENTED_EDGE('',*,*,#9713,.T.);
#14248=ORIENTED_EDGE('',*,*,#9714,.T.);
#14249=ORIENTED_EDGE('',*,*,#9715,.T.);
#14250=ORIENTED_EDGE('',*,*,#9716,.F.);
#14251=ORIENTED_EDGE('',*,*,#9717,.T.);
#14252=ORIENTED_EDGE('',*,*,#9712,.T.);
#14253=ORIENTED_EDGE('',*,*,#9718,.T.);
#14254=ORIENTED_EDGE('',*,*,#9719,.F.);
#14255=ORIENTED_EDGE('',*,*,#9720,.T.);
#14256=ORIENTED_EDGE('',*,*,#9716,.T.);
#14257=ORIENTED_EDGE('',*,*,#9721,.T.);
#14258=ORIENTED_EDGE('',*,*,#9722,.F.);
#14259=ORIENTED_EDGE('',*,*,#9723,.T.);
#14260=ORIENTED_EDGE('',*,*,#9719,.T.);
#14261=ORIENTED_EDGE('',*,*,#9724,.T.);
#14262=ORIENTED_EDGE('',*,*,#9725,.F.);
#14263=ORIENTED_EDGE('',*,*,#9726,.T.);
#14264=ORIENTED_EDGE('',*,*,#9722,.T.);
#14265=ORIENTED_EDGE('',*,*,#9727,.T.);
#14266=ORIENTED_EDGE('',*,*,#9728,.F.);
#14267=ORIENTED_EDGE('',*,*,#9729,.T.);
#14268=ORIENTED_EDGE('',*,*,#9725,.T.);
#14269=ORIENTED_EDGE('',*,*,#9730,.T.);
#14270=ORIENTED_EDGE('',*,*,#9731,.F.);
#14271=ORIENTED_EDGE('',*,*,#9732,.T.);
#14272=ORIENTED_EDGE('',*,*,#9728,.T.);
#14273=ORIENTED_EDGE('',*,*,#9733,.T.);
#14274=ORIENTED_EDGE('',*,*,#9734,.F.);
#14275=ORIENTED_EDGE('',*,*,#9735,.T.);
#14276=ORIENTED_EDGE('',*,*,#9731,.T.);
#14277=ORIENTED_EDGE('',*,*,#9736,.T.);
#14278=ORIENTED_EDGE('',*,*,#9737,.F.);
#14279=ORIENTED_EDGE('',*,*,#9738,.T.);
#14280=ORIENTED_EDGE('',*,*,#9734,.T.);
#14281=ORIENTED_EDGE('',*,*,#9739,.T.);
#14282=ORIENTED_EDGE('',*,*,#9740,.F.);
#14283=ORIENTED_EDGE('',*,*,#9741,.T.);
#14284=ORIENTED_EDGE('',*,*,#9737,.T.);
#14285=ORIENTED_EDGE('',*,*,#9742,.T.);
#14286=ORIENTED_EDGE('',*,*,#9743,.F.);
#14287=ORIENTED_EDGE('',*,*,#9744,.T.);
#14288=ORIENTED_EDGE('',*,*,#9740,.T.);
#14289=ORIENTED_EDGE('',*,*,#9745,.T.);
#14290=ORIENTED_EDGE('',*,*,#9746,.F.);
#14291=ORIENTED_EDGE('',*,*,#9747,.T.);
#14292=ORIENTED_EDGE('',*,*,#9743,.T.);
#14293=ORIENTED_EDGE('',*,*,#9748,.T.);
#14294=ORIENTED_EDGE('',*,*,#9749,.F.);
#14295=ORIENTED_EDGE('',*,*,#9750,.T.);
#14296=ORIENTED_EDGE('',*,*,#9746,.T.);
#14297=ORIENTED_EDGE('',*,*,#9751,.T.);
#14298=ORIENTED_EDGE('',*,*,#9752,.F.);
#14299=ORIENTED_EDGE('',*,*,#9753,.T.);
#14300=ORIENTED_EDGE('',*,*,#9749,.T.);
#14301=ORIENTED_EDGE('',*,*,#9754,.T.);
#14302=ORIENTED_EDGE('',*,*,#9755,.F.);
#14303=ORIENTED_EDGE('',*,*,#9756,.T.);
#14304=ORIENTED_EDGE('',*,*,#9752,.T.);
#14305=ORIENTED_EDGE('',*,*,#9757,.T.);
#14306=ORIENTED_EDGE('',*,*,#9758,.F.);
#14307=ORIENTED_EDGE('',*,*,#9759,.T.);
#14308=ORIENTED_EDGE('',*,*,#9755,.T.);
#14309=ORIENTED_EDGE('',*,*,#9760,.T.);
#14310=ORIENTED_EDGE('',*,*,#9761,.F.);
#14311=ORIENTED_EDGE('',*,*,#9762,.T.);
#14312=ORIENTED_EDGE('',*,*,#9763,.T.);
#14313=ORIENTED_EDGE('',*,*,#9764,.F.);
#14314=ORIENTED_EDGE('',*,*,#9765,.F.);
#14315=ORIENTED_EDGE('',*,*,#9766,.T.);
#14316=ORIENTED_EDGE('',*,*,#9761,.T.);
#14317=ORIENTED_EDGE('',*,*,#9767,.F.);
#14318=ORIENTED_EDGE('',*,*,#9768,.F.);
#14319=ORIENTED_EDGE('',*,*,#9769,.T.);
#14320=ORIENTED_EDGE('',*,*,#9765,.T.);
#14321=ORIENTED_EDGE('',*,*,#9770,.F.);
#14322=ORIENTED_EDGE('',*,*,#9771,.F.);
#14323=ORIENTED_EDGE('',*,*,#9772,.T.);
#14324=ORIENTED_EDGE('',*,*,#9768,.T.);
#14325=ORIENTED_EDGE('',*,*,#9773,.F.);
#14326=ORIENTED_EDGE('',*,*,#9774,.F.);
#14327=ORIENTED_EDGE('',*,*,#9775,.T.);
#14328=ORIENTED_EDGE('',*,*,#9771,.T.);
#14329=ORIENTED_EDGE('',*,*,#9776,.F.);
#14330=ORIENTED_EDGE('',*,*,#9777,.F.);
#14331=ORIENTED_EDGE('',*,*,#9778,.T.);
#14332=ORIENTED_EDGE('',*,*,#9774,.T.);
#14333=ORIENTED_EDGE('',*,*,#9779,.F.);
#14334=ORIENTED_EDGE('',*,*,#9780,.F.);
#14335=ORIENTED_EDGE('',*,*,#9781,.T.);
#14336=ORIENTED_EDGE('',*,*,#9777,.T.);
#14337=ORIENTED_EDGE('',*,*,#9782,.F.);
#14338=ORIENTED_EDGE('',*,*,#9783,.F.);
#14339=ORIENTED_EDGE('',*,*,#9784,.T.);
#14340=ORIENTED_EDGE('',*,*,#9780,.T.);
#14341=ORIENTED_EDGE('',*,*,#9785,.F.);
#14342=ORIENTED_EDGE('',*,*,#9786,.F.);
#14343=ORIENTED_EDGE('',*,*,#9787,.T.);
#14344=ORIENTED_EDGE('',*,*,#9783,.T.);
#14345=ORIENTED_EDGE('',*,*,#9788,.F.);
#14346=ORIENTED_EDGE('',*,*,#9789,.F.);
#14347=ORIENTED_EDGE('',*,*,#9790,.T.);
#14348=ORIENTED_EDGE('',*,*,#9786,.T.);
#14349=ORIENTED_EDGE('',*,*,#9791,.F.);
#14350=ORIENTED_EDGE('',*,*,#9792,.F.);
#14351=ORIENTED_EDGE('',*,*,#9793,.T.);
#14352=ORIENTED_EDGE('',*,*,#9789,.T.);
#14353=ORIENTED_EDGE('',*,*,#9794,.F.);
#14354=ORIENTED_EDGE('',*,*,#9795,.F.);
#14355=ORIENTED_EDGE('',*,*,#9796,.T.);
#14356=ORIENTED_EDGE('',*,*,#9792,.T.);
#14357=ORIENTED_EDGE('',*,*,#9797,.F.);
#14358=ORIENTED_EDGE('',*,*,#9798,.F.);
#14359=ORIENTED_EDGE('',*,*,#9799,.T.);
#14360=ORIENTED_EDGE('',*,*,#9795,.T.);
#14361=ORIENTED_EDGE('',*,*,#9800,.F.);
#14362=ORIENTED_EDGE('',*,*,#9801,.F.);
#14363=ORIENTED_EDGE('',*,*,#9802,.T.);
#14364=ORIENTED_EDGE('',*,*,#9798,.T.);
#14365=ORIENTED_EDGE('',*,*,#9803,.F.);
#14366=ORIENTED_EDGE('',*,*,#9804,.F.);
#14367=ORIENTED_EDGE('',*,*,#9805,.T.);
#14368=ORIENTED_EDGE('',*,*,#9801,.T.);
#14369=ORIENTED_EDGE('',*,*,#9806,.F.);
#14370=ORIENTED_EDGE('',*,*,#9807,.F.);
#14371=ORIENTED_EDGE('',*,*,#9808,.T.);
#14372=ORIENTED_EDGE('',*,*,#9804,.T.);
#14373=ORIENTED_EDGE('',*,*,#9809,.F.);
#14374=ORIENTED_EDGE('',*,*,#9810,.F.);
#14375=ORIENTED_EDGE('',*,*,#9763,.F.);
#14376=ORIENTED_EDGE('',*,*,#9811,.F.);
#14377=ORIENTED_EDGE('',*,*,#9812,.F.);
#14378=ORIENTED_EDGE('',*,*,#9813,.F.);
#14379=ORIENTED_EDGE('',*,*,#9814,.T.);
#14380=ORIENTED_EDGE('',*,*,#9815,.F.);
#14381=ORIENTED_EDGE('',*,*,#9814,.F.);
#14382=ORIENTED_EDGE('',*,*,#9811,.T.);
#14383=ORIENTED_EDGE('',*,*,#9762,.F.);
#14384=ORIENTED_EDGE('',*,*,#9766,.F.);
#14385=ORIENTED_EDGE('',*,*,#9769,.F.);
#14386=ORIENTED_EDGE('',*,*,#9772,.F.);
#14387=ORIENTED_EDGE('',*,*,#9775,.F.);
#14388=ORIENTED_EDGE('',*,*,#9778,.F.);
#14389=ORIENTED_EDGE('',*,*,#9781,.F.);
#14390=ORIENTED_EDGE('',*,*,#9784,.F.);
#14391=ORIENTED_EDGE('',*,*,#9787,.F.);
#14392=ORIENTED_EDGE('',*,*,#9790,.F.);
#14393=ORIENTED_EDGE('',*,*,#9793,.F.);
#14394=ORIENTED_EDGE('',*,*,#9796,.F.);
#14395=ORIENTED_EDGE('',*,*,#9799,.F.);
#14396=ORIENTED_EDGE('',*,*,#9802,.F.);
#14397=ORIENTED_EDGE('',*,*,#9805,.F.);
#14398=ORIENTED_EDGE('',*,*,#9808,.F.);
#14399=ORIENTED_EDGE('',*,*,#9816,.F.);
#14400=ORIENTED_EDGE('',*,*,#9817,.F.);
#14401=ORIENTED_EDGE('',*,*,#9713,.F.);
#14402=ORIENTED_EDGE('',*,*,#9717,.F.);
#14403=ORIENTED_EDGE('',*,*,#9720,.F.);
#14404=ORIENTED_EDGE('',*,*,#9723,.F.);
#14405=ORIENTED_EDGE('',*,*,#9726,.F.);
#14406=ORIENTED_EDGE('',*,*,#9729,.F.);
#14407=ORIENTED_EDGE('',*,*,#9732,.F.);
#14408=ORIENTED_EDGE('',*,*,#9735,.F.);
#14409=ORIENTED_EDGE('',*,*,#9738,.F.);
#14410=ORIENTED_EDGE('',*,*,#9741,.F.);
#14411=ORIENTED_EDGE('',*,*,#9744,.F.);
#14412=ORIENTED_EDGE('',*,*,#9747,.F.);
#14413=ORIENTED_EDGE('',*,*,#9750,.F.);
#14414=ORIENTED_EDGE('',*,*,#9753,.F.);
#14415=ORIENTED_EDGE('',*,*,#9756,.F.);
#14416=ORIENTED_EDGE('',*,*,#9759,.F.);
#14417=ORIENTED_EDGE('',*,*,#9818,.F.);
#14418=ORIENTED_EDGE('',*,*,#9807,.T.);
#14419=ORIENTED_EDGE('',*,*,#9819,.F.);
#14420=ORIENTED_EDGE('',*,*,#9820,.F.);
#14421=ORIENTED_EDGE('',*,*,#9816,.T.);
#14422=ORIENTED_EDGE('',*,*,#9810,.T.);
#14423=ORIENTED_EDGE('',*,*,#9813,.T.);
#14424=ORIENTED_EDGE('',*,*,#9821,.F.);
#14425=ORIENTED_EDGE('',*,*,#9760,.F.);
#14426=ORIENTED_EDGE('',*,*,#9757,.F.);
#14427=ORIENTED_EDGE('',*,*,#9754,.F.);
#14428=ORIENTED_EDGE('',*,*,#9751,.F.);
#14429=ORIENTED_EDGE('',*,*,#9748,.F.);
#14430=ORIENTED_EDGE('',*,*,#9745,.F.);
#14431=ORIENTED_EDGE('',*,*,#9742,.F.);
#14432=ORIENTED_EDGE('',*,*,#9739,.F.);
#14433=ORIENTED_EDGE('',*,*,#9736,.F.);
#14434=ORIENTED_EDGE('',*,*,#9733,.F.);
#14435=ORIENTED_EDGE('',*,*,#9730,.F.);
#14436=ORIENTED_EDGE('',*,*,#9727,.F.);
#14437=ORIENTED_EDGE('',*,*,#9724,.F.);
#14438=ORIENTED_EDGE('',*,*,#9721,.F.);
#14439=ORIENTED_EDGE('',*,*,#9718,.F.);
#14440=ORIENTED_EDGE('',*,*,#9715,.F.);
#14441=ORIENTED_EDGE('',*,*,#9822,.F.);
#14442=ORIENTED_EDGE('',*,*,#9819,.T.);
#14443=ORIENTED_EDGE('',*,*,#9809,.T.);
#14444=ORIENTED_EDGE('',*,*,#9806,.T.);
#14445=ORIENTED_EDGE('',*,*,#9803,.T.);
#14446=ORIENTED_EDGE('',*,*,#9800,.T.);
#14447=ORIENTED_EDGE('',*,*,#9797,.T.);
#14448=ORIENTED_EDGE('',*,*,#9794,.T.);
#14449=ORIENTED_EDGE('',*,*,#9791,.T.);
#14450=ORIENTED_EDGE('',*,*,#9788,.T.);
#14451=ORIENTED_EDGE('',*,*,#9785,.T.);
#14452=ORIENTED_EDGE('',*,*,#9782,.T.);
#14453=ORIENTED_EDGE('',*,*,#9779,.T.);
#14454=ORIENTED_EDGE('',*,*,#9776,.T.);
#14455=ORIENTED_EDGE('',*,*,#9773,.T.);
#14456=ORIENTED_EDGE('',*,*,#9770,.T.);
#14457=ORIENTED_EDGE('',*,*,#9767,.T.);
#14458=ORIENTED_EDGE('',*,*,#9764,.T.);
#14459=ORIENTED_EDGE('',*,*,#9758,.T.);
#14460=ORIENTED_EDGE('',*,*,#9821,.T.);
#14461=ORIENTED_EDGE('',*,*,#9812,.T.);
#14462=ORIENTED_EDGE('',*,*,#9818,.T.);
#14463=ORIENTED_EDGE('',*,*,#9823,.F.);
#14464=ORIENTED_EDGE('',*,*,#9824,.T.);
#14465=ORIENTED_EDGE('',*,*,#9825,.T.);
#14466=ORIENTED_EDGE('',*,*,#9826,.F.);
#14467=ORIENTED_EDGE('',*,*,#9827,.F.);
#14468=ORIENTED_EDGE('',*,*,#9828,.T.);
#14469=ORIENTED_EDGE('',*,*,#9829,.T.);
#14470=ORIENTED_EDGE('',*,*,#9824,.F.);
#14471=ORIENTED_EDGE('',*,*,#9830,.F.);
#14472=ORIENTED_EDGE('',*,*,#9831,.T.);
#14473=ORIENTED_EDGE('',*,*,#9832,.T.);
#14474=ORIENTED_EDGE('',*,*,#9828,.F.);
#14475=ORIENTED_EDGE('',*,*,#9833,.F.);
#14476=ORIENTED_EDGE('',*,*,#9834,.T.);
#14477=ORIENTED_EDGE('',*,*,#9835,.T.);
#14478=ORIENTED_EDGE('',*,*,#9831,.F.);
#14479=ORIENTED_EDGE('',*,*,#9836,.F.);
#14480=ORIENTED_EDGE('',*,*,#9837,.T.);
#14481=ORIENTED_EDGE('',*,*,#9838,.T.);
#14482=ORIENTED_EDGE('',*,*,#9834,.F.);
#14483=ORIENTED_EDGE('',*,*,#9839,.F.);
#14484=ORIENTED_EDGE('',*,*,#9826,.T.);
#14485=ORIENTED_EDGE('',*,*,#9840,.T.);
#14486=ORIENTED_EDGE('',*,*,#9837,.F.);
#14487=ORIENTED_EDGE('',*,*,#9840,.F.);
#14488=ORIENTED_EDGE('',*,*,#9825,.F.);
#14489=ORIENTED_EDGE('',*,*,#9829,.F.);
#14490=ORIENTED_EDGE('',*,*,#9832,.F.);
#14491=ORIENTED_EDGE('',*,*,#9835,.F.);
#14492=ORIENTED_EDGE('',*,*,#9838,.F.);
#14493=ORIENTED_EDGE('',*,*,#9841,.T.);
#14494=ORIENTED_EDGE('',*,*,#9817,.T.);
#14495=ORIENTED_EDGE('',*,*,#9820,.T.);
#14496=ORIENTED_EDGE('',*,*,#9822,.T.);
#14497=ORIENTED_EDGE('',*,*,#9714,.F.);
#14498=ORIENTED_EDGE('',*,*,#9841,.F.);
#14499=ORIENTED_EDGE('',*,*,#9842,.T.);
#14500=ORIENTED_EDGE('',*,*,#9843,.T.);
#14501=ORIENTED_EDGE('',*,*,#9842,.F.);
#14502=ORIENTED_EDGE('',*,*,#9843,.F.);
#14503=ORIENTED_EDGE('',*,*,#9823,.T.);
#14504=ORIENTED_EDGE('',*,*,#9839,.T.);
#14505=ORIENTED_EDGE('',*,*,#9836,.T.);
#14506=ORIENTED_EDGE('',*,*,#9833,.T.);
#14507=ORIENTED_EDGE('',*,*,#9830,.T.);
#14508=ORIENTED_EDGE('',*,*,#9827,.T.);
#14509=ORIENTED_EDGE('',*,*,#9815,.T.);
#14510=PLANE('',#15697);
#14511=PLANE('',#15698);
#14512=PLANE('',#15701);
#14513=PLANE('',#15702);
#14514=PLANE('',#15703);
#14515=PLANE('',#15706);
#14516=PLANE('',#15735);
#14517=PLANE('',#15736);
#14518=PLANE('',#15737);
#14519=PLANE('',#15738);
#14520=PLANE('',#15739);
#14521=PLANE('',#15741);
#14522=PLANE('',#15750);
#14523=PLANE('',#15751);
#14524=PLANE('',#16116);
#14525=PLANE('',#16119);
#14526=PLANE('',#16122);
#14527=PLANE('',#16125);
#14528=PLANE('',#16128);
#14529=PLANE('',#16129);
#14530=PLANE('',#16130);
#14531=PLANE('',#16131);
#14532=PLANE('',#16132);
#14533=PLANE('',#16135);
#14534=PLANE('',#16138);
#14535=PLANE('',#16141);
#14536=PLANE('',#16144);
#14537=PLANE('',#16145);
#14538=PLANE('',#16146);
#14539=PLANE('',#16147);
#14540=PLANE('',#16148);
#14541=PLANE('',#16149);
#14542=PLANE('',#16150);
#14543=PLANE('',#16151);
#14544=PLANE('',#16155);
#14545=PLANE('',#16158);
#14546=PLANE('',#16159);
#14547=PLANE('',#16160);
#14548=PLANE('',#16161);
#14549=PLANE('',#16163);
#14550=PLANE('',#16166);
#14551=PLANE('',#16172);
#14552=PLANE('',#16174);
#14553=PLANE('',#16183);
#14554=PLANE('',#16228);
#14555=PLANE('',#16230);
#14556=PLANE('',#16234);
#14557=PLANE('',#16235);
#14558=PLANE('',#16236);
#14559=PLANE('',#16238);
#14560=PLANE('',#16239);
#14561=PLANE('',#16243);
#14562=PLANE('',#16245);
#14563=PLANE('',#16249);
#14564=PLANE('',#16252);
#14565=PLANE('',#16253);
#14566=PLANE('',#16256);
#14567=PLANE('',#16262);
#14568=PLANE('',#16266);
#14569=PLANE('',#16275);
#14570=PLANE('',#16276);
#14571=PLANE('',#16284);
#14572=PLANE('',#16285);
#14573=PLANE('',#16287);
#14574=PLANE('',#16288);
#14575=PLANE('',#16289);
#14576=PLANE('',#16296);
#14577=PLANE('',#16298);
#14578=PLANE('',#16299);
#14579=PLANE('',#16300);
#14580=PLANE('',#16301);
#14581=PLANE('',#16302);
#14582=PLANE('',#16303);
#14583=PLANE('',#16471);
#14584=PLANE('',#16476);
#14585=PLANE('',#16477);
#14586=PLANE('',#16481);
#14587=PLANE('',#16502);
#14588=PLANE('',#16507);
#14589=PLANE('',#16508);
#14590=PLANE('',#16518);
#14591=PLANE('',#16519);
#14592=PLANE('',#16521);
#14593=PLANE('',#16522);
#14594=PLANE('',#16523);
#14595=PLANE('',#16530);
#14596=PLANE('',#16570);
#14597=PLANE('',#16571);
#14598=PLANE('',#16572);
#14599=PLANE('',#16573);
#14600=PLANE('',#16574);
#14601=PLANE('',#16575);
#14602=PLANE('',#16576);
#14603=PLANE('',#16579);
#14604=PLANE('',#16582);
#14605=PLANE('',#16584);
#14606=PLANE('',#16591);
#14607=PLANE('',#16598);
#14608=PLANE('',#16605);
#14609=PLANE('',#16618);
#14610=PLANE('',#16619);
#14611=PLANE('',#16632);
#14612=PLANE('',#16633);
#14613=PLANE('',#16646);
#14614=PLANE('',#16647);
#14615=PLANE('',#16670);
#14616=PLANE('',#16676);
#14617=PLANE('',#16683);
#14618=PLANE('',#16689);
#14619=PLANE('',#16695);
#14620=PLANE('',#16701);
#14621=PLANE('',#16707);
#14622=PLANE('',#16713);
#14623=PLANE('',#16720);
#14624=PLANE('',#16726);
#14625=PLANE('',#16732);
#14626=PLANE('',#16741);
#14627=PLANE('',#16742);
#14628=PLANE('',#16750);
#14629=PLANE('',#16751);
#14630=PLANE('',#16793);
#14631=PLANE('',#16794);
#14632=PLANE('',#16795);
#14633=PLANE('',#16796);
#14634=PLANE('',#16797);
#14635=PLANE('',#16798);
#14636=PLANE('',#16799);
#14637=PLANE('',#16800);
#14638=PLANE('',#16804);
#14639=PLANE('',#16805);
#14640=ADVANCED_FACE('',(#2660),#14510,.F.);
#14641=ADVANCED_FACE('',(#2661),#14511,.F.);
#14642=ADVANCED_FACE('',(#2662),#14512,.F.);
#14643=ADVANCED_FACE('',(#2663),#14513,.F.);
#14644=ADVANCED_FACE('',(#2664),#14514,.F.);
#14645=ADVANCED_FACE('',(#2665),#14515,.F.);
#14646=ADVANCED_FACE('',(#2666),#1715,.F.);
#14647=ADVANCED_FACE('',(#2667),#1716,.T.);
#14648=ADVANCED_FACE('',(#2668),#1717,.F.);
#14649=ADVANCED_FACE('',(#2669),#1718,.F.);
#14650=ADVANCED_FACE('',(#2670),#1719,.F.);
#14651=ADVANCED_FACE('',(#2671),#1720,.F.);
#14652=ADVANCED_FACE('',(#2672),#1721,.F.);
#14653=ADVANCED_FACE('',(#2673),#1722,.F.);
#14654=ADVANCED_FACE('',(#2674),#14516,.T.);
#14655=ADVANCED_FACE('',(#2675),#14517,.T.);
#14656=ADVANCED_FACE('',(#2676),#14518,.T.);
#14657=ADVANCED_FACE('',(#2677,#1628),#14519,.F.);
#14658=ADVANCED_FACE('',(#2678,#1629,#1630,#1631,#1632,#1633,#1634),#14520,
 .T.);
#14659=ADVANCED_FACE('',(#2679,#1635,#1636,#1637,#1638,#1639,#1640),#14521,
 .F.);
#14660=ADVANCED_FACE('',(#2680),#1723,.T.);
#14661=ADVANCED_FACE('',(#2681),#1724,.T.);
#14662=ADVANCED_FACE('',(#2682),#1725,.F.);
#14663=ADVANCED_FACE('',(#2683,#1641,#1642),#14522,.T.);
#14664=ADVANCED_FACE('',(#2684,#1643),#14523,.F.);
#14665=ADVANCED_FACE('',(#2685),#1726,.F.);
#14666=ADVANCED_FACE('',(#2686),#1727,.F.);
#14667=ADVANCED_FACE('',(#2687),#1728,.F.);
#14668=ADVANCED_FACE('',(#2688),#1729,.F.);
#14669=ADVANCED_FACE('',(#2689),#1730,.F.);
#14670=ADVANCED_FACE('',(#2690),#1731,.F.);
#14671=ADVANCED_FACE('',(#2691),#1732,.F.);
#14672=ADVANCED_FACE('',(#2692),#1733,.F.);
#14673=ADVANCED_FACE('',(#2693),#1734,.F.);
#14674=ADVANCED_FACE('',(#2694),#1735,.F.);
#14675=ADVANCED_FACE('',(#2695),#1736,.F.);
#14676=ADVANCED_FACE('',(#2696),#1737,.F.);
#14677=ADVANCED_FACE('',(#2697),#1738,.F.);
#14678=ADVANCED_FACE('',(#2698),#1739,.F.);
#14679=ADVANCED_FACE('',(#2699),#1740,.F.);
#14680=ADVANCED_FACE('',(#2700),#1741,.F.);
#14681=ADVANCED_FACE('',(#2701),#1742,.F.);
#14682=ADVANCED_FACE('',(#2702),#1743,.F.);
#14683=ADVANCED_FACE('',(#2703),#1744,.F.);
#14684=ADVANCED_FACE('',(#2704),#1745,.F.);
#14685=ADVANCED_FACE('',(#2705),#1746,.F.);
#14686=ADVANCED_FACE('',(#2706),#1747,.F.);
#14687=ADVANCED_FACE('',(#2707),#1748,.F.);
#14688=ADVANCED_FACE('',(#2708),#1749,.F.);
#14689=ADVANCED_FACE('',(#2709),#1750,.F.);
#14690=ADVANCED_FACE('',(#2710),#1751,.F.);
#14691=ADVANCED_FACE('',(#2711),#1752,.F.);
#14692=ADVANCED_FACE('',(#2712),#1753,.F.);
#14693=ADVANCED_FACE('',(#2713),#1754,.F.);
#14694=ADVANCED_FACE('',(#2714),#1755,.F.);
#14695=ADVANCED_FACE('',(#2715),#1756,.F.);
#14696=ADVANCED_FACE('',(#2716),#1757,.F.);
#14697=ADVANCED_FACE('',(#2717),#1758,.F.);
#14698=ADVANCED_FACE('',(#2718),#1759,.F.);
#14699=ADVANCED_FACE('',(#2719),#1760,.F.);
#14700=ADVANCED_FACE('',(#2720),#1761,.F.);
#14701=ADVANCED_FACE('',(#2721),#1762,.F.);
#14702=ADVANCED_FACE('',(#2722),#1763,.F.);
#14703=ADVANCED_FACE('',(#2723),#1764,.F.);
#14704=ADVANCED_FACE('',(#2724),#1765,.F.);
#14705=ADVANCED_FACE('',(#2725),#1766,.F.);
#14706=ADVANCED_FACE('',(#2726),#1767,.F.);
#14707=ADVANCED_FACE('',(#2727),#1768,.F.);
#14708=ADVANCED_FACE('',(#2728),#1769,.F.);
#14709=ADVANCED_FACE('',(#2729),#1770,.F.);
#14710=ADVANCED_FACE('',(#2730),#1771,.F.);
#14711=ADVANCED_FACE('',(#2731),#1772,.F.);
#14712=ADVANCED_FACE('',(#2732),#1773,.F.);
#14713=ADVANCED_FACE('',(#2733),#1774,.F.);
#14714=ADVANCED_FACE('',(#2734),#1775,.F.);
#14715=ADVANCED_FACE('',(#2735),#1776,.F.);
#14716=ADVANCED_FACE('',(#2736),#1777,.F.);
#14717=ADVANCED_FACE('',(#2737),#1778,.F.);
#14718=ADVANCED_FACE('',(#2738),#1779,.F.);
#14719=ADVANCED_FACE('',(#2739),#1780,.F.);
#14720=ADVANCED_FACE('',(#2740),#1781,.F.);
#14721=ADVANCED_FACE('',(#2741),#1782,.F.);
#14722=ADVANCED_FACE('',(#2742),#1783,.F.);
#14723=ADVANCED_FACE('',(#2743),#1784,.F.);
#14724=ADVANCED_FACE('',(#2744),#1785,.F.);
#14725=ADVANCED_FACE('',(#2745),#1786,.F.);
#14726=ADVANCED_FACE('',(#2746),#1787,.F.);
#14727=ADVANCED_FACE('',(#2747),#1788,.F.);
#14728=ADVANCED_FACE('',(#2748),#1789,.F.);
#14729=ADVANCED_FACE('',(#2749),#1790,.F.);
#14730=ADVANCED_FACE('',(#2750),#1791,.F.);
#14731=ADVANCED_FACE('',(#2751),#1792,.F.);
#14732=ADVANCED_FACE('',(#2752),#1793,.F.);
#14733=ADVANCED_FACE('',(#2753),#1794,.F.);
#14734=ADVANCED_FACE('',(#2754),#1795,.F.);
#14735=ADVANCED_FACE('',(#2755),#1796,.F.);
#14736=ADVANCED_FACE('',(#2756),#1797,.F.);
#14737=ADVANCED_FACE('',(#2757),#1798,.F.);
#14738=ADVANCED_FACE('',(#2758),#1799,.F.);
#14739=ADVANCED_FACE('',(#2759),#1800,.F.);
#14740=ADVANCED_FACE('',(#2760),#1801,.F.);
#14741=ADVANCED_FACE('',(#2761),#1802,.F.);
#14742=ADVANCED_FACE('',(#2762),#1803,.F.);
#14743=ADVANCED_FACE('',(#2763),#1804,.F.);
#14744=ADVANCED_FACE('',(#2764),#1805,.F.);
#14745=ADVANCED_FACE('',(#2765),#1806,.F.);
#14746=ADVANCED_FACE('',(#2766),#1807,.F.);
#14747=ADVANCED_FACE('',(#2767),#1808,.F.);
#14748=ADVANCED_FACE('',(#2768),#1809,.F.);
#14749=ADVANCED_FACE('',(#2769),#1810,.F.);
#14750=ADVANCED_FACE('',(#2770),#1811,.F.);
#14751=ADVANCED_FACE('',(#2771),#1812,.F.);
#14752=ADVANCED_FACE('',(#2772),#1813,.F.);
#14753=ADVANCED_FACE('',(#2773),#1814,.F.);
#14754=ADVANCED_FACE('',(#2774),#1815,.F.);
#14755=ADVANCED_FACE('',(#2775),#1816,.F.);
#14756=ADVANCED_FACE('',(#2776),#1817,.F.);
#14757=ADVANCED_FACE('',(#2777),#1818,.F.);
#14758=ADVANCED_FACE('',(#2778),#1819,.F.);
#14759=ADVANCED_FACE('',(#2779),#1820,.F.);
#14760=ADVANCED_FACE('',(#2780),#1821,.F.);
#14761=ADVANCED_FACE('',(#2781),#1822,.F.);
#14762=ADVANCED_FACE('',(#2782),#1823,.F.);
#14763=ADVANCED_FACE('',(#2783),#1824,.F.);
#14764=ADVANCED_FACE('',(#2784),#1825,.F.);
#14765=ADVANCED_FACE('',(#2785),#1826,.F.);
#14766=ADVANCED_FACE('',(#2786),#1827,.F.);
#14767=ADVANCED_FACE('',(#2787),#1828,.F.);
#14768=ADVANCED_FACE('',(#2788),#1829,.F.);
#14769=ADVANCED_FACE('',(#2789),#1830,.F.);
#14770=ADVANCED_FACE('',(#2790),#1831,.F.);
#14771=ADVANCED_FACE('',(#2791),#1832,.F.);
#14772=ADVANCED_FACE('',(#2792),#1833,.F.);
#14773=ADVANCED_FACE('',(#2793),#1834,.F.);
#14774=ADVANCED_FACE('',(#2794),#1835,.F.);
#14775=ADVANCED_FACE('',(#2795),#1836,.F.);
#14776=ADVANCED_FACE('',(#2796),#1837,.F.);
#14777=ADVANCED_FACE('',(#2797),#1838,.F.);
#14778=ADVANCED_FACE('',(#2798),#1839,.F.);
#14779=ADVANCED_FACE('',(#2799),#1840,.F.);
#14780=ADVANCED_FACE('',(#2800),#1841,.F.);
#14781=ADVANCED_FACE('',(#2801),#1842,.F.);
#14782=ADVANCED_FACE('',(#2802),#1843,.F.);
#14783=ADVANCED_FACE('',(#2803),#1844,.F.);
#14784=ADVANCED_FACE('',(#2804),#1845,.F.);
#14785=ADVANCED_FACE('',(#2805),#1846,.F.);
#14786=ADVANCED_FACE('',(#2806),#1847,.F.);
#14787=ADVANCED_FACE('',(#2807),#1848,.F.);
#14788=ADVANCED_FACE('',(#2808),#1849,.F.);
#14789=ADVANCED_FACE('',(#2809),#1850,.F.);
#14790=ADVANCED_FACE('',(#2810),#1851,.F.);
#14791=ADVANCED_FACE('',(#2811),#1852,.F.);
#14792=ADVANCED_FACE('',(#2812),#1853,.F.);
#14793=ADVANCED_FACE('',(#2813),#1854,.F.);
#14794=ADVANCED_FACE('',(#2814),#1855,.F.);
#14795=ADVANCED_FACE('',(#2815),#1856,.F.);
#14796=ADVANCED_FACE('',(#2816),#1857,.F.);
#14797=ADVANCED_FACE('',(#2817),#1858,.F.);
#14798=ADVANCED_FACE('',(#2818),#1859,.F.);
#14799=ADVANCED_FACE('',(#2819),#1860,.F.);
#14800=ADVANCED_FACE('',(#2820),#1861,.F.);
#14801=ADVANCED_FACE('',(#2821),#1862,.F.);
#14802=ADVANCED_FACE('',(#2822),#1863,.F.);
#14803=ADVANCED_FACE('',(#2823),#1864,.F.);
#14804=ADVANCED_FACE('',(#2824),#1865,.F.);
#14805=ADVANCED_FACE('',(#2825),#1866,.F.);
#14806=ADVANCED_FACE('',(#2826),#1867,.F.);
#14807=ADVANCED_FACE('',(#2827),#1868,.F.);
#14808=ADVANCED_FACE('',(#2828),#1869,.F.);
#14809=ADVANCED_FACE('',(#2829),#1870,.F.);
#14810=ADVANCED_FACE('',(#2830),#1871,.F.);
#14811=ADVANCED_FACE('',(#2831),#1872,.F.);
#14812=ADVANCED_FACE('',(#2832),#1873,.F.);
#14813=ADVANCED_FACE('',(#2833),#1874,.F.);
#14814=ADVANCED_FACE('',(#2834),#1875,.F.);
#14815=ADVANCED_FACE('',(#2835),#1876,.F.);
#14816=ADVANCED_FACE('',(#2836),#1877,.F.);
#14817=ADVANCED_FACE('',(#2837),#1878,.F.);
#14818=ADVANCED_FACE('',(#2838),#1879,.F.);
#14819=ADVANCED_FACE('',(#2839),#1880,.F.);
#14820=ADVANCED_FACE('',(#2840),#1881,.F.);
#14821=ADVANCED_FACE('',(#2841),#1882,.F.);
#14822=ADVANCED_FACE('',(#2842),#1883,.F.);
#14823=ADVANCED_FACE('',(#2843),#1884,.F.);
#14824=ADVANCED_FACE('',(#2844),#1885,.F.);
#14825=ADVANCED_FACE('',(#2845),#1886,.F.);
#14826=ADVANCED_FACE('',(#2846),#1887,.F.);
#14827=ADVANCED_FACE('',(#2847),#1888,.F.);
#14828=ADVANCED_FACE('',(#2848),#1889,.F.);
#14829=ADVANCED_FACE('',(#2849),#1890,.F.);
#14830=ADVANCED_FACE('',(#2850),#1891,.F.);
#14831=ADVANCED_FACE('',(#2851),#1892,.F.);
#14832=ADVANCED_FACE('',(#2852),#1893,.F.);
#14833=ADVANCED_FACE('',(#2853),#1894,.F.);
#14834=ADVANCED_FACE('',(#2854),#1895,.F.);
#14835=ADVANCED_FACE('',(#2855),#1896,.F.);
#14836=ADVANCED_FACE('',(#2856),#1897,.F.);
#14837=ADVANCED_FACE('',(#2857),#1898,.F.);
#14838=ADVANCED_FACE('',(#2858),#1899,.F.);
#14839=ADVANCED_FACE('',(#2859),#1900,.F.);
#14840=ADVANCED_FACE('',(#2860),#1901,.F.);
#14841=ADVANCED_FACE('',(#2861),#1902,.F.);
#14842=ADVANCED_FACE('',(#2862),#1903,.F.);
#14843=ADVANCED_FACE('',(#2863),#1904,.F.);
#14844=ADVANCED_FACE('',(#2864),#1905,.F.);
#14845=ADVANCED_FACE('',(#2865),#1906,.F.);
#14846=ADVANCED_FACE('',(#2866),#1907,.F.);
#14847=ADVANCED_FACE('',(#2867),#1908,.F.);
#14848=ADVANCED_FACE('',(#2868),#1909,.F.);
#14849=ADVANCED_FACE('',(#2869),#1910,.F.);
#14850=ADVANCED_FACE('',(#2870),#1911,.F.);
#14851=ADVANCED_FACE('',(#2871),#1912,.F.);
#14852=ADVANCED_FACE('',(#2872),#1913,.F.);
#14853=ADVANCED_FACE('',(#2873),#1914,.F.);
#14854=ADVANCED_FACE('',(#2874),#1915,.F.);
#14855=ADVANCED_FACE('',(#2875),#1916,.F.);
#14856=ADVANCED_FACE('',(#2876),#1917,.F.);
#14857=ADVANCED_FACE('',(#2877),#1918,.F.);
#14858=ADVANCED_FACE('',(#2878),#1919,.F.);
#14859=ADVANCED_FACE('',(#2879),#1920,.F.);
#14860=ADVANCED_FACE('',(#2880),#1921,.F.);
#14861=ADVANCED_FACE('',(#2881),#1922,.F.);
#14862=ADVANCED_FACE('',(#2882),#1923,.F.);
#14863=ADVANCED_FACE('',(#2883),#1924,.F.);
#14864=ADVANCED_FACE('',(#2884),#1925,.F.);
#14865=ADVANCED_FACE('',(#2885),#1926,.F.);
#14866=ADVANCED_FACE('',(#2886),#1927,.F.);
#14867=ADVANCED_FACE('',(#2887),#1928,.F.);
#14868=ADVANCED_FACE('',(#2888),#1929,.F.);
#14869=ADVANCED_FACE('',(#2889),#1930,.F.);
#14870=ADVANCED_FACE('',(#2890),#1931,.F.);
#14871=ADVANCED_FACE('',(#2891),#1932,.F.);
#14872=ADVANCED_FACE('',(#2892),#1933,.F.);
#14873=ADVANCED_FACE('',(#2893),#1934,.F.);
#14874=ADVANCED_FACE('',(#2894),#1935,.F.);
#14875=ADVANCED_FACE('',(#2895),#1936,.F.);
#14876=ADVANCED_FACE('',(#2896),#1937,.F.);
#14877=ADVANCED_FACE('',(#2897),#1938,.F.);
#14878=ADVANCED_FACE('',(#2898),#1939,.F.);
#14879=ADVANCED_FACE('',(#2899),#1940,.F.);
#14880=ADVANCED_FACE('',(#2900),#1941,.F.);
#14881=ADVANCED_FACE('',(#2901),#1942,.F.);
#14882=ADVANCED_FACE('',(#2902),#1943,.F.);
#14883=ADVANCED_FACE('',(#2903),#1944,.F.);
#14884=ADVANCED_FACE('',(#2904),#1945,.F.);
#14885=ADVANCED_FACE('',(#2905),#1946,.F.);
#14886=ADVANCED_FACE('',(#2906),#1947,.F.);
#14887=ADVANCED_FACE('',(#2907),#1948,.F.);
#14888=ADVANCED_FACE('',(#2908),#1949,.F.);
#14889=ADVANCED_FACE('',(#2909),#1950,.F.);
#14890=ADVANCED_FACE('',(#2910),#1951,.F.);
#14891=ADVANCED_FACE('',(#2911),#1952,.F.);
#14892=ADVANCED_FACE('',(#2912),#1953,.F.);
#14893=ADVANCED_FACE('',(#2913),#1954,.F.);
#14894=ADVANCED_FACE('',(#2914),#1955,.F.);
#14895=ADVANCED_FACE('',(#2915),#1956,.F.);
#14896=ADVANCED_FACE('',(#2916),#1957,.F.);
#14897=ADVANCED_FACE('',(#2917),#1958,.F.);
#14898=ADVANCED_FACE('',(#2918),#1959,.F.);
#14899=ADVANCED_FACE('',(#2919),#1960,.F.);
#14900=ADVANCED_FACE('',(#2920),#1961,.F.);
#14901=ADVANCED_FACE('',(#2921),#1962,.F.);
#14902=ADVANCED_FACE('',(#2922),#1963,.F.);
#14903=ADVANCED_FACE('',(#2923),#1964,.F.);
#14904=ADVANCED_FACE('',(#2924),#1965,.F.);
#14905=ADVANCED_FACE('',(#2925),#1966,.F.);
#14906=ADVANCED_FACE('',(#2926),#1967,.F.);
#14907=ADVANCED_FACE('',(#2927),#1968,.F.);
#14908=ADVANCED_FACE('',(#2928),#1969,.F.);
#14909=ADVANCED_FACE('',(#2929),#1970,.F.);
#14910=ADVANCED_FACE('',(#2930),#1971,.F.);
#14911=ADVANCED_FACE('',(#2931),#1972,.F.);
#14912=ADVANCED_FACE('',(#2932),#1973,.F.);
#14913=ADVANCED_FACE('',(#2933),#1974,.F.);
#14914=ADVANCED_FACE('',(#2934),#1975,.F.);
#14915=ADVANCED_FACE('',(#2935),#1976,.F.);
#14916=ADVANCED_FACE('',(#2936),#1977,.F.);
#14917=ADVANCED_FACE('',(#2937),#1978,.F.);
#14918=ADVANCED_FACE('',(#2938),#1979,.F.);
#14919=ADVANCED_FACE('',(#2939),#1980,.F.);
#14920=ADVANCED_FACE('',(#2940),#1981,.F.);
#14921=ADVANCED_FACE('',(#2941),#1982,.F.);
#14922=ADVANCED_FACE('',(#2942),#1983,.F.);
#14923=ADVANCED_FACE('',(#2943),#1984,.F.);
#14924=ADVANCED_FACE('',(#2944),#1985,.F.);
#14925=ADVANCED_FACE('',(#2945),#1986,.F.);
#14926=ADVANCED_FACE('',(#2946),#1987,.F.);
#14927=ADVANCED_FACE('',(#2947),#1988,.F.);
#14928=ADVANCED_FACE('',(#2948),#1989,.F.);
#14929=ADVANCED_FACE('',(#2949),#1990,.F.);
#14930=ADVANCED_FACE('',(#2950),#1991,.F.);
#14931=ADVANCED_FACE('',(#2951),#1992,.F.);
#14932=ADVANCED_FACE('',(#2952),#1993,.F.);
#14933=ADVANCED_FACE('',(#2953),#1994,.F.);
#14934=ADVANCED_FACE('',(#2954),#1995,.F.);
#14935=ADVANCED_FACE('',(#2955),#1996,.F.);
#14936=ADVANCED_FACE('',(#2956),#1997,.F.);
#14937=ADVANCED_FACE('',(#2957),#1998,.F.);
#14938=ADVANCED_FACE('',(#2958),#1999,.F.);
#14939=ADVANCED_FACE('',(#2959),#2000,.F.);
#14940=ADVANCED_FACE('',(#2960),#2001,.F.);
#14941=ADVANCED_FACE('',(#2961),#2002,.F.);
#14942=ADVANCED_FACE('',(#2962),#2003,.F.);
#14943=ADVANCED_FACE('',(#2963),#2004,.F.);
#14944=ADVANCED_FACE('',(#2964),#2005,.F.);
#14945=ADVANCED_FACE('',(#2965),#2006,.F.);
#14946=ADVANCED_FACE('',(#2966),#2007,.F.);
#14947=ADVANCED_FACE('',(#2967),#2008,.F.);
#14948=ADVANCED_FACE('',(#2968),#2009,.F.);
#14949=ADVANCED_FACE('',(#2969),#2010,.F.);
#14950=ADVANCED_FACE('',(#2970),#2011,.F.);
#14951=ADVANCED_FACE('',(#2971),#2012,.F.);
#14952=ADVANCED_FACE('',(#2972),#2013,.F.);
#14953=ADVANCED_FACE('',(#2973),#2014,.F.);
#14954=ADVANCED_FACE('',(#2974),#2015,.F.);
#14955=ADVANCED_FACE('',(#2975),#2016,.F.);
#14956=ADVANCED_FACE('',(#2976),#2017,.F.);
#14957=ADVANCED_FACE('',(#2977),#2018,.F.);
#14958=ADVANCED_FACE('',(#2978),#2019,.F.);
#14959=ADVANCED_FACE('',(#2979),#2020,.F.);
#14960=ADVANCED_FACE('',(#2980),#2021,.F.);
#14961=ADVANCED_FACE('',(#2981),#2022,.F.);
#14962=ADVANCED_FACE('',(#2982),#2023,.F.);
#14963=ADVANCED_FACE('',(#2983),#2024,.F.);
#14964=ADVANCED_FACE('',(#2984),#2025,.F.);
#14965=ADVANCED_FACE('',(#2985),#2026,.F.);
#14966=ADVANCED_FACE('',(#2986),#2027,.F.);
#14967=ADVANCED_FACE('',(#2987),#2028,.F.);
#14968=ADVANCED_FACE('',(#2988),#2029,.F.);
#14969=ADVANCED_FACE('',(#2989),#2030,.F.);
#14970=ADVANCED_FACE('',(#2990),#2031,.F.);
#14971=ADVANCED_FACE('',(#2991),#2032,.F.);
#14972=ADVANCED_FACE('',(#2992),#2033,.F.);
#14973=ADVANCED_FACE('',(#2993),#2034,.F.);
#14974=ADVANCED_FACE('',(#2994),#2035,.F.);
#14975=ADVANCED_FACE('',(#2995),#14524,.T.);
#14976=ADVANCED_FACE('',(#2996),#2036,.F.);
#14977=ADVANCED_FACE('',(#2997),#240,.F.);
#14978=ADVANCED_FACE('',(#2998),#241,.F.);
#14979=ADVANCED_FACE('',(#2999),#2037,.F.);
#14980=ADVANCED_FACE('',(#3000),#14525,.T.);
#14981=ADVANCED_FACE('',(#3001),#2038,.F.);
#14982=ADVANCED_FACE('',(#3002),#242,.F.);
#14983=ADVANCED_FACE('',(#3003),#243,.F.);
#14984=ADVANCED_FACE('',(#3004),#2039,.F.);
#14985=ADVANCED_FACE('',(#3005),#14526,.T.);
#14986=ADVANCED_FACE('',(#3006),#2040,.F.);
#14987=ADVANCED_FACE('',(#3007),#244,.F.);
#14988=ADVANCED_FACE('',(#3008),#245,.F.);
#14989=ADVANCED_FACE('',(#3009),#2041,.F.);
#14990=ADVANCED_FACE('',(#3010),#14527,.T.);
#14991=ADVANCED_FACE('',(#3011),#2042,.F.);
#14992=ADVANCED_FACE('',(#3012),#246,.F.);
#14993=ADVANCED_FACE('',(#3013),#247,.F.);
#14994=ADVANCED_FACE('',(#3014),#2043,.F.);
#14995=ADVANCED_FACE('',(#3015),#14528,.F.);
#14996=ADVANCED_FACE('',(#3016),#14529,.F.);
#14997=ADVANCED_FACE('',(#3017),#14530,.F.);
#14998=ADVANCED_FACE('',(#3018),#14531,.F.);
#14999=ADVANCED_FACE('',(#3019),#14532,.F.);
#15000=ADVANCED_FACE('',(#3020),#2044,.F.);
#15001=ADVANCED_FACE('',(#3021),#248,.F.);
#15002=ADVANCED_FACE('',(#3022),#249,.F.);
#15003=ADVANCED_FACE('',(#3023),#2045,.F.);
#15004=ADVANCED_FACE('',(#3024),#14533,.F.);
#15005=ADVANCED_FACE('',(#3025),#2046,.F.);
#15006=ADVANCED_FACE('',(#3026),#250,.F.);
#15007=ADVANCED_FACE('',(#3027),#251,.F.);
#15008=ADVANCED_FACE('',(#3028),#2047,.F.);
#15009=ADVANCED_FACE('',(#3029),#14534,.F.);
#15010=ADVANCED_FACE('',(#3030),#2048,.F.);
#15011=ADVANCED_FACE('',(#3031),#252,.F.);
#15012=ADVANCED_FACE('',(#3032),#253,.F.);
#15013=ADVANCED_FACE('',(#3033),#2049,.F.);
#15014=ADVANCED_FACE('',(#3034),#14535,.F.);
#15015=ADVANCED_FACE('',(#3035),#2050,.F.);
#15016=ADVANCED_FACE('',(#3036),#254,.F.);
#15017=ADVANCED_FACE('',(#3037),#255,.F.);
#15018=ADVANCED_FACE('',(#3038),#2051,.F.);
#15019=ADVANCED_FACE('',(#3039),#14536,.F.);
#15020=ADVANCED_FACE('',(#3040),#14537,.F.);
#15021=ADVANCED_FACE('',(#3041),#14538,.F.);
#15022=ADVANCED_FACE('',(#3042),#14539,.F.);
#15023=ADVANCED_FACE('',(#3043),#14540,.F.);
#15024=ADVANCED_FACE('',(#3044),#14541,.F.);
#15025=ADVANCED_FACE('',(#3045),#14542,.F.);
#15026=ADVANCED_FACE('',(#3046,#1644,#1645,#1646,#1647,#1648),#14543,.F.);
#15027=ADVANCED_FACE('',(#3047),#2052,.F.);
#15028=ADVANCED_FACE('',(#3048),#256,.F.);
#15029=ADVANCED_FACE('',(#3049),#257,.F.);
#15030=ADVANCED_FACE('',(#3050,#1649),#14544,.T.);
#15031=ADVANCED_FACE('',(#3051),#2053,.F.);
#15032=ADVANCED_FACE('',(#3052),#14545,.T.);
#15033=ADVANCED_FACE('',(#3053),#14546,.T.);
#15034=ADVANCED_FACE('',(#3054),#14547,.T.);
#15035=ADVANCED_FACE('',(#3055,#1650),#14548,.F.);
#15036=ADVANCED_FACE('',(#3056,#1651),#14549,.T.);
#15037=ADVANCED_FACE('',(#3057,#1652),#14550,.F.);
#15038=ADVANCED_FACE('',(#3058),#2054,.F.);
#15039=ADVANCED_FACE('',(#3059),#2055,.F.);
#15040=ADVANCED_FACE('',(#3060,#1653),#14551,.T.);
#15041=ADVANCED_FACE('',(#3061,#1654),#14552,.F.);
#15042=ADVANCED_FACE('',(#3062),#2056,.F.);
#15043=ADVANCED_FACE('',(#3063),#2057,.F.);
#15044=ADVANCED_FACE('',(#3064),#2058,.F.);
#15045=ADVANCED_FACE('',(#3065,#1655),#2059,.T.);
#15046=ADVANCED_FACE('',(#3066,#1656,#1657,#1658,#1659,#1660),#14553,.T.);
#15047=ADVANCED_FACE('',(#3067),#2060,.F.);
#15048=ADVANCED_FACE('',(#3068),#2061,.F.);
#15049=ADVANCED_FACE('',(#3069),#2062,.F.);
#15050=ADVANCED_FACE('',(#3070),#2063,.F.);
#15051=ADVANCED_FACE('',(#3071),#2064,.F.);
#15052=ADVANCED_FACE('',(#3072),#2065,.F.);
#15053=ADVANCED_FACE('',(#3073),#2066,.F.);
#15054=ADVANCED_FACE('',(#3074),#2067,.F.);
#15055=ADVANCED_FACE('',(#3075),#2068,.F.);
#15056=ADVANCED_FACE('',(#3076),#2069,.F.);
#15057=ADVANCED_FACE('',(#3077),#2070,.F.);
#15058=ADVANCED_FACE('',(#3078),#2071,.F.);
#15059=ADVANCED_FACE('',(#3079),#2072,.F.);
#15060=ADVANCED_FACE('',(#3080),#2073,.F.);
#15061=ADVANCED_FACE('',(#3081),#2074,.F.);
#15062=ADVANCED_FACE('',(#3082),#2075,.F.);
#15063=ADVANCED_FACE('',(#3083),#2076,.F.);
#15064=ADVANCED_FACE('',(#3084),#2077,.F.);
#15065=ADVANCED_FACE('',(#3085),#2078,.F.);
#15066=ADVANCED_FACE('',(#3086),#2079,.F.);
#15067=ADVANCED_FACE('',(#3087),#2080,.F.);
#15068=ADVANCED_FACE('',(#3088),#2081,.F.);
#15069=ADVANCED_FACE('',(#3089),#2082,.F.);
#15070=ADVANCED_FACE('',(#3090),#2083,.F.);
#15071=ADVANCED_FACE('',(#3091),#2084,.F.);
#15072=ADVANCED_FACE('',(#3092),#2085,.F.);
#15073=ADVANCED_FACE('',(#3093),#2086,.F.);
#15074=ADVANCED_FACE('',(#3094),#2087,.F.);
#15075=ADVANCED_FACE('',(#3095),#2088,.F.);
#15076=ADVANCED_FACE('',(#3096),#2089,.F.);
#15077=ADVANCED_FACE('',(#3097),#2090,.F.);
#15078=ADVANCED_FACE('',(#3098),#2091,.F.);
#15079=ADVANCED_FACE('',(#3099),#2092,.F.);
#15080=ADVANCED_FACE('',(#3100),#2093,.F.);
#15081=ADVANCED_FACE('',(#3101),#2094,.F.);
#15082=ADVANCED_FACE('',(#3102),#2095,.F.);
#15083=ADVANCED_FACE('',(#3103),#2096,.T.);
#15084=ADVANCED_FACE('',(#3104,#1661),#14554,.F.);
#15085=ADVANCED_FACE('',(#3105,#1662),#14555,.F.);
#15086=ADVANCED_FACE('',(#3106),#2097,.T.);
#15087=ADVANCED_FACE('',(#3107),#14556,.F.);
#15088=ADVANCED_FACE('',(#3108),#14557,.F.);
#15089=ADVANCED_FACE('',(#3109),#14558,.F.);
#15090=ADVANCED_FACE('',(#3110),#14559,.F.);
#15091=ADVANCED_FACE('',(#3111,#1663),#14560,.T.);
#15092=ADVANCED_FACE('',(#3112),#258,.F.);
#15093=ADVANCED_FACE('',(#3113),#2098,.F.);
#15094=ADVANCED_FACE('',(#3114),#259,.F.);
#15095=ADVANCED_FACE('',(#3115),#14561,.F.);
#15096=ADVANCED_FACE('',(#3116),#2099,.F.);
#15097=ADVANCED_FACE('',(#3117),#14562,.F.);
#15098=ADVANCED_FACE('',(#3118),#2100,.F.);
#15099=ADVANCED_FACE('',(#3119),#14563,.F.);
#15100=ADVANCED_FACE('',(#3120),#2101,.T.);
#15101=ADVANCED_FACE('',(#3121),#14564,.T.);
#15102=ADVANCED_FACE('',(#3122,#1664),#14565,.T.);
#15103=ADVANCED_FACE('',(#3123,#1665),#14566,.F.);
#15104=ADVANCED_FACE('',(#3124),#2102,.T.);
#15105=ADVANCED_FACE('',(#3125),#2103,.T.);
#15106=ADVANCED_FACE('',(#3126,#1666),#14567,.T.);
#15107=ADVANCED_FACE('',(#3127,#1667),#2104,.T.);
#15108=ADVANCED_FACE('',(#3128,#1668),#14568,.F.);
#15109=ADVANCED_FACE('',(#3129),#2105,.T.);
#15110=ADVANCED_FACE('',(#3130),#2106,.F.);
#15111=ADVANCED_FACE('',(#3131),#2107,.T.);
#15112=ADVANCED_FACE('',(#3132,#1669),#14569,.T.);
#15113=ADVANCED_FACE('',(#3133,#1670),#14570,.F.);
#15114=ADVANCED_FACE('',(#3134),#2108,.F.);
#15115=ADVANCED_FACE('',(#3135),#2109,.T.);
#15116=ADVANCED_FACE('',(#3136,#1671),#14571,.T.);
#15117=ADVANCED_FACE('',(#3137,#1672),#14572,.F.);
#15118=ADVANCED_FACE('',(#3138),#14573,.F.);
#15119=ADVANCED_FACE('',(#3139),#14574,.F.);
#15120=ADVANCED_FACE('',(#3140),#14575,.F.);
#15121=ADVANCED_FACE('',(#3141),#2110,.F.);
#15122=ADVANCED_FACE('',(#3142),#2111,.T.);
#15123=ADVANCED_FACE('',(#3143),#14576,.T.);
#15124=ADVANCED_FACE('',(#3144),#14577,.T.);
#15125=ADVANCED_FACE('',(#3145),#14578,.T.);
#15126=ADVANCED_FACE('',(#3146),#14579,.T.);
#15127=ADVANCED_FACE('',(#3147),#14580,.T.);
#15128=ADVANCED_FACE('',(#3148),#14581,.T.);
#15129=ADVANCED_FACE('',(#3149),#14582,.F.);
#15130=ADVANCED_FACE('',(#3150),#2112,.T.);
#15131=ADVANCED_FACE('',(#3151),#2113,.T.);
#15132=ADVANCED_FACE('',(#3152),#2114,.T.);
#15133=ADVANCED_FACE('',(#3153),#2115,.T.);
#15134=ADVANCED_FACE('',(#3154),#2116,.T.);
#15135=ADVANCED_FACE('',(#3155),#2117,.T.);
#15136=ADVANCED_FACE('',(#3156),#2118,.T.);
#15137=ADVANCED_FACE('',(#3157),#2119,.T.);
#15138=ADVANCED_FACE('',(#3158),#2120,.T.);
#15139=ADVANCED_FACE('',(#3159),#2121,.T.);
#15140=ADVANCED_FACE('',(#3160),#2122,.T.);
#15141=ADVANCED_FACE('',(#3161),#2123,.T.);
#15142=ADVANCED_FACE('',(#3162),#2124,.T.);
#15143=ADVANCED_FACE('',(#3163),#2125,.T.);
#15144=ADVANCED_FACE('',(#3164),#2126,.T.);
#15145=ADVANCED_FACE('',(#3165),#2127,.T.);
#15146=ADVANCED_FACE('',(#3166),#2128,.T.);
#15147=ADVANCED_FACE('',(#3167),#2129,.T.);
#15148=ADVANCED_FACE('',(#3168),#2130,.T.);
#15149=ADVANCED_FACE('',(#3169),#2131,.T.);
#15150=ADVANCED_FACE('',(#3170),#2132,.T.);
#15151=ADVANCED_FACE('',(#3171),#2133,.T.);
#15152=ADVANCED_FACE('',(#3172),#2134,.T.);
#15153=ADVANCED_FACE('',(#3173),#2135,.T.);
#15154=ADVANCED_FACE('',(#3174),#2136,.T.);
#15155=ADVANCED_FACE('',(#3175),#2137,.T.);
#15156=ADVANCED_FACE('',(#3176),#2138,.T.);
#15157=ADVANCED_FACE('',(#3177),#2139,.T.);
#15158=ADVANCED_FACE('',(#3178),#2140,.T.);
#15159=ADVANCED_FACE('',(#3179),#2141,.T.);
#15160=ADVANCED_FACE('',(#3180),#2142,.T.);
#15161=ADVANCED_FACE('',(#3181),#2143,.T.);
#15162=ADVANCED_FACE('',(#3182),#2144,.T.);
#15163=ADVANCED_FACE('',(#3183),#2145,.T.);
#15164=ADVANCED_FACE('',(#3184),#2146,.T.);
#15165=ADVANCED_FACE('',(#3185),#2147,.T.);
#15166=ADVANCED_FACE('',(#3186),#2148,.T.);
#15167=ADVANCED_FACE('',(#3187),#2149,.T.);
#15168=ADVANCED_FACE('',(#3188),#2150,.T.);
#15169=ADVANCED_FACE('',(#3189),#2151,.T.);
#15170=ADVANCED_FACE('',(#3190),#2152,.T.);
#15171=ADVANCED_FACE('',(#3191),#2153,.T.);
#15172=ADVANCED_FACE('',(#3192),#2154,.T.);
#15173=ADVANCED_FACE('',(#3193),#2155,.T.);
#15174=ADVANCED_FACE('',(#3194),#2156,.T.);
#15175=ADVANCED_FACE('',(#3195),#2157,.T.);
#15176=ADVANCED_FACE('',(#3196),#2158,.T.);
#15177=ADVANCED_FACE('',(#3197),#2159,.T.);
#15178=ADVANCED_FACE('',(#3198),#2160,.T.);
#15179=ADVANCED_FACE('',(#3199),#2161,.T.);
#15180=ADVANCED_FACE('',(#3200),#2162,.T.);
#15181=ADVANCED_FACE('',(#3201),#2163,.T.);
#15182=ADVANCED_FACE('',(#3202),#2164,.T.);
#15183=ADVANCED_FACE('',(#3203),#2165,.T.);
#15184=ADVANCED_FACE('',(#3204),#2166,.T.);
#15185=ADVANCED_FACE('',(#3205),#2167,.T.);
#15186=ADVANCED_FACE('',(#3206),#2168,.T.);
#15187=ADVANCED_FACE('',(#3207),#2169,.T.);
#15188=ADVANCED_FACE('',(#3208),#2170,.T.);
#15189=ADVANCED_FACE('',(#3209),#2171,.T.);
#15190=ADVANCED_FACE('',(#3210),#2172,.T.);
#15191=ADVANCED_FACE('',(#3211),#2173,.T.);
#15192=ADVANCED_FACE('',(#3212),#2174,.T.);
#15193=ADVANCED_FACE('',(#3213),#2175,.T.);
#15194=ADVANCED_FACE('',(#3214),#2176,.T.);
#15195=ADVANCED_FACE('',(#3215),#2177,.T.);
#15196=ADVANCED_FACE('',(#3216),#2178,.T.);
#15197=ADVANCED_FACE('',(#3217),#2179,.T.);
#15198=ADVANCED_FACE('',(#3218),#2180,.T.);
#15199=ADVANCED_FACE('',(#3219),#2181,.T.);
#15200=ADVANCED_FACE('',(#3220),#2182,.T.);
#15201=ADVANCED_FACE('',(#3221),#2183,.T.);
#15202=ADVANCED_FACE('',(#3222),#2184,.T.);
#15203=ADVANCED_FACE('',(#3223),#2185,.T.);
#15204=ADVANCED_FACE('',(#3224),#2186,.T.);
#15205=ADVANCED_FACE('',(#3225),#2187,.T.);
#15206=ADVANCED_FACE('',(#3226),#2188,.T.);
#15207=ADVANCED_FACE('',(#3227),#2189,.T.);
#15208=ADVANCED_FACE('',(#3228),#2190,.T.);
#15209=ADVANCED_FACE('',(#3229),#2191,.T.);
#15210=ADVANCED_FACE('',(#3230),#2192,.T.);
#15211=ADVANCED_FACE('',(#3231),#2193,.T.);
#15212=ADVANCED_FACE('',(#3232),#2194,.T.);
#15213=ADVANCED_FACE('',(#3233),#2195,.T.);
#15214=ADVANCED_FACE('',(#3234),#2196,.T.);
#15215=ADVANCED_FACE('',(#3235),#2197,.T.);
#15216=ADVANCED_FACE('',(#3236),#2198,.T.);
#15217=ADVANCED_FACE('',(#3237),#2199,.T.);
#15218=ADVANCED_FACE('',(#3238),#2200,.T.);
#15219=ADVANCED_FACE('',(#3239),#2201,.T.);
#15220=ADVANCED_FACE('',(#3240),#2202,.T.);
#15221=ADVANCED_FACE('',(#3241),#2203,.T.);
#15222=ADVANCED_FACE('',(#3242),#2204,.T.);
#15223=ADVANCED_FACE('',(#3243),#2205,.T.);
#15224=ADVANCED_FACE('',(#3244),#2206,.T.);
#15225=ADVANCED_FACE('',(#3245),#2207,.T.);
#15226=ADVANCED_FACE('',(#3246),#2208,.T.);
#15227=ADVANCED_FACE('',(#3247),#2209,.T.);
#15228=ADVANCED_FACE('',(#3248),#2210,.T.);
#15229=ADVANCED_FACE('',(#3249),#2211,.T.);
#15230=ADVANCED_FACE('',(#3250),#2212,.T.);
#15231=ADVANCED_FACE('',(#3251),#2213,.T.);
#15232=ADVANCED_FACE('',(#3252),#2214,.T.);
#15233=ADVANCED_FACE('',(#3253),#2215,.T.);
#15234=ADVANCED_FACE('',(#3254),#2216,.T.);
#15235=ADVANCED_FACE('',(#3255),#2217,.T.);
#15236=ADVANCED_FACE('',(#3256),#2218,.T.);
#15237=ADVANCED_FACE('',(#3257),#2219,.T.);
#15238=ADVANCED_FACE('',(#3258),#2220,.T.);
#15239=ADVANCED_FACE('',(#3259),#2221,.T.);
#15240=ADVANCED_FACE('',(#3260),#2222,.T.);
#15241=ADVANCED_FACE('',(#3261),#2223,.T.);
#15242=ADVANCED_FACE('',(#3262),#2224,.T.);
#15243=ADVANCED_FACE('',(#3263),#2225,.T.);
#15244=ADVANCED_FACE('',(#3264),#2226,.T.);
#15245=ADVANCED_FACE('',(#3265),#2227,.T.);
#15246=ADVANCED_FACE('',(#3266),#2228,.T.);
#15247=ADVANCED_FACE('',(#3267),#2229,.T.);
#15248=ADVANCED_FACE('',(#3268),#2230,.T.);
#15249=ADVANCED_FACE('',(#3269),#2231,.T.);
#15250=ADVANCED_FACE('',(#3270),#2232,.T.);
#15251=ADVANCED_FACE('',(#3271),#2233,.T.);
#15252=ADVANCED_FACE('',(#3272),#2234,.T.);
#15253=ADVANCED_FACE('',(#3273),#2235,.T.);
#15254=ADVANCED_FACE('',(#3274),#2236,.T.);
#15255=ADVANCED_FACE('',(#3275),#2237,.T.);
#15256=ADVANCED_FACE('',(#3276),#2238,.T.);
#15257=ADVANCED_FACE('',(#3277),#2239,.T.);
#15258=ADVANCED_FACE('',(#3278),#2240,.T.);
#15259=ADVANCED_FACE('',(#3279),#2241,.T.);
#15260=ADVANCED_FACE('',(#3280),#2242,.T.);
#15261=ADVANCED_FACE('',(#3281),#2243,.T.);
#15262=ADVANCED_FACE('',(#3282),#2244,.T.);
#15263=ADVANCED_FACE('',(#3283),#2245,.T.);
#15264=ADVANCED_FACE('',(#3284),#2246,.T.);
#15265=ADVANCED_FACE('',(#3285),#2247,.T.);
#15266=ADVANCED_FACE('',(#3286),#2248,.T.);
#15267=ADVANCED_FACE('',(#3287),#2249,.T.);
#15268=ADVANCED_FACE('',(#3288),#2250,.T.);
#15269=ADVANCED_FACE('',(#3289),#2251,.T.);
#15270=ADVANCED_FACE('',(#3290),#2252,.T.);
#15271=ADVANCED_FACE('',(#3291),#2253,.T.);
#15272=ADVANCED_FACE('',(#3292),#2254,.T.);
#15273=ADVANCED_FACE('',(#3293),#2255,.T.);
#15274=ADVANCED_FACE('',(#3294),#2256,.T.);
#15275=ADVANCED_FACE('',(#3295),#2257,.T.);
#15276=ADVANCED_FACE('',(#3296),#2258,.T.);
#15277=ADVANCED_FACE('',(#3297),#2259,.T.);
#15278=ADVANCED_FACE('',(#3298),#2260,.T.);
#15279=ADVANCED_FACE('',(#3299),#2261,.T.);
#15280=ADVANCED_FACE('',(#3300),#2262,.T.);
#15281=ADVANCED_FACE('',(#3301),#2263,.T.);
#15282=ADVANCED_FACE('',(#3302),#2264,.T.);
#15283=ADVANCED_FACE('',(#3303),#2265,.T.);
#15284=ADVANCED_FACE('',(#3304),#2266,.T.);
#15285=ADVANCED_FACE('',(#3305),#2267,.T.);
#15286=ADVANCED_FACE('',(#3306),#2268,.T.);
#15287=ADVANCED_FACE('',(#3307),#2269,.T.);
#15288=ADVANCED_FACE('',(#3308),#2270,.T.);
#15289=ADVANCED_FACE('',(#3309),#238,.T.);
#15290=ADVANCED_FACE('',(#3310),#14583,.F.);
#15291=ADVANCED_FACE('',(#3311),#2271,.T.);
#15292=ADVANCED_FACE('',(#3312,#1673),#14584,.F.);
#15293=ADVANCED_FACE('',(#3313,#1674),#14585,.F.);
#15294=ADVANCED_FACE('',(#3314),#2272,.T.);
#15295=ADVANCED_FACE('',(#3315),#14586,.F.);
#15296=ADVANCED_FACE('',(#3316),#260,.F.);
#15297=ADVANCED_FACE('',(#3317),#2273,.T.);
#15298=ADVANCED_FACE('',(#3318),#261,.F.);
#15299=ADVANCED_FACE('',(#3319),#2274,.T.);
#15300=ADVANCED_FACE('',(#3320),#2275,.F.);
#15301=ADVANCED_FACE('',(#3321),#2276,.F.);
#15302=ADVANCED_FACE('',(#3322),#2277,.F.);
#15303=ADVANCED_FACE('',(#3323),#2278,.F.);
#15304=ADVANCED_FACE('',(#3324),#2279,.F.);
#15305=ADVANCED_FACE('',(#3325),#2280,.F.);
#15306=ADVANCED_FACE('',(#3326,#1675,#1676,#1677,#1678,#1679,#1680,#1681),
#14587,.F.);
#15307=ADVANCED_FACE('',(#3327),#2281,.T.);
#15308=ADVANCED_FACE('',(#3328,#1682,#1683,#1684,#1685,#1686,#1687),#14588,
 .T.);
#15309=ADVANCED_FACE('',(#3329,#1688),#14589,.F.);
#15310=ADVANCED_FACE('',(#3330),#2282,.T.);
#15311=ADVANCED_FACE('',(#3331),#2283,.F.);
#15312=ADVANCED_FACE('',(#3332),#2284,.T.);
#15313=ADVANCED_FACE('',(#3333,#1689),#14590,.T.);
#15314=ADVANCED_FACE('',(#3334,#1690),#14591,.F.);
#15315=ADVANCED_FACE('',(#3335),#14592,.F.);
#15316=ADVANCED_FACE('',(#3336),#14593,.F.);
#15317=ADVANCED_FACE('',(#3337),#14594,.F.);
#15318=ADVANCED_FACE('',(#3338),#2285,.F.);
#15319=ADVANCED_FACE('',(#3339),#2286,.T.);
#15320=ADVANCED_FACE('',(#3340),#14595,.T.);
#15321=ADVANCED_FACE('',(#3341),#2287,.T.);
#15322=ADVANCED_FACE('',(#3342),#2288,.T.);
#15323=ADVANCED_FACE('',(#3343),#2289,.T.);
#15324=ADVANCED_FACE('',(#3344),#2290,.T.);
#15325=ADVANCED_FACE('',(#3345),#2291,.T.);
#15326=ADVANCED_FACE('',(#3346),#2292,.T.);
#15327=ADVANCED_FACE('',(#3347),#2293,.T.);
#15328=ADVANCED_FACE('',(#3348),#2294,.T.);
#15329=ADVANCED_FACE('',(#3349),#2295,.T.);
#15330=ADVANCED_FACE('',(#3350),#2296,.T.);
#15331=ADVANCED_FACE('',(#3351),#2297,.T.);
#15332=ADVANCED_FACE('',(#3352),#2298,.T.);
#15333=ADVANCED_FACE('',(#3353),#2299,.T.);
#15334=ADVANCED_FACE('',(#3354),#2300,.T.);
#15335=ADVANCED_FACE('',(#3355),#2301,.T.);
#15336=ADVANCED_FACE('',(#3356),#2302,.T.);
#15337=ADVANCED_FACE('',(#3357),#2303,.T.);
#15338=ADVANCED_FACE('',(#3358),#2304,.T.);
#15339=ADVANCED_FACE('',(#3359),#2305,.T.);
#15340=ADVANCED_FACE('',(#3360),#2306,.T.);
#15341=ADVANCED_FACE('',(#3361),#2307,.T.);
#15342=ADVANCED_FACE('',(#3362),#2308,.T.);
#15343=ADVANCED_FACE('',(#3363),#2309,.T.);
#15344=ADVANCED_FACE('',(#3364),#2310,.T.);
#15345=ADVANCED_FACE('',(#3365),#2311,.T.);
#15346=ADVANCED_FACE('',(#3366),#2312,.T.);
#15347=ADVANCED_FACE('',(#3367),#2313,.T.);
#15348=ADVANCED_FACE('',(#3368),#2314,.T.);
#15349=ADVANCED_FACE('',(#3369),#2315,.T.);
#15350=ADVANCED_FACE('',(#3370),#2316,.T.);
#15351=ADVANCED_FACE('',(#3371),#2317,.T.);
#15352=ADVANCED_FACE('',(#3372),#2318,.T.);
#15353=ADVANCED_FACE('',(#3373),#2319,.T.);
#15354=ADVANCED_FACE('',(#3374),#2320,.T.);
#15355=ADVANCED_FACE('',(#3375),#2321,.T.);
#15356=ADVANCED_FACE('',(#3376),#2322,.T.);
#15357=ADVANCED_FACE('',(#3377),#14596,.F.);
#15358=ADVANCED_FACE('',(#3378),#14597,.F.);
#15359=ADVANCED_FACE('',(#3379),#14598,.F.);
#15360=ADVANCED_FACE('',(#3380),#14599,.F.);
#15361=ADVANCED_FACE('',(#3381),#14600,.F.);
#15362=ADVANCED_FACE('',(#3382),#14601,.F.);
#15363=ADVANCED_FACE('',(#3383),#14602,.F.);
#15364=ADVANCED_FACE('',(#3384),#262,.F.);
#15365=ADVANCED_FACE('',(#3385),#2323,.T.);
#15366=ADVANCED_FACE('',(#3386),#263,.F.);
#15367=ADVANCED_FACE('',(#3387),#14603,.T.);
#15368=ADVANCED_FACE('',(#3388),#2324,.T.);
#15369=ADVANCED_FACE('',(#3389,#1691),#14604,.F.);
#15370=ADVANCED_FACE('',(#3390,#1692),#14605,.F.);
#15371=ADVANCED_FACE('',(#3391),#2325,.F.);
#15372=ADVANCED_FACE('',(#3392),#2326,.F.);
#15373=ADVANCED_FACE('',(#3393,#1693),#14606,.F.);
#15374=ADVANCED_FACE('',(#3394),#2327,.F.);
#15375=ADVANCED_FACE('',(#3395),#2328,.F.);
#15376=ADVANCED_FACE('',(#3396,#1694),#14607,.F.);
#15377=ADVANCED_FACE('',(#3397),#2329,.F.);
#15378=ADVANCED_FACE('',(#3398),#2330,.F.);
#15379=ADVANCED_FACE('',(#3399,#1695),#14608,.F.);
#15380=ADVANCED_FACE('',(#3400),#2331,.F.);
#15381=ADVANCED_FACE('',(#3401),#2332,.F.);
#15382=ADVANCED_FACE('',(#3402),#2333,.F.);
#15383=ADVANCED_FACE('',(#3403),#2334,.T.);
#15384=ADVANCED_FACE('',(#3404,#1696,#1697,#1698,#1699,#1700),#14609,.T.);
#15385=ADVANCED_FACE('',(#3405,#1701,#1702,#1703,#1704,#1705),#14610,.F.);
#15386=ADVANCED_FACE('',(#3406),#236,.F.);
#15387=ADVANCED_FACE('',(#3407),#2335,.T.);
#15388=ADVANCED_FACE('',(#3408),#2336,.F.);
#15389=ADVANCED_FACE('',(#3409),#2337,.T.);
#15390=ADVANCED_FACE('',(#3410,#1706),#14611,.T.);
#15391=ADVANCED_FACE('',(#3411,#1707),#14612,.F.);
#15392=ADVANCED_FACE('',(#3412),#237,.F.);
#15393=ADVANCED_FACE('',(#3413),#2338,.F.);
#15394=ADVANCED_FACE('',(#3414),#2339,.F.);
#15395=ADVANCED_FACE('',(#3415),#2340,.T.);
#15396=ADVANCED_FACE('',(#3416,#1708),#14613,.T.);
#15397=ADVANCED_FACE('',(#3417,#1709),#14614,.F.);
#15398=ADVANCED_FACE('',(#3418),#223,.T.);
#15399=ADVANCED_FACE('',(#3419),#224,.F.);
#15400=ADVANCED_FACE('',(#3420),#2341,.F.);
#15401=ADVANCED_FACE('',(#3421),#14615,.F.);
#15402=ADVANCED_FACE('',(#3422),#225,.F.);
#15403=ADVANCED_FACE('',(#3423),#14616,.F.);
#15404=ADVANCED_FACE('',(#3424),#226,.F.);
#15405=ADVANCED_FACE('',(#3425),#14617,.F.);
#15406=ADVANCED_FACE('',(#3426),#227,.F.);
#15407=ADVANCED_FACE('',(#3427),#14618,.F.);
#15408=ADVANCED_FACE('',(#3428),#228,.F.);
#15409=ADVANCED_FACE('',(#3429),#14619,.F.);
#15410=ADVANCED_FACE('',(#3430),#229,.F.);
#15411=ADVANCED_FACE('',(#3431),#14620,.F.);
#15412=ADVANCED_FACE('',(#3432),#230,.F.);
#15413=ADVANCED_FACE('',(#3433),#14621,.F.);
#15414=ADVANCED_FACE('',(#3434),#231,.F.);
#15415=ADVANCED_FACE('',(#3435),#14622,.F.);
#15416=ADVANCED_FACE('',(#3436),#232,.F.);
#15417=ADVANCED_FACE('',(#3437),#14623,.F.);
#15418=ADVANCED_FACE('',(#3438),#233,.F.);
#15419=ADVANCED_FACE('',(#3439),#14624,.F.);
#15420=ADVANCED_FACE('',(#3440),#234,.F.);
#15421=ADVANCED_FACE('',(#3441),#14625,.F.);
#15422=ADVANCED_FACE('',(#3442),#235,.F.);
#15423=ADVANCED_FACE('',(#3443),#2342,.T.);
#15424=ADVANCED_FACE('',(#3444,#1710),#14626,.T.);
#15425=ADVANCED_FACE('',(#3445),#14627,.F.);
#15426=ADVANCED_FACE('',(#3446),#2343,.F.);
#15427=ADVANCED_FACE('',(#3447),#2344,.T.);
#15428=ADVANCED_FACE('',(#3448,#1711),#14628,.T.);
#15429=ADVANCED_FACE('',(#3449,#1712),#14629,.F.);
#15430=ADVANCED_FACE('',(#3450),#2345,.T.);
#15431=ADVANCED_FACE('',(#3451),#2346,.T.);
#15432=ADVANCED_FACE('',(#3452),#2347,.T.);
#15433=ADVANCED_FACE('',(#3453),#2348,.T.);
#15434=ADVANCED_FACE('',(#3454),#2349,.T.);
#15435=ADVANCED_FACE('',(#3455),#2350,.T.);
#15436=ADVANCED_FACE('',(#3456),#2351,.T.);
#15437=ADVANCED_FACE('',(#3457),#2352,.T.);
#15438=ADVANCED_FACE('',(#3458),#2353,.T.);
#15439=ADVANCED_FACE('',(#3459),#2354,.T.);
#15440=ADVANCED_FACE('',(#3460),#2355,.T.);
#15441=ADVANCED_FACE('',(#3461),#2356,.T.);
#15442=ADVANCED_FACE('',(#3462),#2357,.T.);
#15443=ADVANCED_FACE('',(#3463),#2358,.T.);
#15444=ADVANCED_FACE('',(#3464),#2359,.T.);
#15445=ADVANCED_FACE('',(#3465),#2360,.T.);
#15446=ADVANCED_FACE('',(#3466),#2361,.T.);
#15447=ADVANCED_FACE('',(#3467),#2362,.T.);
#15448=ADVANCED_FACE('',(#3468),#2363,.T.);
#15449=ADVANCED_FACE('',(#3469),#2364,.T.);
#15450=ADVANCED_FACE('',(#3470),#2365,.T.);
#15451=ADVANCED_FACE('',(#3471),#2366,.T.);
#15452=ADVANCED_FACE('',(#3472),#2367,.T.);
#15453=ADVANCED_FACE('',(#3473),#2368,.T.);
#15454=ADVANCED_FACE('',(#3474),#2369,.T.);
#15455=ADVANCED_FACE('',(#3475),#2370,.T.);
#15456=ADVANCED_FACE('',(#3476),#2371,.T.);
#15457=ADVANCED_FACE('',(#3477),#2372,.T.);
#15458=ADVANCED_FACE('',(#3478),#2373,.T.);
#15459=ADVANCED_FACE('',(#3479),#2374,.T.);
#15460=ADVANCED_FACE('',(#3480),#2375,.T.);
#15461=ADVANCED_FACE('',(#3481),#2376,.T.);
#15462=ADVANCED_FACE('',(#3482),#239,.T.);
#15463=ADVANCED_FACE('',(#3483),#264,.F.);
#15464=ADVANCED_FACE('',(#3484),#2377,.T.);
#15465=ADVANCED_FACE('',(#3485),#265,.F.);
#15466=ADVANCED_FACE('',(#3486),#2378,.T.);
#15467=ADVANCED_FACE('',(#3487),#14630,.F.);
#15468=ADVANCED_FACE('',(#3488),#14631,.F.);
#15469=ADVANCED_FACE('',(#3489),#14632,.F.);
#15470=ADVANCED_FACE('',(#3490),#14633,.F.);
#15471=ADVANCED_FACE('',(#3491),#14634,.F.);
#15472=ADVANCED_FACE('',(#3492),#14635,.F.);
#15473=ADVANCED_FACE('',(#3493),#14636,.F.);
#15474=ADVANCED_FACE('',(#3494,#1713),#14637,.T.);
#15475=ADVANCED_FACE('',(#3495),#2379,.T.);
#15476=ADVANCED_FACE('',(#3496,#1714),#14638,.F.);
#15477=ADVANCED_FACE('',(#3497),#14639,.T.);
#15478=CLOSED_SHELL('',(#14640,#14641,#14642,#14643,#14644,#14645,#14646,
#14647,#14648,#14649,#14650,#14651,#14652,#14653,#14654,#14655,#14656,#14657,
#14658,#14659,#14660,#14661,#14662,#14663,#14664));
#15479=CLOSED_SHELL('',(#14665,#14666,#14667,#14668,#14669,#14670,#14671,
#14672,#14673,#14674,#14675,#14676,#14677,#14678,#14679,#14680,#14681,#14682,
#14683,#14684,#14685,#14686,#14687,#14688,#14689,#14690,#14691,#14692,#14693,
#14694,#14695,#14696,#14697,#14698,#14699,#14700,#14701,#14702,#14703,#14704,
#14705,#14706,#14707,#14708,#14709,#14710,#14711,#14712,#14713,#14714,#14715,
#14716,#14717,#14718,#14719,#14720,#14721,#14722,#14723,#14724,#14725,#14726,
#14727,#14728,#14729,#14730,#14731,#14732,#14733,#14734,#14735,#14736,#14737,
#14738,#14739,#14740,#14741,#14742,#14743,#14744,#14745,#14746,#14747,#14748,
#14749,#14750,#14751,#14752,#14753,#14754,#14755,#14756,#14757,#14758,#14759,
#14760,#14761,#14762,#14763,#14764,#14765,#14766,#14767,#14768,#14769,#14770,
#14771,#14772,#14773,#14774,#14775,#14776,#14777,#14778,#14779,#14780,#14781,
#14782,#14783,#14784,#14785,#14786,#14787,#14788,#14789,#14790,#14791,#14792,
#14793,#14794,#14795,#14796,#14797,#14798,#14799,#14800,#14801,#14802,#14803,
#14804,#14805,#14806,#14807,#14808,#14809,#14810,#14811,#14812,#14813,#14814,
#14815,#14816,#14817,#14818,#14819,#14820,#14821,#14822,#14823,#14824,#14825,
#14826,#14827,#14828,#14829,#14830,#14831,#14832,#14833,#14834,#14835,#14836,
#14837,#14838,#14839,#14840,#14841,#14842,#14843,#14844,#14845,#14846,#14847,
#14848,#14849,#14850,#14851,#14852,#14853,#14854,#14855,#14856,#14857,#14858,
#14859,#14860,#14861,#14862,#14863,#14864,#14865,#14866,#14867,#14868,#14869,
#14870,#14871,#14872,#14873,#14874,#14875,#14876,#14877,#14878,#14879,#14880,
#14881,#14882,#14883,#14884,#14885,#14886,#14887,#14888,#14889,#14890,#14891,
#14892,#14893,#14894,#14895,#14896,#14897,#14898,#14899,#14900,#14901,#14902,
#14903,#14904,#14905,#14906,#14907,#14908,#14909,#14910,#14911,#14912,#14913,
#14914,#14915,#14916,#14917,#14918,#14919,#14920,#14921,#14922,#14923,#14924,
#14925,#14926,#14927,#14928,#14929,#14930,#14931,#14932,#14933,#14934,#14935,
#14936,#14937,#14938,#14939,#14940,#14941,#14942,#14943,#14944,#14945,#14946,
#14947,#14948,#14949,#14950,#14951,#14952,#14953,#14954,#14955,#14956,#14957,
#14958,#14959,#14960,#14961,#14962,#14963,#14964,#14965,#14966,#14967,#14968,
#14969,#14970,#14971,#14972,#14973,#14974,#14975,#14976,#14977,#14978,#14979,
#14980,#14981,#14982,#14983,#14984,#14985,#14986,#14987,#14988,#14989,#14990,
#14991,#14992,#14993,#14994,#14995,#14996,#14997,#14998,#14999,#15000,#15001,
#15002,#15003,#15004,#15005,#15006,#15007,#15008,#15009,#15010,#15011,#15012,
#15013,#15014,#15015,#15016,#15017,#15018,#15019,#15020,#15021,#15022,#15023,
#15024,#15025,#15026,#15027,#15028,#15029,#15030,#15031,#15032,#15033,#15034,
#15035,#15036,#15037,#15038,#15039,#15040,#15041,#15042,#15043,#15044,#15045,
#15046));
#15480=CLOSED_SHELL('',(#15047,#15048,#15049,#15050,#15051,#15052,#15053,
#15054,#15055,#15056,#15057,#15058,#15059,#15060,#15061,#15062,#15063,#15064,
#15065,#15066,#15067,#15068,#15069,#15070,#15071,#15072,#15073,#15074,#15075,
#15076,#15077,#15078,#15079,#15080,#15081,#15082,#15083,#15084,#15085,#15086,
#15087,#15088,#15089,#15090,#15091,#15092,#15093,#15094,#15095,#15096,#15097,
#15098,#15099,#15100,#15101,#15102,#15103,#15104,#15105,#15106,#15107,#15108,
#15109));
#15481=CLOSED_SHELL('',(#15110,#15111,#15112,#15113));
#15482=CLOSED_SHELL('',(#15114,#15115,#15116,#15117));
#15483=CLOSED_SHELL('',(#15118,#15119,#15120,#15121,#15122,#15123));
#15484=CLOSED_SHELL('',(#15124,#15125,#15126,#15127,#15128,#15129));
#15485=CLOSED_SHELL('',(#15130,#15131,#15132,#15133,#15134,#15135,#15136,
#15137,#15138,#15139,#15140,#15141,#15142,#15143,#15144,#15145,#15146,#15147,
#15148,#15149,#15150,#15151,#15152,#15153,#15154,#15155,#15156,#15157,#15158,
#15159,#15160,#15161,#15162,#15163,#15164,#15165,#15166,#15167,#15168,#15169,
#15170,#15171,#15172,#15173,#15174,#15175,#15176,#15177,#15178,#15179,#15180,
#15181,#15182,#15183,#15184,#15185,#15186,#15187,#15188,#15189,#15190,#15191,
#15192,#15193,#15194,#15195,#15196,#15197,#15198,#15199,#15200,#15201,#15202,
#15203,#15204,#15205,#15206,#15207,#15208,#15209,#15210,#15211,#15212,#15213,
#15214,#15215,#15216,#15217,#15218,#15219,#15220,#15221,#15222,#15223,#15224,
#15225,#15226,#15227,#15228,#15229,#15230,#15231,#15232,#15233,#15234,#15235,
#15236,#15237,#15238,#15239,#15240,#15241,#15242,#15243,#15244,#15245,#15246,
#15247,#15248,#15249,#15250,#15251,#15252,#15253,#15254,#15255,#15256,#15257,
#15258,#15259,#15260,#15261,#15262,#15263,#15264,#15265,#15266,#15267,#15268,
#15269,#15270,#15271,#15272,#15273,#15274,#15275,#15276,#15277,#15278,#15279,
#15280,#15281,#15282,#15283,#15284,#15285,#15286,#15287,#15288,#15289,#15290,
#15291,#15292,#15293,#15294,#15295,#15296,#15297,#15298,#15299,#15300,#15301,
#15302,#15303,#15304,#15305,#15306,#15307,#15308,#15309,#15310));
#15486=CLOSED_SHELL('',(#15311,#15312,#15313,#15314));
#15487=CLOSED_SHELL('',(#15315,#15316,#15317,#15318,#15319,#15320));
#15488=CLOSED_SHELL('',(#15321,#15322,#15323,#15324,#15325,#15326,#15327,
#15328,#15329,#15330,#15331,#15332,#15333,#15334,#15335,#15336,#15337,#15338,
#15339,#15340,#15341,#15342,#15343,#15344,#15345,#15346,#15347,#15348,#15349,
#15350,#15351,#15352,#15353,#15354,#15355,#15356,#15357,#15358,#15359,#15360,
#15361,#15362,#15363,#15364,#15365,#15366,#15367,#15368,#15369));
#15489=CLOSED_SHELL('',(#15370,#15371,#15372,#15373,#15374,#15375,#15376,
#15377,#15378,#15379,#15380,#15381,#15382,#15383,#15384,#15385));
#15490=CLOSED_SHELL('',(#15386,#15387,#15388,#15389,#15390,#15391));
#15491=CLOSED_SHELL('',(#15392,#15393,#15394,#15395,#15396,#15397));
#15492=CLOSED_SHELL('',(#15398));
#15493=CLOSED_SHELL('',(#15399,#15400,#15401,#15402,#15403,#15404,#15405,
#15406,#15407,#15408,#15409,#15410,#15411,#15412,#15413,#15414,#15415,#15416,
#15417,#15418,#15419,#15420,#15421,#15422,#15423,#15424,#15425));
#15494=CLOSED_SHELL('',(#15426,#15427,#15428,#15429));
#15495=CLOSED_SHELL('',(#15430,#15431,#15432,#15433,#15434,#15435,#15436,
#15437,#15438,#15439,#15440,#15441,#15442,#15443,#15444,#15445,#15446,#15447,
#15448,#15449,#15450,#15451,#15452,#15453,#15454,#15455,#15456,#15457,#15458,
#15459,#15460,#15461,#15462,#15463,#15464,#15465,#15466,#15467,#15468,#15469,
#15470,#15471,#15472,#15473,#15474,#15475,#15476,#15477));
#15496=DERIVED_UNIT_ELEMENT(#15532,1.);
#15497=DERIVED_UNIT_ELEMENT(#63900,-3.);
#15498=DERIVED_UNIT_ELEMENT(#15532,1.);
#15499=DERIVED_UNIT_ELEMENT(#63900,-3.);
#15500=DERIVED_UNIT_ELEMENT(#15532,1.);
#15501=DERIVED_UNIT_ELEMENT(#63900,-3.);
#15502=DERIVED_UNIT_ELEMENT(#15532,1.);
#15503=DERIVED_UNIT_ELEMENT(#63900,-3.);
#15504=DERIVED_UNIT_ELEMENT(#15532,1.);
#15505=DERIVED_UNIT_ELEMENT(#63900,-3.);
#15506=DERIVED_UNIT_ELEMENT(#15532,1.);
#15507=DERIVED_UNIT_ELEMENT(#63900,-3.);
#15508=DERIVED_UNIT_ELEMENT(#15532,1.);
#15509=DERIVED_UNIT_ELEMENT(#63900,-3.);
#15510=DERIVED_UNIT_ELEMENT(#15532,1.);
#15511=DERIVED_UNIT_ELEMENT(#63900,-3.);
#15512=DERIVED_UNIT_ELEMENT(#15532,1.);
#15513=DERIVED_UNIT_ELEMENT(#63900,-3.);
#15514=DERIVED_UNIT_ELEMENT(#15532,1.);
#15515=DERIVED_UNIT_ELEMENT(#63900,-3.);
#15516=DERIVED_UNIT_ELEMENT(#15532,1.);
#15517=DERIVED_UNIT_ELEMENT(#63900,-3.);
#15518=DERIVED_UNIT_ELEMENT(#15532,1.);
#15519=DERIVED_UNIT_ELEMENT(#63900,-3.);
#15520=DERIVED_UNIT_ELEMENT(#15532,1.);
#15521=DERIVED_UNIT_ELEMENT(#63900,-3.);
#15522=DERIVED_UNIT_ELEMENT(#15532,1.);
#15523=DERIVED_UNIT_ELEMENT(#63900,-3.);
#15524=DERIVED_UNIT_ELEMENT(#15532,1.);
#15525=DERIVED_UNIT_ELEMENT(#63900,-3.);
#15526=DERIVED_UNIT_ELEMENT(#15532,1.);
#15527=DERIVED_UNIT_ELEMENT(#63900,-3.);
#15528=DERIVED_UNIT_ELEMENT(#15532,1.);
#15529=DERIVED_UNIT_ELEMENT(#63900,-3.);
#15530=DERIVED_UNIT_ELEMENT(#15532,1.);
#15531=DERIVED_UNIT_ELEMENT(#63900,-3.);
#15532=(
MASS_UNIT()
NAMED_UNIT(*)
SI_UNIT(.KILO.,.GRAM.)
);
#15533=DERIVED_UNIT((#15496,#15497));
#15534=DERIVED_UNIT((#15498,#15499));
#15535=DERIVED_UNIT((#15500,#15501));
#15536=DERIVED_UNIT((#15502,#15503));
#15537=DERIVED_UNIT((#15504,#15505));
#15538=DERIVED_UNIT((#15506,#15507));
#15539=DERIVED_UNIT((#15508,#15509));
#15540=DERIVED_UNIT((#15510,#15511));
#15541=DERIVED_UNIT((#15512,#15513));
#15542=DERIVED_UNIT((#15514,#15515));
#15543=DERIVED_UNIT((#15516,#15517));
#15544=DERIVED_UNIT((#15518,#15519));
#15545=DERIVED_UNIT((#15520,#15521));
#15546=DERIVED_UNIT((#15522,#15523));
#15547=DERIVED_UNIT((#15524,#15525));
#15548=DERIVED_UNIT((#15526,#15527));
#15549=DERIVED_UNIT((#15528,#15529));
#15550=DERIVED_UNIT((#15530,#15531));
#15551=MEASURE_REPRESENTATION_ITEM('density measure',
POSITIVE_RATIO_MEASURE(7850.),#15533);
#15552=MEASURE_REPRESENTATION_ITEM('density measure',
POSITIVE_RATIO_MEASURE(7850.),#15534);
#15553=MEASURE_REPRESENTATION_ITEM('density measure',
POSITIVE_RATIO_MEASURE(7850.),#15535);
#15554=MEASURE_REPRESENTATION_ITEM('density measure',
POSITIVE_RATIO_MEASURE(7850.),#15536);
#15555=MEASURE_REPRESENTATION_ITEM('density measure',
POSITIVE_RATIO_MEASURE(7850.),#15537);
#15556=MEASURE_REPRESENTATION_ITEM('density measure',
POSITIVE_RATIO_MEASURE(7850.),#15538);
#15557=MEASURE_REPRESENTATION_ITEM('density measure',
POSITIVE_RATIO_MEASURE(7850.),#15539);
#15558=MEASURE_REPRESENTATION_ITEM('density measure',
POSITIVE_RATIO_MEASURE(7850.),#15540);
#15559=MEASURE_REPRESENTATION_ITEM('density measure',
POSITIVE_RATIO_MEASURE(8920.),#15541);
#15560=MEASURE_REPRESENTATION_ITEM('density measure',
POSITIVE_RATIO_MEASURE(7850.),#15542);
#15561=MEASURE_REPRESENTATION_ITEM('density measure',
POSITIVE_RATIO_MEASURE(7850.),#15543);
#15562=MEASURE_REPRESENTATION_ITEM('density measure',
POSITIVE_RATIO_MEASURE(7850.),#15544);
#15563=MEASURE_REPRESENTATION_ITEM('density measure',
POSITIVE_RATIO_MEASURE(7850.),#15545);
#15564=MEASURE_REPRESENTATION_ITEM('density measure',
POSITIVE_RATIO_MEASURE(7850.),#15546);
#15565=MEASURE_REPRESENTATION_ITEM('density measure',
POSITIVE_RATIO_MEASURE(7850.),#15547);
#15566=MEASURE_REPRESENTATION_ITEM('density measure',
POSITIVE_RATIO_MEASURE(1130.),#15548);
#15567=MEASURE_REPRESENTATION_ITEM('density measure',
POSITIVE_RATIO_MEASURE(8920.),#15549);
#15568=MEASURE_REPRESENTATION_ITEM('density measure',
POSITIVE_RATIO_MEASURE(7850.),#15550);
#15569=PROPERTY_DEFINITION_REPRESENTATION(#15659,#15605);
#15570=PROPERTY_DEFINITION_REPRESENTATION(#15660,#15606);
#15571=PROPERTY_DEFINITION_REPRESENTATION(#15661,#15607);
#15572=PROPERTY_DEFINITION_REPRESENTATION(#15662,#15608);
#15573=PROPERTY_DEFINITION_REPRESENTATION(#15663,#15609);
#15574=PROPERTY_DEFINITION_REPRESENTATION(#15664,#15610);
#15575=PROPERTY_DEFINITION_REPRESENTATION(#15665,#15611);
#15576=PROPERTY_DEFINITION_REPRESENTATION(#15666,#15612);
#15577=PROPERTY_DEFINITION_REPRESENTATION(#15667,#15613);
#15578=PROPERTY_DEFINITION_REPRESENTATION(#15668,#15614);
#15579=PROPERTY_DEFINITION_REPRESENTATION(#15669,#15615);
#15580=PROPERTY_DEFINITION_REPRESENTATION(#15670,#15616);
#15581=PROPERTY_DEFINITION_REPRESENTATION(#15671,#15617);
#15582=PROPERTY_DEFINITION_REPRESENTATION(#15672,#15618);
#15583=PROPERTY_DEFINITION_REPRESENTATION(#15673,#15619);
#15584=PROPERTY_DEFINITION_REPRESENTATION(#15674,#15620);
#15585=PROPERTY_DEFINITION_REPRESENTATION(#15675,#15621);
#15586=PROPERTY_DEFINITION_REPRESENTATION(#15676,#15622);
#15587=PROPERTY_DEFINITION_REPRESENTATION(#15677,#15623);
#15588=PROPERTY_DEFINITION_REPRESENTATION(#15678,#15624);
#15589=PROPERTY_DEFINITION_REPRESENTATION(#15679,#15625);
#15590=PROPERTY_DEFINITION_REPRESENTATION(#15680,#15626);
#15591=PROPERTY_DEFINITION_REPRESENTATION(#15681,#15627);
#15592=PROPERTY_DEFINITION_REPRESENTATION(#15682,#15628);
#15593=PROPERTY_DEFINITION_REPRESENTATION(#15683,#15629);
#15594=PROPERTY_DEFINITION_REPRESENTATION(#15684,#15630);
#15595=PROPERTY_DEFINITION_REPRESENTATION(#15685,#15631);
#15596=PROPERTY_DEFINITION_REPRESENTATION(#15686,#15632);
#15597=PROPERTY_DEFINITION_REPRESENTATION(#15687,#15633);
#15598=PROPERTY_DEFINITION_REPRESENTATION(#15688,#15634);
#15599=PROPERTY_DEFINITION_REPRESENTATION(#15689,#15635);
#15600=PROPERTY_DEFINITION_REPRESENTATION(#15690,#15636);
#15601=PROPERTY_DEFINITION_REPRESENTATION(#15691,#15637);
#15602=PROPERTY_DEFINITION_REPRESENTATION(#15692,#15638);
#15603=PROPERTY_DEFINITION_REPRESENTATION(#15693,#15639);
#15604=PROPERTY_DEFINITION_REPRESENTATION(#15694,#15640);
#15605=REPRESENTATION('material name',(#15641),#63880);
#15606=REPRESENTATION('density',(#15551),#63880);
#15607=REPRESENTATION('material name',(#15642),#63881);
#15608=REPRESENTATION('density',(#15552),#63881);
#15609=REPRESENTATION('material name',(#15643),#63882);
#15610=REPRESENTATION('density',(#15553),#63882);
#15611=REPRESENTATION('material name',(#15644),#63883);
#15612=REPRESENTATION('density',(#15554),#63883);
#15613=REPRESENTATION('material name',(#15645),#63884);
#15614=REPRESENTATION('density',(#15555),#63884);
#15615=REPRESENTATION('material name',(#15646),#63885);
#15616=REPRESENTATION('density',(#15556),#63885);
#15617=REPRESENTATION('material name',(#15647),#63886);
#15618=REPRESENTATION('density',(#15557),#63886);
#15619=REPRESENTATION('material name',(#15648),#63887);
#15620=REPRESENTATION('density',(#15558),#63887);
#15621=REPRESENTATION('material name',(#15649),#63888);
#15622=REPRESENTATION('density',(#15559),#63888);
#15623=REPRESENTATION('material name',(#15650),#63889);
#15624=REPRESENTATION('density',(#15560),#63889);
#15625=REPRESENTATION('material name',(#15651),#63890);
#15626=REPRESENTATION('density',(#15561),#63890);
#15627=REPRESENTATION('material name',(#15652),#63891);
#15628=REPRESENTATION('density',(#15562),#63891);
#15629=REPRESENTATION('material name',(#15653),#63892);
#15630=REPRESENTATION('density',(#15563),#63892);
#15631=REPRESENTATION('material name',(#15654),#63893);
#15632=REPRESENTATION('density',(#15564),#63893);
#15633=REPRESENTATION('material name',(#15655),#63894);
#15634=REPRESENTATION('density',(#15565),#63894);
#15635=REPRESENTATION('material name',(#15656),#63895);
#15636=REPRESENTATION('density',(#15566),#63895);
#15637=REPRESENTATION('material name',(#15657),#63896);
#15638=REPRESENTATION('density',(#15567),#63896);
#15639=REPRESENTATION('material name',(#15658),#63897);
#15640=REPRESENTATION('density',(#15568),#63897);
#15641=DESCRIPTIVE_REPRESENTATION_ITEM('Steel','Steel');
#15642=DESCRIPTIVE_REPRESENTATION_ITEM('Steel','Steel');
#15643=DESCRIPTIVE_REPRESENTATION_ITEM('Steel','Steel');
#15644=DESCRIPTIVE_REPRESENTATION_ITEM('Steel','Steel');
#15645=DESCRIPTIVE_REPRESENTATION_ITEM('Steel','Steel');
#15646=DESCRIPTIVE_REPRESENTATION_ITEM('Steel','Steel');
#15647=DESCRIPTIVE_REPRESENTATION_ITEM('Steel','Steel');
#15648=DESCRIPTIVE_REPRESENTATION_ITEM('Steel','Steel');
#15649=DESCRIPTIVE_REPRESENTATION_ITEM('Copper, Alloy','Copper, Alloy');
#15650=DESCRIPTIVE_REPRESENTATION_ITEM('Steel','Steel');
#15651=DESCRIPTIVE_REPRESENTATION_ITEM('Steel','Steel');
#15652=DESCRIPTIVE_REPRESENTATION_ITEM('Steel','Steel');
#15653=DESCRIPTIVE_REPRESENTATION_ITEM('Steel','Steel');
#15654=DESCRIPTIVE_REPRESENTATION_ITEM('Steel','Steel');
#15655=DESCRIPTIVE_REPRESENTATION_ITEM('Steel','Steel');
#15656=DESCRIPTIVE_REPRESENTATION_ITEM('Nylon 6/6','Nylon 6/6');
#15657=DESCRIPTIVE_REPRESENTATION_ITEM('Copper, Alloy','Copper, Alloy');
#15658=DESCRIPTIVE_REPRESENTATION_ITEM('Steel','Steel');
#15659=PROPERTY_DEFINITION('material property','material name',#64015);
#15660=PROPERTY_DEFINITION('material property','density of part',#64015);
#15661=PROPERTY_DEFINITION('material property','material name',#64016);
#15662=PROPERTY_DEFINITION('material property','density of part',#64016);
#15663=PROPERTY_DEFINITION('material property','material name',#64017);
#15664=PROPERTY_DEFINITION('material property','density of part',#64017);
#15665=PROPERTY_DEFINITION('material property','material name',#64018);
#15666=PROPERTY_DEFINITION('material property','density of part',#64018);
#15667=PROPERTY_DEFINITION('material property','material name',#64019);
#15668=PROPERTY_DEFINITION('material property','density of part',#64019);
#15669=PROPERTY_DEFINITION('material property','material name',#64020);
#15670=PROPERTY_DEFINITION('material property','density of part',#64020);
#15671=PROPERTY_DEFINITION('material property','material name',#64021);
#15672=PROPERTY_DEFINITION('material property','density of part',#64021);
#15673=PROPERTY_DEFINITION('material property','material name',#64022);
#15674=PROPERTY_DEFINITION('material property','density of part',#64022);
#15675=PROPERTY_DEFINITION('material property','material name',#64023);
#15676=PROPERTY_DEFINITION('material property','density of part',#64023);
#15677=PROPERTY_DEFINITION('material property','material name',#64024);
#15678=PROPERTY_DEFINITION('material property','density of part',#64024);
#15679=PROPERTY_DEFINITION('material property','material name',#64025);
#15680=PROPERTY_DEFINITION('material property','density of part',#64025);
#15681=PROPERTY_DEFINITION('material property','material name',#64026);
#15682=PROPERTY_DEFINITION('material property','density of part',#64026);
#15683=PROPERTY_DEFINITION('material property','material name',#64027);
#15684=PROPERTY_DEFINITION('material property','density of part',#64027);
#15685=PROPERTY_DEFINITION('material property','material name',#64028);
#15686=PROPERTY_DEFINITION('material property','density of part',#64028);
#15687=PROPERTY_DEFINITION('material property','material name',#64029);
#15688=PROPERTY_DEFINITION('material property','density of part',#64029);
#15689=PROPERTY_DEFINITION('material property','material name',#64030);
#15690=PROPERTY_DEFINITION('material property','density of part',#64030);
#15691=PROPERTY_DEFINITION('material property','material name',#64031);
#15692=PROPERTY_DEFINITION('material property','density of part',#64031);
#15693=PROPERTY_DEFINITION('material property','material name',#64032);
#15694=PROPERTY_DEFINITION('material property','density of part',#64032);
#15695=AXIS2_PLACEMENT_3D('',#19950,#16859,#16860);
#15696=AXIS2_PLACEMENT_3D('',#19951,#16861,#16862);
#15697=AXIS2_PLACEMENT_3D('',#19952,#16863,#16864);
#15698=AXIS2_PLACEMENT_3D('',#19961,#16869,#16870);
#15699=AXIS2_PLACEMENT_3D('',#19963,#16871,#16872);
#15700=AXIS2_PLACEMENT_3D('',#19968,#16875,#16876);
#15701=AXIS2_PLACEMENT_3D('',#19969,#16877,#16878);
#15702=AXIS2_PLACEMENT_3D('',#19975,#16882,#16883);
#15703=AXIS2_PLACEMENT_3D('',#19977,#16885,#16886);
#15704=AXIS2_PLACEMENT_3D('',#19979,#16887,#16888);
#15705=AXIS2_PLACEMENT_3D('',#19980,#16889,#16890);
#15706=AXIS2_PLACEMENT_3D('',#19981,#16891,#16892);
#15707=AXIS2_PLACEMENT_3D('',#19984,#16893,#16894);
#15708=AXIS2_PLACEMENT_3D('',#19985,#16895,#16896);
#15709=AXIS2_PLACEMENT_3D('',#19986,#16897,#16898);
#15710=AXIS2_PLACEMENT_3D('',#19990,#16900,#16901);
#15711=AXIS2_PLACEMENT_3D('',#19992,#16903,#16904);
#15712=AXIS2_PLACEMENT_3D('',#19994,#16905,#16906);
#15713=AXIS2_PLACEMENT_3D('',#19998,#16908,#16909);
#15714=AXIS2_PLACEMENT_3D('',#20001,#16911,#16912);
#15715=AXIS2_PLACEMENT_3D('',#20003,#16913,#16914);
#15716=AXIS2_PLACEMENT_3D('',#20006,#16916,#16917);
#15717=AXIS2_PLACEMENT_3D('',#20007,#16918,#16919);
#15718=AXIS2_PLACEMENT_3D('',#20009,#16920,#16921);
#15719=AXIS2_PLACEMENT_3D('',#20012,#16923,#16924);
#15720=AXIS2_PLACEMENT_3D('',#20013,#16925,#16926);
#15721=AXIS2_PLACEMENT_3D('',#20015,#16927,#16928);
#15722=AXIS2_PLACEMENT_3D('',#20018,#16930,#16931);
#15723=AXIS2_PLACEMENT_3D('',#20019,#16932,#16933);
#15724=AXIS2_PLACEMENT_3D('',#20021,#16934,#16935);
#15725=AXIS2_PLACEMENT_3D('',#20024,#16937,#16938);
#15726=AXIS2_PLACEMENT_3D('',#20025,#16939,#16940);
#15727=AXIS2_PLACEMENT_3D('',#20027,#16941,#16942);
#15728=AXIS2_PLACEMENT_3D('',#20030,#16944,#16945);
#15729=AXIS2_PLACEMENT_3D('',#20031,#16946,#16947);
#15730=AXIS2_PLACEMENT_3D('',#20033,#16948,#16949);
#15731=AXIS2_PLACEMENT_3D('',#20036,#16951,#16952);
#15732=AXIS2_PLACEMENT_3D('',#20037,#16953,#16954);
#15733=AXIS2_PLACEMENT_3D('',#20039,#16955,#16956);
#15734=AXIS2_PLACEMENT_3D('',#20042,#16958,#16959);
#15735=AXIS2_PLACEMENT_3D('',#20043,#16960,#16961);
#15736=AXIS2_PLACEMENT_3D('',#20049,#16965,#16966);
#15737=AXIS2_PLACEMENT_3D('',#20055,#16970,#16971);
#15738=AXIS2_PLACEMENT_3D('',#20058,#16974,#16975);
#15739=AXIS2_PLACEMENT_3D('',#20059,#16976,#16977);
#15740=AXIS2_PLACEMENT_3D('',#20061,#16978,#16979);
#15741=AXIS2_PLACEMENT_3D('',#20062,#16980,#16981);
#15742=AXIS2_PLACEMENT_3D('',#20064,#16982,#16983);
#15743=AXIS2_PLACEMENT_3D('',#20066,#16984,#16985);
#15744=AXIS2_PLACEMENT_3D('',#20067,#16986,#16987);
#15745=AXIS2_PLACEMENT_3D('',#20069,#16989,#16990);
#15746=AXIS2_PLACEMENT_3D('',#20072,#16992,#16993);
#15747=AXIS2_PLACEMENT_3D('',#20073,#16994,#16995);
#15748=AXIS2_PLACEMENT_3D('',#20075,#16996,#16997);
#15749=AXIS2_PLACEMENT_3D('',#20079,#17000,#17001);
#15750=AXIS2_PLACEMENT_3D('',#20080,#17002,#17003);
#15751=AXIS2_PLACEMENT_3D('',#20081,#17004,#17005);
#15752=AXIS2_PLACEMENT_3D('',#20082,#17006,#17007);
#15753=AXIS2_PLACEMENT_3D('',#20083,#17008,#17009);
#15754=AXIS2_PLACEMENT_3D('',#20088,#17011,#17012);
#15755=AXIS2_PLACEMENT_3D('',#20102,#17013,#17014);
#15756=AXIS2_PLACEMENT_3D('',#20147,#17016,#17017);
#15757=AXIS2_PLACEMENT_3D('',#20191,#17018,#17019);
#15758=AXIS2_PLACEMENT_3D('',#20278,#17021,#17022);
#15759=AXIS2_PLACEMENT_3D('',#20368,#17024,#17025);
#15760=AXIS2_PLACEMENT_3D('',#20455,#17027,#17028);
#15761=AXIS2_PLACEMENT_3D('',#20545,#17030,#17031);
#15762=AXIS2_PLACEMENT_3D('',#20576,#17033,#17034);
#15763=AXIS2_PLACEMENT_3D('',#20614,#17035,#17036);
#15764=AXIS2_PLACEMENT_3D('',#20631,#17038,#17039);
#15765=AXIS2_PLACEMENT_3D('',#20644,#17040,#17041);
#15766=AXIS2_PLACEMENT_3D('',#20682,#17043,#17044);
#15767=AXIS2_PLACEMENT_3D('',#20719,#17046,#17047);
#15768=AXIS2_PLACEMENT_3D('',#20756,#17049,#17050);
#15769=AXIS2_PLACEMENT_3D('',#20794,#17052,#17053);
#15770=AXIS2_PLACEMENT_3D('',#20832,#17055,#17056);
#15771=AXIS2_PLACEMENT_3D('',#20844,#17058,#17059);
#15772=AXIS2_PLACEMENT_3D('',#20852,#17060,#17061);
#15773=AXIS2_PLACEMENT_3D('',#20874,#17063,#17064);
#15774=AXIS2_PLACEMENT_3D('',#20877,#17066,#17067);
#15775=AXIS2_PLACEMENT_3D('',#20879,#17068,#17069);
#15776=AXIS2_PLACEMENT_3D('',#20902,#17070,#17071);
#15777=AXIS2_PLACEMENT_3D('',#20950,#17073,#17074);
#15778=AXIS2_PLACEMENT_3D('',#20998,#17076,#17077);
#15779=AXIS2_PLACEMENT_3D('',#21049,#17079,#17080);
#15780=AXIS2_PLACEMENT_3D('',#21100,#17082,#17083);
#15781=AXIS2_PLACEMENT_3D('',#21148,#17085,#17086);
#15782=AXIS2_PLACEMENT_3D('',#21199,#17088,#17089);
#15783=AXIS2_PLACEMENT_3D('',#21250,#17091,#17092);
#15784=AXIS2_PLACEMENT_3D('',#21298,#17094,#17095);
#15785=AXIS2_PLACEMENT_3D('',#21346,#17097,#17098);
#15786=AXIS2_PLACEMENT_3D('',#21400,#17100,#17101);
#15787=AXIS2_PLACEMENT_3D('',#21448,#17103,#17104);
#15788=AXIS2_PLACEMENT_3D('',#21496,#17106,#17107);
#15789=AXIS2_PLACEMENT_3D('',#21547,#17109,#17110);
#15790=AXIS2_PLACEMENT_3D('',#21598,#17112,#17113);
#15791=AXIS2_PLACEMENT_3D('',#21646,#17115,#17116);
#15792=AXIS2_PLACEMENT_3D('',#21697,#17118,#17119);
#15793=AXIS2_PLACEMENT_3D('',#21716,#17121,#17122);
#15794=AXIS2_PLACEMENT_3D('',#21736,#17123,#17124);
#15795=AXIS2_PLACEMENT_3D('',#21747,#17126,#17127);
#15796=AXIS2_PLACEMENT_3D('',#21754,#17128,#17129);
#15797=AXIS2_PLACEMENT_3D('',#21779,#17131,#17132);
#15798=AXIS2_PLACEMENT_3D('',#21803,#17134,#17135);
#15799=AXIS2_PLACEMENT_3D('',#21828,#17137,#17138);
#15800=AXIS2_PLACEMENT_3D('',#21852,#17140,#17141);
#15801=AXIS2_PLACEMENT_3D('',#21877,#17143,#17144);
#15802=AXIS2_PLACEMENT_3D('',#21902,#17146,#17147);
#15803=AXIS2_PLACEMENT_3D('',#21926,#17149,#17150);
#15804=AXIS2_PLACEMENT_3D('',#21951,#17152,#17153);
#15805=AXIS2_PLACEMENT_3D('',#21975,#17155,#17156);
#15806=AXIS2_PLACEMENT_3D('',#22000,#17158,#17159);
#15807=AXIS2_PLACEMENT_3D('',#22025,#17161,#17162);
#15808=AXIS2_PLACEMENT_3D('',#22049,#17164,#17165);
#15809=AXIS2_PLACEMENT_3D('',#22074,#17167,#17168);
#15810=AXIS2_PLACEMENT_3D('',#22098,#17170,#17171);
#15811=AXIS2_PLACEMENT_3D('',#22123,#17173,#17174);
#15812=AXIS2_PLACEMENT_3D('',#22148,#17176,#17177);
#15813=AXIS2_PLACEMENT_3D('',#22172,#17179,#17180);
#15814=AXIS2_PLACEMENT_3D('',#22183,#17182,#17183);
#15815=AXIS2_PLACEMENT_3D('',#22189,#17184,#17185);
#15816=AXIS2_PLACEMENT_3D('',#22211,#17187,#17188);
#15817=AXIS2_PLACEMENT_3D('',#22214,#17190,#17191);
#15818=AXIS2_PLACEMENT_3D('',#22216,#17192,#17193);
#15819=AXIS2_PLACEMENT_3D('',#22239,#17194,#17195);
#15820=AXIS2_PLACEMENT_3D('',#22287,#17197,#17198);
#15821=AXIS2_PLACEMENT_3D('',#22335,#17200,#17201);
#15822=AXIS2_PLACEMENT_3D('',#22386,#17203,#17204);
#15823=AXIS2_PLACEMENT_3D('',#22437,#17206,#17207);
#15824=AXIS2_PLACEMENT_3D('',#22485,#17209,#17210);
#15825=AXIS2_PLACEMENT_3D('',#22536,#17212,#17213);
#15826=AXIS2_PLACEMENT_3D('',#22587,#17215,#17216);
#15827=AXIS2_PLACEMENT_3D('',#22635,#17218,#17219);
#15828=AXIS2_PLACEMENT_3D('',#22683,#17221,#17222);
#15829=AXIS2_PLACEMENT_3D('',#22737,#17224,#17225);
#15830=AXIS2_PLACEMENT_3D('',#22785,#17227,#17228);
#15831=AXIS2_PLACEMENT_3D('',#22833,#17230,#17231);
#15832=AXIS2_PLACEMENT_3D('',#22884,#17233,#17234);
#15833=AXIS2_PLACEMENT_3D('',#22935,#17236,#17237);
#15834=AXIS2_PLACEMENT_3D('',#22983,#17239,#17240);
#15835=AXIS2_PLACEMENT_3D('',#23034,#17242,#17243);
#15836=AXIS2_PLACEMENT_3D('',#23053,#17245,#17246);
#15837=AXIS2_PLACEMENT_3D('',#23073,#17247,#17248);
#15838=AXIS2_PLACEMENT_3D('',#23084,#17250,#17251);
#15839=AXIS2_PLACEMENT_3D('',#23091,#17252,#17253);
#15840=AXIS2_PLACEMENT_3D('',#23116,#17255,#17256);
#15841=AXIS2_PLACEMENT_3D('',#23140,#17258,#17259);
#15842=AXIS2_PLACEMENT_3D('',#23165,#17261,#17262);
#15843=AXIS2_PLACEMENT_3D('',#23189,#17264,#17265);
#15844=AXIS2_PLACEMENT_3D('',#23214,#17267,#17268);
#15845=AXIS2_PLACEMENT_3D('',#23239,#17270,#17271);
#15846=AXIS2_PLACEMENT_3D('',#23263,#17273,#17274);
#15847=AXIS2_PLACEMENT_3D('',#23288,#17276,#17277);
#15848=AXIS2_PLACEMENT_3D('',#23312,#17279,#17280);
#15849=AXIS2_PLACEMENT_3D('',#23337,#17282,#17283);
#15850=AXIS2_PLACEMENT_3D('',#23362,#17285,#17286);
#15851=AXIS2_PLACEMENT_3D('',#23386,#17288,#17289);
#15852=AXIS2_PLACEMENT_3D('',#23411,#17291,#17292);
#15853=AXIS2_PLACEMENT_3D('',#23435,#17294,#17295);
#15854=AXIS2_PLACEMENT_3D('',#23460,#17297,#17298);
#15855=AXIS2_PLACEMENT_3D('',#23485,#17300,#17301);
#15856=AXIS2_PLACEMENT_3D('',#23509,#17303,#17304);
#15857=AXIS2_PLACEMENT_3D('',#23520,#17306,#17307);
#15858=AXIS2_PLACEMENT_3D('',#23526,#17308,#17309);
#15859=AXIS2_PLACEMENT_3D('',#23548,#17311,#17312);
#15860=AXIS2_PLACEMENT_3D('',#23551,#17314,#17315);
#15861=AXIS2_PLACEMENT_3D('',#23553,#17316,#17317);
#15862=AXIS2_PLACEMENT_3D('',#23576,#17318,#17319);
#15863=AXIS2_PLACEMENT_3D('',#23624,#17321,#17322);
#15864=AXIS2_PLACEMENT_3D('',#23672,#17324,#17325);
#15865=AXIS2_PLACEMENT_3D('',#23723,#17327,#17328);
#15866=AXIS2_PLACEMENT_3D('',#23774,#17330,#17331);
#15867=AXIS2_PLACEMENT_3D('',#23822,#17333,#17334);
#15868=AXIS2_PLACEMENT_3D('',#23873,#17336,#17337);
#15869=AXIS2_PLACEMENT_3D('',#23924,#17339,#17340);
#15870=AXIS2_PLACEMENT_3D('',#23972,#17342,#17343);
#15871=AXIS2_PLACEMENT_3D('',#24020,#17345,#17346);
#15872=AXIS2_PLACEMENT_3D('',#24074,#17348,#17349);
#15873=AXIS2_PLACEMENT_3D('',#24122,#17351,#17352);
#15874=AXIS2_PLACEMENT_3D('',#24170,#17354,#17355);
#15875=AXIS2_PLACEMENT_3D('',#24221,#17357,#17358);
#15876=AXIS2_PLACEMENT_3D('',#24272,#17360,#17361);
#15877=AXIS2_PLACEMENT_3D('',#24320,#17363,#17364);
#15878=AXIS2_PLACEMENT_3D('',#24371,#17366,#17367);
#15879=AXIS2_PLACEMENT_3D('',#24390,#17369,#17370);
#15880=AXIS2_PLACEMENT_3D('',#24410,#17371,#17372);
#15881=AXIS2_PLACEMENT_3D('',#24421,#17374,#17375);
#15882=AXIS2_PLACEMENT_3D('',#24428,#17376,#17377);
#15883=AXIS2_PLACEMENT_3D('',#24453,#17379,#17380);
#15884=AXIS2_PLACEMENT_3D('',#24477,#17382,#17383);
#15885=AXIS2_PLACEMENT_3D('',#24502,#17385,#17386);
#15886=AXIS2_PLACEMENT_3D('',#24526,#17388,#17389);
#15887=AXIS2_PLACEMENT_3D('',#24551,#17391,#17392);
#15888=AXIS2_PLACEMENT_3D('',#24576,#17394,#17395);
#15889=AXIS2_PLACEMENT_3D('',#24600,#17397,#17398);
#15890=AXIS2_PLACEMENT_3D('',#24625,#17400,#17401);
#15891=AXIS2_PLACEMENT_3D('',#24649,#17403,#17404);
#15892=AXIS2_PLACEMENT_3D('',#24674,#17406,#17407);
#15893=AXIS2_PLACEMENT_3D('',#24699,#17409,#17410);
#15894=AXIS2_PLACEMENT_3D('',#24723,#17412,#17413);
#15895=AXIS2_PLACEMENT_3D('',#24748,#17415,#17416);
#15896=AXIS2_PLACEMENT_3D('',#24772,#17418,#17419);
#15897=AXIS2_PLACEMENT_3D('',#24797,#17421,#17422);
#15898=AXIS2_PLACEMENT_3D('',#24822,#17424,#17425);
#15899=AXIS2_PLACEMENT_3D('',#24846,#17427,#17428);
#15900=AXIS2_PLACEMENT_3D('',#24857,#17430,#17431);
#15901=AXIS2_PLACEMENT_3D('',#24863,#17432,#17433);
#15902=AXIS2_PLACEMENT_3D('',#24885,#17435,#17436);
#15903=AXIS2_PLACEMENT_3D('',#24888,#17438,#17439);
#15904=AXIS2_PLACEMENT_3D('',#24890,#17440,#17441);
#15905=AXIS2_PLACEMENT_3D('',#24913,#17442,#17443);
#15906=AXIS2_PLACEMENT_3D('',#24961,#17445,#17446);
#15907=AXIS2_PLACEMENT_3D('',#25009,#17448,#17449);
#15908=AXIS2_PLACEMENT_3D('',#25060,#17451,#17452);
#15909=AXIS2_PLACEMENT_3D('',#25111,#17454,#17455);
#15910=AXIS2_PLACEMENT_3D('',#25159,#17457,#17458);
#15911=AXIS2_PLACEMENT_3D('',#25210,#17460,#17461);
#15912=AXIS2_PLACEMENT_3D('',#25261,#17463,#17464);
#15913=AXIS2_PLACEMENT_3D('',#25309,#17466,#17467);
#15914=AXIS2_PLACEMENT_3D('',#25357,#17469,#17470);
#15915=AXIS2_PLACEMENT_3D('',#25411,#17472,#17473);
#15916=AXIS2_PLACEMENT_3D('',#25459,#17475,#17476);
#15917=AXIS2_PLACEMENT_3D('',#25507,#17478,#17479);
#15918=AXIS2_PLACEMENT_3D('',#25558,#17481,#17482);
#15919=AXIS2_PLACEMENT_3D('',#25609,#17484,#17485);
#15920=AXIS2_PLACEMENT_3D('',#25657,#17487,#17488);
#15921=AXIS2_PLACEMENT_3D('',#25708,#17490,#17491);
#15922=AXIS2_PLACEMENT_3D('',#25727,#17493,#17494);
#15923=AXIS2_PLACEMENT_3D('',#25747,#17495,#17496);
#15924=AXIS2_PLACEMENT_3D('',#25758,#17498,#17499);
#15925=AXIS2_PLACEMENT_3D('',#25765,#17500,#17501);
#15926=AXIS2_PLACEMENT_3D('',#25790,#17503,#17504);
#15927=AXIS2_PLACEMENT_3D('',#25814,#17506,#17507);
#15928=AXIS2_PLACEMENT_3D('',#25839,#17509,#17510);
#15929=AXIS2_PLACEMENT_3D('',#25863,#17512,#17513);
#15930=AXIS2_PLACEMENT_3D('',#25888,#17515,#17516);
#15931=AXIS2_PLACEMENT_3D('',#25913,#17518,#17519);
#15932=AXIS2_PLACEMENT_3D('',#25937,#17521,#17522);
#15933=AXIS2_PLACEMENT_3D('',#25962,#17524,#17525);
#15934=AXIS2_PLACEMENT_3D('',#25986,#17527,#17528);
#15935=AXIS2_PLACEMENT_3D('',#26011,#17530,#17531);
#15936=AXIS2_PLACEMENT_3D('',#26036,#17533,#17534);
#15937=AXIS2_PLACEMENT_3D('',#26060,#17536,#17537);
#15938=AXIS2_PLACEMENT_3D('',#26085,#17539,#17540);
#15939=AXIS2_PLACEMENT_3D('',#26109,#17542,#17543);
#15940=AXIS2_PLACEMENT_3D('',#26134,#17545,#17546);
#15941=AXIS2_PLACEMENT_3D('',#26159,#17548,#17549);
#15942=AXIS2_PLACEMENT_3D('',#26183,#17551,#17552);
#15943=AXIS2_PLACEMENT_3D('',#26194,#17554,#17555);
#15944=AXIS2_PLACEMENT_3D('',#26200,#17556,#17557);
#15945=AXIS2_PLACEMENT_3D('',#26222,#17559,#17560);
#15946=AXIS2_PLACEMENT_3D('',#26225,#17562,#17563);
#15947=AXIS2_PLACEMENT_3D('',#26227,#17564,#17565);
#15948=AXIS2_PLACEMENT_3D('',#26250,#17566,#17567);
#15949=AXIS2_PLACEMENT_3D('',#26298,#17569,#17570);
#15950=AXIS2_PLACEMENT_3D('',#26346,#17572,#17573);
#15951=AXIS2_PLACEMENT_3D('',#26397,#17575,#17576);
#15952=AXIS2_PLACEMENT_3D('',#26448,#17578,#17579);
#15953=AXIS2_PLACEMENT_3D('',#26496,#17581,#17582);
#15954=AXIS2_PLACEMENT_3D('',#26547,#17584,#17585);
#15955=AXIS2_PLACEMENT_3D('',#26598,#17587,#17588);
#15956=AXIS2_PLACEMENT_3D('',#26646,#17590,#17591);
#15957=AXIS2_PLACEMENT_3D('',#26694,#17593,#17594);
#15958=AXIS2_PLACEMENT_3D('',#26748,#17596,#17597);
#15959=AXIS2_PLACEMENT_3D('',#26796,#17599,#17600);
#15960=AXIS2_PLACEMENT_3D('',#26844,#17602,#17603);
#15961=AXIS2_PLACEMENT_3D('',#26895,#17605,#17606);
#15962=AXIS2_PLACEMENT_3D('',#26946,#17608,#17609);
#15963=AXIS2_PLACEMENT_3D('',#26994,#17611,#17612);
#15964=AXIS2_PLACEMENT_3D('',#27045,#17614,#17615);
#15965=AXIS2_PLACEMENT_3D('',#27064,#17617,#17618);
#15966=AXIS2_PLACEMENT_3D('',#27084,#17619,#17620);
#15967=AXIS2_PLACEMENT_3D('',#27095,#17622,#17623);
#15968=AXIS2_PLACEMENT_3D('',#27102,#17624,#17625);
#15969=AXIS2_PLACEMENT_3D('',#27127,#17627,#17628);
#15970=AXIS2_PLACEMENT_3D('',#27151,#17630,#17631);
#15971=AXIS2_PLACEMENT_3D('',#27176,#17633,#17634);
#15972=AXIS2_PLACEMENT_3D('',#27200,#17636,#17637);
#15973=AXIS2_PLACEMENT_3D('',#27225,#17639,#17640);
#15974=AXIS2_PLACEMENT_3D('',#27250,#17642,#17643);
#15975=AXIS2_PLACEMENT_3D('',#27274,#17645,#17646);
#15976=AXIS2_PLACEMENT_3D('',#27299,#17648,#17649);
#15977=AXIS2_PLACEMENT_3D('',#27323,#17651,#17652);
#15978=AXIS2_PLACEMENT_3D('',#27348,#17654,#17655);
#15979=AXIS2_PLACEMENT_3D('',#27373,#17657,#17658);
#15980=AXIS2_PLACEMENT_3D('',#27397,#17660,#17661);
#15981=AXIS2_PLACEMENT_3D('',#27422,#17663,#17664);
#15982=AXIS2_PLACEMENT_3D('',#27446,#17666,#17667);
#15983=AXIS2_PLACEMENT_3D('',#27471,#17669,#17670);
#15984=AXIS2_PLACEMENT_3D('',#27496,#17672,#17673);
#15985=AXIS2_PLACEMENT_3D('',#27520,#17675,#17676);
#15986=AXIS2_PLACEMENT_3D('',#27531,#17678,#17679);
#15987=AXIS2_PLACEMENT_3D('',#27537,#17680,#17681);
#15988=AXIS2_PLACEMENT_3D('',#27559,#17683,#17684);
#15989=AXIS2_PLACEMENT_3D('',#27562,#17686,#17687);
#15990=AXIS2_PLACEMENT_3D('',#27564,#17688,#17689);
#15991=AXIS2_PLACEMENT_3D('',#27587,#17690,#17691);
#15992=AXIS2_PLACEMENT_3D('',#27635,#17693,#17694);
#15993=AXIS2_PLACEMENT_3D('',#27683,#17696,#17697);
#15994=AXIS2_PLACEMENT_3D('',#27734,#17699,#17700);
#15995=AXIS2_PLACEMENT_3D('',#27785,#17702,#17703);
#15996=AXIS2_PLACEMENT_3D('',#27833,#17705,#17706);
#15997=AXIS2_PLACEMENT_3D('',#27884,#17708,#17709);
#15998=AXIS2_PLACEMENT_3D('',#27935,#17711,#17712);
#15999=AXIS2_PLACEMENT_3D('',#27983,#17714,#17715);
#16000=AXIS2_PLACEMENT_3D('',#28031,#17717,#17718);
#16001=AXIS2_PLACEMENT_3D('',#28085,#17720,#17721);
#16002=AXIS2_PLACEMENT_3D('',#28133,#17723,#17724);
#16003=AXIS2_PLACEMENT_3D('',#28181,#17726,#17727);
#16004=AXIS2_PLACEMENT_3D('',#28232,#17729,#17730);
#16005=AXIS2_PLACEMENT_3D('',#28283,#17732,#17733);
#16006=AXIS2_PLACEMENT_3D('',#28331,#17735,#17736);
#16007=AXIS2_PLACEMENT_3D('',#28382,#17738,#17739);
#16008=AXIS2_PLACEMENT_3D('',#28401,#17741,#17742);
#16009=AXIS2_PLACEMENT_3D('',#28421,#17743,#17744);
#16010=AXIS2_PLACEMENT_3D('',#28432,#17746,#17747);
#16011=AXIS2_PLACEMENT_3D('',#28439,#17748,#17749);
#16012=AXIS2_PLACEMENT_3D('',#28464,#17751,#17752);
#16013=AXIS2_PLACEMENT_3D('',#28488,#17754,#17755);
#16014=AXIS2_PLACEMENT_3D('',#28513,#17757,#17758);
#16015=AXIS2_PLACEMENT_3D('',#28537,#17760,#17761);
#16016=AXIS2_PLACEMENT_3D('',#28562,#17763,#17764);
#16017=AXIS2_PLACEMENT_3D('',#28587,#17766,#17767);
#16018=AXIS2_PLACEMENT_3D('',#28611,#17769,#17770);
#16019=AXIS2_PLACEMENT_3D('',#28636,#17772,#17773);
#16020=AXIS2_PLACEMENT_3D('',#28660,#17775,#17776);
#16021=AXIS2_PLACEMENT_3D('',#28685,#17778,#17779);
#16022=AXIS2_PLACEMENT_3D('',#28710,#17781,#17782);
#16023=AXIS2_PLACEMENT_3D('',#28734,#17784,#17785);
#16024=AXIS2_PLACEMENT_3D('',#28759,#17787,#17788);
#16025=AXIS2_PLACEMENT_3D('',#28783,#17790,#17791);
#16026=AXIS2_PLACEMENT_3D('',#28808,#17793,#17794);
#16027=AXIS2_PLACEMENT_3D('',#28833,#17796,#17797);
#16028=AXIS2_PLACEMENT_3D('',#28857,#17799,#17800);
#16029=AXIS2_PLACEMENT_3D('',#28868,#17802,#17803);
#16030=AXIS2_PLACEMENT_3D('',#28874,#17804,#17805);
#16031=AXIS2_PLACEMENT_3D('',#28896,#17807,#17808);
#16032=AXIS2_PLACEMENT_3D('',#28899,#17810,#17811);
#16033=AXIS2_PLACEMENT_3D('',#28901,#17812,#17813);
#16034=AXIS2_PLACEMENT_3D('',#28924,#17814,#17815);
#16035=AXIS2_PLACEMENT_3D('',#28972,#17817,#17818);
#16036=AXIS2_PLACEMENT_3D('',#29020,#17820,#17821);
#16037=AXIS2_PLACEMENT_3D('',#29071,#17823,#17824);
#16038=AXIS2_PLACEMENT_3D('',#29122,#17826,#17827);
#16039=AXIS2_PLACEMENT_3D('',#29170,#17829,#17830);
#16040=AXIS2_PLACEMENT_3D('',#29221,#17832,#17833);
#16041=AXIS2_PLACEMENT_3D('',#29272,#17835,#17836);
#16042=AXIS2_PLACEMENT_3D('',#29320,#17838,#17839);
#16043=AXIS2_PLACEMENT_3D('',#29368,#17841,#17842);
#16044=AXIS2_PLACEMENT_3D('',#29422,#17844,#17845);
#16045=AXIS2_PLACEMENT_3D('',#29470,#17847,#17848);
#16046=AXIS2_PLACEMENT_3D('',#29518,#17850,#17851);
#16047=AXIS2_PLACEMENT_3D('',#29569,#17853,#17854);
#16048=AXIS2_PLACEMENT_3D('',#29620,#17856,#17857);
#16049=AXIS2_PLACEMENT_3D('',#29668,#17859,#17860);
#16050=AXIS2_PLACEMENT_3D('',#29719,#17862,#17863);
#16051=AXIS2_PLACEMENT_3D('',#29738,#17865,#17866);
#16052=AXIS2_PLACEMENT_3D('',#29758,#17867,#17868);
#16053=AXIS2_PLACEMENT_3D('',#29769,#17870,#17871);
#16054=AXIS2_PLACEMENT_3D('',#29776,#17872,#17873);
#16055=AXIS2_PLACEMENT_3D('',#29801,#17875,#17876);
#16056=AXIS2_PLACEMENT_3D('',#29825,#17878,#17879);
#16057=AXIS2_PLACEMENT_3D('',#29850,#17881,#17882);
#16058=AXIS2_PLACEMENT_3D('',#29874,#17884,#17885);
#16059=AXIS2_PLACEMENT_3D('',#29899,#17887,#17888);
#16060=AXIS2_PLACEMENT_3D('',#29924,#17890,#17891);
#16061=AXIS2_PLACEMENT_3D('',#29948,#17893,#17894);
#16062=AXIS2_PLACEMENT_3D('',#29973,#17896,#17897);
#16063=AXIS2_PLACEMENT_3D('',#29997,#17899,#17900);
#16064=AXIS2_PLACEMENT_3D('',#30022,#17902,#17903);
#16065=AXIS2_PLACEMENT_3D('',#30047,#17905,#17906);
#16066=AXIS2_PLACEMENT_3D('',#30071,#17908,#17909);
#16067=AXIS2_PLACEMENT_3D('',#30096,#17911,#17912);
#16068=AXIS2_PLACEMENT_3D('',#30120,#17914,#17915);
#16069=AXIS2_PLACEMENT_3D('',#30145,#17917,#17918);
#16070=AXIS2_PLACEMENT_3D('',#30170,#17920,#17921);
#16071=AXIS2_PLACEMENT_3D('',#30194,#17923,#17924);
#16072=AXIS2_PLACEMENT_3D('',#30205,#17926,#17927);
#16073=AXIS2_PLACEMENT_3D('',#30211,#17928,#17929);
#16074=AXIS2_PLACEMENT_3D('',#30233,#17931,#17932);
#16075=AXIS2_PLACEMENT_3D('',#30236,#17934,#17935);
#16076=AXIS2_PLACEMENT_3D('',#30238,#17936,#17937);
#16077=AXIS2_PLACEMENT_3D('',#30261,#17938,#17939);
#16078=AXIS2_PLACEMENT_3D('',#30309,#17941,#17942);
#16079=AXIS2_PLACEMENT_3D('',#30357,#17944,#17945);
#16080=AXIS2_PLACEMENT_3D('',#30408,#17947,#17948);
#16081=AXIS2_PLACEMENT_3D('',#30459,#17950,#17951);
#16082=AXIS2_PLACEMENT_3D('',#30507,#17953,#17954);
#16083=AXIS2_PLACEMENT_3D('',#30558,#17956,#17957);
#16084=AXIS2_PLACEMENT_3D('',#30609,#17959,#17960);
#16085=AXIS2_PLACEMENT_3D('',#30657,#17962,#17963);
#16086=AXIS2_PLACEMENT_3D('',#30705,#17965,#17966);
#16087=AXIS2_PLACEMENT_3D('',#30759,#17968,#17969);
#16088=AXIS2_PLACEMENT_3D('',#30807,#17971,#17972);
#16089=AXIS2_PLACEMENT_3D('',#30855,#17974,#17975);
#16090=AXIS2_PLACEMENT_3D('',#30906,#17977,#17978);
#16091=AXIS2_PLACEMENT_3D('',#30957,#17980,#17981);
#16092=AXIS2_PLACEMENT_3D('',#31005,#17983,#17984);
#16093=AXIS2_PLACEMENT_3D('',#31056,#17986,#17987);
#16094=AXIS2_PLACEMENT_3D('',#31075,#17989,#17990);
#16095=AXIS2_PLACEMENT_3D('',#31095,#17991,#17992);
#16096=AXIS2_PLACEMENT_3D('',#31106,#17994,#17995);
#16097=AXIS2_PLACEMENT_3D('',#31113,#17996,#17997);
#16098=AXIS2_PLACEMENT_3D('',#31138,#17999,#18000);
#16099=AXIS2_PLACEMENT_3D('',#31162,#18002,#18003);
#16100=AXIS2_PLACEMENT_3D('',#31187,#18005,#18006);
#16101=AXIS2_PLACEMENT_3D('',#31211,#18008,#18009);
#16102=AXIS2_PLACEMENT_3D('',#31236,#18011,#18012);
#16103=AXIS2_PLACEMENT_3D('',#31261,#18014,#18015);
#16104=AXIS2_PLACEMENT_3D('',#31285,#18017,#18018);
#16105=AXIS2_PLACEMENT_3D('',#31310,#18020,#18021);
#16106=AXIS2_PLACEMENT_3D('',#31334,#18023,#18024);
#16107=AXIS2_PLACEMENT_3D('',#31359,#18026,#18027);
#16108=AXIS2_PLACEMENT_3D('',#31384,#18029,#18030);
#16109=AXIS2_PLACEMENT_3D('',#31408,#18032,#18033);
#16110=AXIS2_PLACEMENT_3D('',#31433,#18035,#18036);
#16111=AXIS2_PLACEMENT_3D('',#31457,#18038,#18039);
#16112=AXIS2_PLACEMENT_3D('',#31482,#18041,#18042);
#16113=AXIS2_PLACEMENT_3D('',#31507,#18044,#18045);
#16114=AXIS2_PLACEMENT_3D('',#31531,#18047,#18048);
#16115=AXIS2_PLACEMENT_3D('',#31542,#18050,#18051);
#16116=AXIS2_PLACEMENT_3D('',#31548,#18052,#18053);
#16117=AXIS2_PLACEMENT_3D('',#31722,#18054,#18055);
#16118=AXIS2_PLACEMENT_3D('',#32934,#18056,#18057);
#16119=AXIS2_PLACEMENT_3D('',#32935,#18058,#18059);
#16120=AXIS2_PLACEMENT_3D('',#33109,#18060,#18061);
#16121=AXIS2_PLACEMENT_3D('',#34321,#18062,#18063);
#16122=AXIS2_PLACEMENT_3D('',#34322,#18064,#18065);
#16123=AXIS2_PLACEMENT_3D('',#34496,#18066,#18067);
#16124=AXIS2_PLACEMENT_3D('',#35708,#18068,#18069);
#16125=AXIS2_PLACEMENT_3D('',#35709,#18070,#18071);
#16126=AXIS2_PLACEMENT_3D('',#35883,#18072,#18073);
#16127=AXIS2_PLACEMENT_3D('',#37095,#18074,#18075);
#16128=AXIS2_PLACEMENT_3D('',#37096,#18076,#18077);
#16129=AXIS2_PLACEMENT_3D('',#37097,#18078,#18079);
#16130=AXIS2_PLACEMENT_3D('',#37098,#18080,#18081);
#16131=AXIS2_PLACEMENT_3D('',#37099,#18082,#18083);
#16132=AXIS2_PLACEMENT_3D('',#37100,#18084,#18085);
#16133=AXIS2_PLACEMENT_3D('',#37274,#18086,#18087);
#16134=AXIS2_PLACEMENT_3D('',#38486,#18088,#18089);
#16135=AXIS2_PLACEMENT_3D('',#38487,#18090,#18091);
#16136=AXIS2_PLACEMENT_3D('',#38661,#18092,#18093);
#16137=AXIS2_PLACEMENT_3D('',#39873,#18094,#18095);
#16138=AXIS2_PLACEMENT_3D('',#39874,#18096,#18097);
#16139=AXIS2_PLACEMENT_3D('',#40048,#18098,#18099);
#16140=AXIS2_PLACEMENT_3D('',#41260,#18100,#18101);
#16141=AXIS2_PLACEMENT_3D('',#41261,#18102,#18103);
#16142=AXIS2_PLACEMENT_3D('',#41435,#18104,#18105);
#16143=AXIS2_PLACEMENT_3D('',#42647,#18106,#18107);
#16144=AXIS2_PLACEMENT_3D('',#42648,#18108,#18109);
#16145=AXIS2_PLACEMENT_3D('',#42649,#18110,#18111);
#16146=AXIS2_PLACEMENT_3D('',#42650,#18112,#18113);
#16147=AXIS2_PLACEMENT_3D('',#42651,#18114,#18115);
#16148=AXIS2_PLACEMENT_3D('',#42652,#18116,#18117);
#16149=AXIS2_PLACEMENT_3D('',#42661,#18122,#18123);
#16150=AXIS2_PLACEMENT_3D('',#42667,#18127,#18128);
#16151=AXIS2_PLACEMENT_3D('',#42673,#18132,#18133);
#16152=AXIS2_PLACEMENT_3D('',#42674,#18134,#18135);
#16153=AXIS2_PLACEMENT_3D('',#42676,#18136,#18137);
#16154=AXIS2_PLACEMENT_3D('',#42677,#18138,#18139);
#16155=AXIS2_PLACEMENT_3D('',#44018,#18140,#18141);
#16156=AXIS2_PLACEMENT_3D('',#44021,#18142,#18143);
#16157=AXIS2_PLACEMENT_3D('',#44027,#18147,#18148);
#16158=AXIS2_PLACEMENT_3D('',#44028,#18149,#18150);
#16159=AXIS2_PLACEMENT_3D('',#44034,#18154,#18155);
#16160=AXIS2_PLACEMENT_3D('',#44040,#18159,#18160);
#16161=AXIS2_PLACEMENT_3D('',#44042,#18162,#18163);
#16162=AXIS2_PLACEMENT_3D('',#44043,#18164,#18165);
#16163=AXIS2_PLACEMENT_3D('',#44044,#18166,#18167);
#16164=AXIS2_PLACEMENT_3D('',#44046,#18168,#18169);
#16165=AXIS2_PLACEMENT_3D('',#44048,#18170,#18171);
#16166=AXIS2_PLACEMENT_3D('',#44049,#18172,#18173);
#16167=AXIS2_PLACEMENT_3D('',#44051,#18174,#18175);
#16168=AXIS2_PLACEMENT_3D('',#44053,#18176,#18177);
#16169=AXIS2_PLACEMENT_3D('',#44054,#18178,#18179);
#16170=AXIS2_PLACEMENT_3D('',#44056,#18181,#18182);
#16171=AXIS2_PLACEMENT_3D('',#44059,#18184,#18185);
#16172=AXIS2_PLACEMENT_3D('',#44060,#18186,#18187);
#16173=AXIS2_PLACEMENT_3D('',#44062,#18188,#18189);
#16174=AXIS2_PLACEMENT_3D('',#44063,#18190,#18191);
#16175=AXIS2_PLACEMENT_3D('',#44065,#18192,#18193);
#16176=AXIS2_PLACEMENT_3D('',#44067,#18194,#18195);
#16177=AXIS2_PLACEMENT_3D('',#44068,#18196,#18197);
#16178=AXIS2_PLACEMENT_3D('',#44070,#18199,#18200);
#16179=AXIS2_PLACEMENT_3D('',#44072,#18202,#18203);
#16180=AXIS2_PLACEMENT_3D('',#44074,#18204,#18205);
#16181=AXIS2_PLACEMENT_3D('',#44076,#18207,#18208);
#16182=AXIS2_PLACEMENT_3D('',#44077,#18209,#18210);
#16183=AXIS2_PLACEMENT_3D('',#44078,#18211,#18212);
#16184=AXIS2_PLACEMENT_3D('',#44079,#18213,#18214);
#16185=AXIS2_PLACEMENT_3D('',#44080,#18215,#18216);
#16186=AXIS2_PLACEMENT_3D('',#44090,#18218,#18219);
#16187=AXIS2_PLACEMENT_3D('',#44092,#18220,#18221);
#16188=AXIS2_PLACEMENT_3D('',#44103,#18222,#18223);
#16189=AXIS2_PLACEMENT_3D('',#44154,#18225,#18226);
#16190=AXIS2_PLACEMENT_3D('',#44205,#18228,#18229);
#16191=AXIS2_PLACEMENT_3D('',#44253,#18231,#18232);
#16192=AXIS2_PLACEMENT_3D('',#44304,#18234,#18235);
#16193=AXIS2_PLACEMENT_3D('',#44355,#18237,#18238);
#16194=AXIS2_PLACEMENT_3D('',#44403,#18240,#18241);
#16195=AXIS2_PLACEMENT_3D('',#44454,#18243,#18244);
#16196=AXIS2_PLACEMENT_3D('',#44505,#18246,#18247);
#16197=AXIS2_PLACEMENT_3D('',#44553,#18249,#18250);
#16198=AXIS2_PLACEMENT_3D('',#44604,#18252,#18253);
#16199=AXIS2_PLACEMENT_3D('',#44652,#18255,#18256);
#16200=AXIS2_PLACEMENT_3D('',#44703,#18258,#18259);
#16201=AXIS2_PLACEMENT_3D('',#44754,#18261,#18262);
#16202=AXIS2_PLACEMENT_3D('',#44802,#18264,#18265);
#16203=AXIS2_PLACEMENT_3D('',#44853,#18267,#18268);
#16204=AXIS2_PLACEMENT_3D('',#44904,#18270,#18271);
#16205=AXIS2_PLACEMENT_3D('',#44958,#18273,#18274);
#16206=AXIS2_PLACEMENT_3D('',#44972,#18276,#18277);
#16207=AXIS2_PLACEMENT_3D('',#44974,#18278,#18279);
#16208=AXIS2_PLACEMENT_3D('',#44984,#18280,#18281);
#16209=AXIS2_PLACEMENT_3D('',#45008,#18283,#18284);
#16210=AXIS2_PLACEMENT_3D('',#45033,#18286,#18287);
#16211=AXIS2_PLACEMENT_3D('',#45058,#18289,#18290);
#16212=AXIS2_PLACEMENT_3D('',#45082,#18292,#18293);
#16213=AXIS2_PLACEMENT_3D('',#45107,#18295,#18296);
#16214=AXIS2_PLACEMENT_3D('',#45132,#18298,#18299);
#16215=AXIS2_PLACEMENT_3D('',#45156,#18301,#18302);
#16216=AXIS2_PLACEMENT_3D('',#45181,#18304,#18305);
#16217=AXIS2_PLACEMENT_3D('',#45206,#18307,#18308);
#16218=AXIS2_PLACEMENT_3D('',#45230,#18310,#18311);
#16219=AXIS2_PLACEMENT_3D('',#45254,#18313,#18314);
#16220=AXIS2_PLACEMENT_3D('',#45280,#18316,#18317);
#16221=AXIS2_PLACEMENT_3D('',#45304,#18319,#18320);
#16222=AXIS2_PLACEMENT_3D('',#45328,#18322,#18323);
#16223=AXIS2_PLACEMENT_3D('',#45354,#18325,#18326);
#16224=AXIS2_PLACEMENT_3D('',#45378,#18328,#18329);
#16225=AXIS2_PLACEMENT_3D('',#45409,#18331,#18332);
#16226=AXIS2_PLACEMENT_3D('',#45411,#18333,#18334);
#16227=AXIS2_PLACEMENT_3D('',#45414,#18336,#18337);
#16228=AXIS2_PLACEMENT_3D('',#45415,#18338,#18339);
#16229=AXIS2_PLACEMENT_3D('',#45417,#18340,#18341);
#16230=AXIS2_PLACEMENT_3D('',#45418,#18342,#18343);
#16231=AXIS2_PLACEMENT_3D('',#45420,#18344,#18345);
#16232=AXIS2_PLACEMENT_3D('',#45421,#18346,#18347);
#16233=AXIS2_PLACEMENT_3D('',#45423,#18348,#18349);
#16234=AXIS2_PLACEMENT_3D('',#45425,#18351,#18352);
#16235=AXIS2_PLACEMENT_3D('',#45434,#18357,#18358);
#16236=AXIS2_PLACEMENT_3D('',#45440,#18362,#18363);
#16237=AXIS2_PLACEMENT_3D('',#45442,#18364,#18365);
#16238=AXIS2_PLACEMENT_3D('',#45444,#18367,#18368);
#16239=AXIS2_PLACEMENT_3D('',#45448,#18371,#18372);
#16240=AXIS2_PLACEMENT_3D('',#45450,#18373,#18374);
#16241=AXIS2_PLACEMENT_3D('',#45451,#18375,#18376);
#16242=AXIS2_PLACEMENT_3D('',#46060,#18377,#18378);
#16243=AXIS2_PLACEMENT_3D('',#46711,#18379,#18380);
#16244=AXIS2_PLACEMENT_3D('',#46713,#18382,#18383);
#16245=AXIS2_PLACEMENT_3D('',#46714,#18384,#18385);
#16246=AXIS2_PLACEMENT_3D('',#46716,#18387,#18388);
#16247=AXIS2_PLACEMENT_3D('',#46718,#18389,#18390);
#16248=AXIS2_PLACEMENT_3D('',#46722,#18393,#18394);
#16249=AXIS2_PLACEMENT_3D('',#46723,#18395,#18396);
#16250=AXIS2_PLACEMENT_3D('',#46724,#18397,#18398);
#16251=AXIS2_PLACEMENT_3D('',#46726,#18399,#18400);
#16252=AXIS2_PLACEMENT_3D('',#46728,#18402,#18403);
#16253=AXIS2_PLACEMENT_3D('',#46729,#18404,#18405);
#16254=AXIS2_PLACEMENT_3D('',#46731,#18406,#18407);
#16255=AXIS2_PLACEMENT_3D('',#46733,#18408,#18409);
#16256=AXIS2_PLACEMENT_3D('',#46734,#18410,#18411);
#16257=AXIS2_PLACEMENT_3D('',#46736,#18412,#18413);
#16258=AXIS2_PLACEMENT_3D('',#46738,#18414,#18415);
#16259=AXIS2_PLACEMENT_3D('',#46739,#18416,#18417);
#16260=AXIS2_PLACEMENT_3D('',#46741,#18419,#18420);
#16261=AXIS2_PLACEMENT_3D('',#46744,#18422,#18423);
#16262=AXIS2_PLACEMENT_3D('',#46745,#18424,#18425);
#16263=AXIS2_PLACEMENT_3D('',#46747,#18426,#18427);
#16264=AXIS2_PLACEMENT_3D('',#46748,#18428,#18429);
#16265=AXIS2_PLACEMENT_3D('',#46751,#18431,#18432);
#16266=AXIS2_PLACEMENT_3D('',#46752,#18433,#18434);
#16267=AXIS2_PLACEMENT_3D('',#46753,#18435,#18436);
#16268=AXIS2_PLACEMENT_3D('',#46755,#18438,#18439);
#16269=AXIS2_PLACEMENT_3D('',#46756,#18440,#18441);
#16270=AXIS2_PLACEMENT_3D('',#46758,#18442,#18443);
#16271=AXIS2_PLACEMENT_3D('',#46761,#18445,#18446);
#16272=AXIS2_PLACEMENT_3D('',#46762,#18447,#18448);
#16273=AXIS2_PLACEMENT_3D('',#46764,#18449,#18450);
#16274=AXIS2_PLACEMENT_3D('',#46767,#18452,#18453);
#16275=AXIS2_PLACEMENT_3D('',#46768,#18454,#18455);
#16276=AXIS2_PLACEMENT_3D('',#46769,#18456,#18457);
#16277=AXIS2_PLACEMENT_3D('',#46770,#18458,#18459);
#16278=AXIS2_PLACEMENT_3D('',#46771,#18460,#18461);
#16279=AXIS2_PLACEMENT_3D('',#46773,#18462,#18463);
#16280=AXIS2_PLACEMENT_3D('',#46776,#18465,#18466);
#16281=AXIS2_PLACEMENT_3D('',#46777,#18467,#18468);
#16282=AXIS2_PLACEMENT_3D('',#46779,#18469,#18470);
#16283=AXIS2_PLACEMENT_3D('',#46782,#18472,#18473);
#16284=AXIS2_PLACEMENT_3D('',#46783,#18474,#18475);
#16285=AXIS2_PLACEMENT_3D('',#46784,#18476,#18477);
#16286=AXIS2_PLACEMENT_3D('',#46785,#18478,#18479);
#16287=AXIS2_PLACEMENT_3D('',#46786,#18480,#18481);
#16288=AXIS2_PLACEMENT_3D('',#46795,#18486,#18487);
#16289=AXIS2_PLACEMENT_3D('',#46804,#18492,#18493);
#16290=AXIS2_PLACEMENT_3D('',#46805,#18494,#18495);
#16291=AXIS2_PLACEMENT_3D('',#46806,#18496,#18497);
#16292=AXIS2_PLACEMENT_3D('',#46807,#18498,#18499);
#16293=AXIS2_PLACEMENT_3D('',#46808,#18500,#18501);
#16294=AXIS2_PLACEMENT_3D('',#46809,#18502,#18503);
#16295=AXIS2_PLACEMENT_3D('',#46810,#18504,#18505);
#16296=AXIS2_PLACEMENT_3D('',#46811,#18506,#18507);
#16297=AXIS2_PLACEMENT_3D('',#46812,#18508,#18509);
#16298=AXIS2_PLACEMENT_3D('',#46813,#18510,#18511);
#16299=AXIS2_PLACEMENT_3D('',#46822,#18516,#18517);
#16300=AXIS2_PLACEMENT_3D('',#46828,#18521,#18522);
#16301=AXIS2_PLACEMENT_3D('',#46834,#18526,#18527);
#16302=AXIS2_PLACEMENT_3D('',#46837,#18530,#18531);
#16303=AXIS2_PLACEMENT_3D('',#46838,#18532,#18533);
#16304=AXIS2_PLACEMENT_3D('',#46839,#18534,#18535);
#16305=AXIS2_PLACEMENT_3D('',#46840,#18536,#18537);
#16306=AXIS2_PLACEMENT_3D('',#46865,#18539,#18540);
#16307=AXIS2_PLACEMENT_3D('',#46882,#18541,#18542);
#16308=AXIS2_PLACEMENT_3D('',#46930,#18544,#18545);
#16309=AXIS2_PLACEMENT_3D('',#46981,#18547,#18548);
#16310=AXIS2_PLACEMENT_3D('',#47032,#18550,#18551);
#16311=AXIS2_PLACEMENT_3D('',#47080,#18553,#18554);
#16312=AXIS2_PLACEMENT_3D('',#47128,#18556,#18557);
#16313=AXIS2_PLACEMENT_3D('',#47182,#18559,#18560);
#16314=AXIS2_PLACEMENT_3D('',#47230,#18562,#18563);
#16315=AXIS2_PLACEMENT_3D('',#47278,#18565,#18566);
#16316=AXIS2_PLACEMENT_3D('',#47329,#18568,#18569);
#16317=AXIS2_PLACEMENT_3D('',#47380,#18571,#18572);
#16318=AXIS2_PLACEMENT_3D('',#47428,#18574,#18575);
#16319=AXIS2_PLACEMENT_3D('',#47476,#18577,#18578);
#16320=AXIS2_PLACEMENT_3D('',#47530,#18580,#18581);
#16321=AXIS2_PLACEMENT_3D('',#47578,#18583,#18584);
#16322=AXIS2_PLACEMENT_3D('',#47626,#18586,#18587);
#16323=AXIS2_PLACEMENT_3D('',#47677,#18589,#18590);
#16324=AXIS2_PLACEMENT_3D('',#47728,#18592,#18593);
#16325=AXIS2_PLACEMENT_3D('',#47776,#18595,#18596);
#16326=AXIS2_PLACEMENT_3D('',#47824,#18598,#18599);
#16327=AXIS2_PLACEMENT_3D('',#47878,#18601,#18602);
#16328=AXIS2_PLACEMENT_3D('',#47926,#18604,#18605);
#16329=AXIS2_PLACEMENT_3D('',#47974,#18607,#18608);
#16330=AXIS2_PLACEMENT_3D('',#48025,#18610,#18611);
#16331=AXIS2_PLACEMENT_3D('',#48076,#18613,#18614);
#16332=AXIS2_PLACEMENT_3D('',#48124,#18616,#18617);
#16333=AXIS2_PLACEMENT_3D('',#48172,#18619,#18620);
#16334=AXIS2_PLACEMENT_3D('',#48226,#18622,#18623);
#16335=AXIS2_PLACEMENT_3D('',#48274,#18625,#18626);
#16336=AXIS2_PLACEMENT_3D('',#48322,#18628,#18629);
#16337=AXIS2_PLACEMENT_3D('',#48373,#18631,#18632);
#16338=AXIS2_PLACEMENT_3D('',#48424,#18634,#18635);
#16339=AXIS2_PLACEMENT_3D('',#48472,#18637,#18638);
#16340=AXIS2_PLACEMENT_3D('',#48520,#18640,#18641);
#16341=AXIS2_PLACEMENT_3D('',#48574,#18643,#18644);
#16342=AXIS2_PLACEMENT_3D('',#48622,#18646,#18647);
#16343=AXIS2_PLACEMENT_3D('',#48670,#18649,#18650);
#16344=AXIS2_PLACEMENT_3D('',#48721,#18652,#18653);
#16345=AXIS2_PLACEMENT_3D('',#48772,#18655,#18656);
#16346=AXIS2_PLACEMENT_3D('',#48820,#18658,#18659);
#16347=AXIS2_PLACEMENT_3D('',#48868,#18661,#18662);
#16348=AXIS2_PLACEMENT_3D('',#48922,#18664,#18665);
#16349=AXIS2_PLACEMENT_3D('',#48970,#18667,#18668);
#16350=AXIS2_PLACEMENT_3D('',#49018,#18670,#18671);
#16351=AXIS2_PLACEMENT_3D('',#49069,#18673,#18674);
#16352=AXIS2_PLACEMENT_3D('',#49120,#18676,#18677);
#16353=AXIS2_PLACEMENT_3D('',#49168,#18679,#18680);
#16354=AXIS2_PLACEMENT_3D('',#49216,#18682,#18683);
#16355=AXIS2_PLACEMENT_3D('',#49270,#18685,#18686);
#16356=AXIS2_PLACEMENT_3D('',#49318,#18688,#18689);
#16357=AXIS2_PLACEMENT_3D('',#49366,#18691,#18692);
#16358=AXIS2_PLACEMENT_3D('',#49417,#18694,#18695);
#16359=AXIS2_PLACEMENT_3D('',#49465,#18697,#18698);
#16360=AXIS2_PLACEMENT_3D('',#49513,#18700,#18701);
#16361=AXIS2_PLACEMENT_3D('',#49561,#18703,#18704);
#16362=AXIS2_PLACEMENT_3D('',#49615,#18706,#18707);
#16363=AXIS2_PLACEMENT_3D('',#49663,#18709,#18710);
#16364=AXIS2_PLACEMENT_3D('',#49711,#18712,#18713);
#16365=AXIS2_PLACEMENT_3D('',#49765,#18715,#18716);
#16366=AXIS2_PLACEMENT_3D('',#49813,#18718,#18719);
#16367=AXIS2_PLACEMENT_3D('',#49861,#18721,#18722);
#16368=AXIS2_PLACEMENT_3D('',#49909,#18724,#18725);
#16369=AXIS2_PLACEMENT_3D('',#49963,#18727,#18728);
#16370=AXIS2_PLACEMENT_3D('',#50011,#18730,#18731);
#16371=AXIS2_PLACEMENT_3D('',#50059,#18733,#18734);
#16372=AXIS2_PLACEMENT_3D('',#50113,#18736,#18737);
#16373=AXIS2_PLACEMENT_3D('',#50161,#18739,#18740);
#16374=AXIS2_PLACEMENT_3D('',#50209,#18742,#18743);
#16375=AXIS2_PLACEMENT_3D('',#50257,#18745,#18746);
#16376=AXIS2_PLACEMENT_3D('',#50311,#18748,#18749);
#16377=AXIS2_PLACEMENT_3D('',#50359,#18751,#18752);
#16378=AXIS2_PLACEMENT_3D('',#50407,#18754,#18755);
#16379=AXIS2_PLACEMENT_3D('',#50461,#18757,#18758);
#16380=AXIS2_PLACEMENT_3D('',#50509,#18760,#18761);
#16381=AXIS2_PLACEMENT_3D('',#50557,#18763,#18764);
#16382=AXIS2_PLACEMENT_3D('',#50605,#18766,#18767);
#16383=AXIS2_PLACEMENT_3D('',#50659,#18769,#18770);
#16384=AXIS2_PLACEMENT_3D('',#50707,#18772,#18773);
#16385=AXIS2_PLACEMENT_3D('',#50709,#18774,#18775);
#16386=AXIS2_PLACEMENT_3D('',#50713,#18777,#18778);
#16387=AXIS2_PLACEMENT_3D('',#50756,#18780,#18781);
#16388=AXIS2_PLACEMENT_3D('',#50757,#18782,#18783);
#16389=AXIS2_PLACEMENT_3D('',#50773,#18785,#18786);
#16390=AXIS2_PLACEMENT_3D('',#50781,#18787,#18788);
#16391=AXIS2_PLACEMENT_3D('',#50806,#18790,#18791);
#16392=AXIS2_PLACEMENT_3D('',#50830,#18793,#18794);
#16393=AXIS2_PLACEMENT_3D('',#50855,#18796,#18797);
#16394=AXIS2_PLACEMENT_3D('',#50880,#18799,#18800);
#16395=AXIS2_PLACEMENT_3D('',#50904,#18802,#18803);
#16396=AXIS2_PLACEMENT_3D('',#50928,#18805,#18806);
#16397=AXIS2_PLACEMENT_3D('',#50953,#18808,#18809);
#16398=AXIS2_PLACEMENT_3D('',#50978,#18811,#18812);
#16399=AXIS2_PLACEMENT_3D('',#51002,#18814,#18815);
#16400=AXIS2_PLACEMENT_3D('',#51027,#18817,#18818);
#16401=AXIS2_PLACEMENT_3D('',#51052,#18820,#18821);
#16402=AXIS2_PLACEMENT_3D('',#51076,#18823,#18824);
#16403=AXIS2_PLACEMENT_3D('',#51100,#18826,#18827);
#16404=AXIS2_PLACEMENT_3D('',#51125,#18829,#18830);
#16405=AXIS2_PLACEMENT_3D('',#51150,#18832,#18833);
#16406=AXIS2_PLACEMENT_3D('',#51174,#18835,#18836);
#16407=AXIS2_PLACEMENT_3D('',#51199,#18838,#18839);
#16408=AXIS2_PLACEMENT_3D('',#51224,#18841,#18842);
#16409=AXIS2_PLACEMENT_3D('',#51248,#18844,#18845);
#16410=AXIS2_PLACEMENT_3D('',#51272,#18847,#18848);
#16411=AXIS2_PLACEMENT_3D('',#51297,#18850,#18851);
#16412=AXIS2_PLACEMENT_3D('',#51322,#18853,#18854);
#16413=AXIS2_PLACEMENT_3D('',#51346,#18856,#18857);
#16414=AXIS2_PLACEMENT_3D('',#51371,#18859,#18860);
#16415=AXIS2_PLACEMENT_3D('',#51408,#18862,#18863);
#16416=AXIS2_PLACEMENT_3D('',#51444,#18865,#18866);
#16417=AXIS2_PLACEMENT_3D('',#51469,#18868,#18869);
#16418=AXIS2_PLACEMENT_3D('',#51493,#18871,#18872);
#16419=AXIS2_PLACEMENT_3D('',#51518,#18874,#18875);
#16420=AXIS2_PLACEMENT_3D('',#51542,#18877,#18878);
#16421=AXIS2_PLACEMENT_3D('',#51567,#18880,#18881);
#16422=AXIS2_PLACEMENT_3D('',#51592,#18883,#18884);
#16423=AXIS2_PLACEMENT_3D('',#51616,#18886,#18887);
#16424=AXIS2_PLACEMENT_3D('',#51641,#18889,#18890);
#16425=AXIS2_PLACEMENT_3D('',#51665,#18892,#18893);
#16426=AXIS2_PLACEMENT_3D('',#51690,#18895,#18896);
#16427=AXIS2_PLACEMENT_3D('',#51714,#18898,#18899);
#16428=AXIS2_PLACEMENT_3D('',#51739,#18901,#18902);
#16429=AXIS2_PLACEMENT_3D('',#51764,#18904,#18905);
#16430=AXIS2_PLACEMENT_3D('',#51788,#18907,#18908);
#16431=AXIS2_PLACEMENT_3D('',#51813,#18910,#18911);
#16432=AXIS2_PLACEMENT_3D('',#51837,#18913,#18914);
#16433=AXIS2_PLACEMENT_3D('',#51862,#18916,#18917);
#16434=AXIS2_PLACEMENT_3D('',#51886,#18919,#18920);
#16435=AXIS2_PLACEMENT_3D('',#51911,#18922,#18923);
#16436=AXIS2_PLACEMENT_3D('',#51936,#18925,#18926);
#16437=AXIS2_PLACEMENT_3D('',#51960,#18928,#18929);
#16438=AXIS2_PLACEMENT_3D('',#51985,#18931,#18932);
#16439=AXIS2_PLACEMENT_3D('',#52009,#18934,#18935);
#16440=AXIS2_PLACEMENT_3D('',#52034,#18937,#18938);
#16441=AXIS2_PLACEMENT_3D('',#52058,#18940,#18941);
#16442=AXIS2_PLACEMENT_3D('',#52083,#18943,#18944);
#16443=AXIS2_PLACEMENT_3D('',#52108,#18946,#18947);
#16444=AXIS2_PLACEMENT_3D('',#52132,#18949,#18950);
#16445=AXIS2_PLACEMENT_3D('',#52157,#18952,#18953);
#16446=AXIS2_PLACEMENT_3D('',#52181,#18955,#18956);
#16447=AXIS2_PLACEMENT_3D('',#52206,#18958,#18959);
#16448=AXIS2_PLACEMENT_3D('',#52230,#18961,#18962);
#16449=AXIS2_PLACEMENT_3D('',#52255,#18964,#18965);
#16450=AXIS2_PLACEMENT_3D('',#52280,#18967,#18968);
#16451=AXIS2_PLACEMENT_3D('',#52304,#18970,#18971);
#16452=AXIS2_PLACEMENT_3D('',#52329,#18973,#18974);
#16453=AXIS2_PLACEMENT_3D('',#52353,#18976,#18977);
#16454=AXIS2_PLACEMENT_3D('',#52378,#18979,#18980);
#16455=AXIS2_PLACEMENT_3D('',#52402,#18982,#18983);
#16456=AXIS2_PLACEMENT_3D('',#52427,#18985,#18986);
#16457=AXIS2_PLACEMENT_3D('',#52452,#18988,#18989);
#16458=AXIS2_PLACEMENT_3D('',#52476,#18991,#18992);
#16459=AXIS2_PLACEMENT_3D('',#52501,#18994,#18995);
#16460=AXIS2_PLACEMENT_3D('',#52525,#18997,#18998);
#16461=AXIS2_PLACEMENT_3D('',#52550,#19000,#19001);
#16462=AXIS2_PLACEMENT_3D('',#52574,#19003,#19004);
#16463=AXIS2_PLACEMENT_3D('',#52599,#19006,#19007);
#16464=AXIS2_PLACEMENT_3D('',#52624,#19009,#19010);
#16465=AXIS2_PLACEMENT_3D('',#52648,#19012,#19013);
#16466=AXIS2_PLACEMENT_3D('',#52673,#19015,#19016);
#16467=AXIS2_PLACEMENT_3D('',#52697,#19018,#19019);
#16468=AXIS2_PLACEMENT_3D('',#52722,#19021,#19022);
#16469=AXIS2_PLACEMENT_3D('',#52746,#19024,#19025);
#16470=AXIS2_PLACEMENT_3D('',#53102,#19026,#19027);
#16471=AXIS2_PLACEMENT_3D('',#53103,#19028,#19029);
#16472=AXIS2_PLACEMENT_3D('',#53113,#19030,#19031);
#16473=AXIS2_PLACEMENT_3D('',#53121,#19032,#19033);
#16474=AXIS2_PLACEMENT_3D('',#53123,#19034,#19035);
#16475=AXIS2_PLACEMENT_3D('',#53126,#19037,#19038);
#16476=AXIS2_PLACEMENT_3D('',#53127,#19039,#19040);
#16477=AXIS2_PLACEMENT_3D('',#53128,#19041,#19042);
#16478=AXIS2_PLACEMENT_3D('',#53130,#19043,#19044);
#16479=AXIS2_PLACEMENT_3D('',#53131,#19045,#19046);
#16480=AXIS2_PLACEMENT_3D('',#53133,#19047,#19048);
#16481=AXIS2_PLACEMENT_3D('',#53135,#19050,#19051);
#16482=AXIS2_PLACEMENT_3D('',#55424,#19052,#19053);
#16483=AXIS2_PLACEMENT_3D('',#57496,#19054,#19055);
#16484=AXIS2_PLACEMENT_3D('',#57497,#19056,#19057);
#16485=AXIS2_PLACEMENT_3D('',#57499,#19058,#19059);
#16486=AXIS2_PLACEMENT_3D('',#57502,#19061,#19062);
#16487=AXIS2_PLACEMENT_3D('',#57503,#19063,#19064);
#16488=AXIS2_PLACEMENT_3D('',#57505,#19065,#19066);
#16489=AXIS2_PLACEMENT_3D('',#57508,#19068,#19069);
#16490=AXIS2_PLACEMENT_3D('',#57509,#19070,#19071);
#16491=AXIS2_PLACEMENT_3D('',#57511,#19072,#19073);
#16492=AXIS2_PLACEMENT_3D('',#57514,#19075,#19076);
#16493=AXIS2_PLACEMENT_3D('',#57515,#19077,#19078);
#16494=AXIS2_PLACEMENT_3D('',#57517,#19079,#19080);
#16495=AXIS2_PLACEMENT_3D('',#57520,#19082,#19083);
#16496=AXIS2_PLACEMENT_3D('',#57521,#19084,#19085);
#16497=AXIS2_PLACEMENT_3D('',#57523,#19086,#19087);
#16498=AXIS2_PLACEMENT_3D('',#57526,#19089,#19090);
#16499=AXIS2_PLACEMENT_3D('',#57527,#19091,#19092);
#16500=AXIS2_PLACEMENT_3D('',#57529,#19093,#19094);
#16501=AXIS2_PLACEMENT_3D('',#57532,#19096,#19097);
#16502=AXIS2_PLACEMENT_3D('',#57533,#19098,#19099);
#16503=AXIS2_PLACEMENT_3D('',#57535,#19100,#19101);
#16504=AXIS2_PLACEMENT_3D('',#57537,#19102,#19103);
#16505=AXIS2_PLACEMENT_3D('',#57538,#19104,#19105);
#16506=AXIS2_PLACEMENT_3D('',#57540,#19106,#19107);
#16507=AXIS2_PLACEMENT_3D('',#57542,#19109,#19110);
#16508=AXIS2_PLACEMENT_3D('',#57543,#19111,#19112);
#16509=AXIS2_PLACEMENT_3D('',#57545,#19113,#19114);
#16510=AXIS2_PLACEMENT_3D('',#57546,#19115,#19116);
#16511=AXIS2_PLACEMENT_3D('',#57548,#19118,#19119);
#16512=AXIS2_PLACEMENT_3D('',#57549,#19120,#19121);
#16513=AXIS2_PLACEMENT_3D('',#57551,#19122,#19123);
#16514=AXIS2_PLACEMENT_3D('',#57554,#19125,#19126);
#16515=AXIS2_PLACEMENT_3D('',#57555,#19127,#19128);
#16516=AXIS2_PLACEMENT_3D('',#57557,#19129,#19130);
#16517=AXIS2_PLACEMENT_3D('',#57560,#19132,#19133);
#16518=AXIS2_PLACEMENT_3D('',#57561,#19134,#19135);
#16519=AXIS2_PLACEMENT_3D('',#57562,#19136,#19137);
#16520=AXIS2_PLACEMENT_3D('',#57563,#19138,#19139);
#16521=AXIS2_PLACEMENT_3D('',#57564,#19140,#19141);
#16522=AXIS2_PLACEMENT_3D('',#57573,#19146,#19147);
#16523=AXIS2_PLACEMENT_3D('',#57582,#19152,#19153);
#16524=AXIS2_PLACEMENT_3D('',#57583,#19154,#19155);
#16525=AXIS2_PLACEMENT_3D('',#57584,#19156,#19157);
#16526=AXIS2_PLACEMENT_3D('',#57585,#19158,#19159);
#16527=AXIS2_PLACEMENT_3D('',#57586,#19160,#19161);
#16528=AXIS2_PLACEMENT_3D('',#57587,#19162,#19163);
#16529=AXIS2_PLACEMENT_3D('',#57588,#19164,#19165);
#16530=AXIS2_PLACEMENT_3D('',#57589,#19166,#19167);
#16531=AXIS2_PLACEMENT_3D('',#57590,#19168,#19169);
#16532=AXIS2_PLACEMENT_3D('',#57591,#19170,#19171);
#16533=AXIS2_PLACEMENT_3D('',#57607,#19173,#19174);
#16534=AXIS2_PLACEMENT_3D('',#57615,#19175,#19176);
#16535=AXIS2_PLACEMENT_3D('',#57663,#19178,#19179);
#16536=AXIS2_PLACEMENT_3D('',#57711,#19181,#19182);
#16537=AXIS2_PLACEMENT_3D('',#57765,#19184,#19185);
#16538=AXIS2_PLACEMENT_3D('',#57813,#19187,#19188);
#16539=AXIS2_PLACEMENT_3D('',#57861,#19190,#19191);
#16540=AXIS2_PLACEMENT_3D('',#57915,#19193,#19194);
#16541=AXIS2_PLACEMENT_3D('',#57963,#19196,#19197);
#16542=AXIS2_PLACEMENT_3D('',#58011,#19199,#19200);
#16543=AXIS2_PLACEMENT_3D('',#58065,#19202,#19203);
#16544=AXIS2_PLACEMENT_3D('',#58113,#19205,#19206);
#16545=AXIS2_PLACEMENT_3D('',#58161,#19208,#19209);
#16546=AXIS2_PLACEMENT_3D('',#58215,#19211,#19212);
#16547=AXIS2_PLACEMENT_3D('',#58263,#19214,#19215);
#16548=AXIS2_PLACEMENT_3D('',#58311,#19217,#19218);
#16549=AXIS2_PLACEMENT_3D('',#58365,#19220,#19221);
#16550=AXIS2_PLACEMENT_3D('',#58413,#19223,#19224);
#16551=AXIS2_PLACEMENT_3D('',#58461,#19226,#19227);
#16552=AXIS2_PLACEMENT_3D('',#58473,#19229,#19230);
#16553=AXIS2_PLACEMENT_3D('',#58478,#19231,#19232);
#16554=AXIS2_PLACEMENT_3D('',#58503,#19234,#19235);
#16555=AXIS2_PLACEMENT_3D('',#58527,#19237,#19238);
#16556=AXIS2_PLACEMENT_3D('',#58552,#19240,#19241);
#16557=AXIS2_PLACEMENT_3D('',#58577,#19243,#19244);
#16558=AXIS2_PLACEMENT_3D('',#58601,#19246,#19247);
#16559=AXIS2_PLACEMENT_3D('',#58626,#19249,#19250);
#16560=AXIS2_PLACEMENT_3D('',#58651,#19252,#19253);
#16561=AXIS2_PLACEMENT_3D('',#58675,#19255,#19256);
#16562=AXIS2_PLACEMENT_3D('',#58700,#19258,#19259);
#16563=AXIS2_PLACEMENT_3D('',#58725,#19261,#19262);
#16564=AXIS2_PLACEMENT_3D('',#58749,#19264,#19265);
#16565=AXIS2_PLACEMENT_3D('',#58774,#19267,#19268);
#16566=AXIS2_PLACEMENT_3D('',#58799,#19270,#19271);
#16567=AXIS2_PLACEMENT_3D('',#58823,#19273,#19274);
#16568=AXIS2_PLACEMENT_3D('',#58848,#19276,#19277);
#16569=AXIS2_PLACEMENT_3D('',#58873,#19279,#19280);
#16570=AXIS2_PLACEMENT_3D('',#58897,#19282,#19283);
#16571=AXIS2_PLACEMENT_3D('',#58906,#19288,#19289);
#16572=AXIS2_PLACEMENT_3D('',#58912,#19293,#19294);
#16573=AXIS2_PLACEMENT_3D('',#58918,#19298,#19299);
#16574=AXIS2_PLACEMENT_3D('',#58924,#19303,#19304);
#16575=AXIS2_PLACEMENT_3D('',#58930,#19308,#19309);
#16576=AXIS2_PLACEMENT_3D('',#58933,#19312,#19313);
#16577=AXIS2_PLACEMENT_3D('',#59622,#19314,#19315);
#16578=AXIS2_PLACEMENT_3D('',#59624,#19316,#19317);
#16579=AXIS2_PLACEMENT_3D('',#60308,#19318,#19319);
#16580=AXIS2_PLACEMENT_3D('',#60309,#19320,#19321);
#16581=AXIS2_PLACEMENT_3D('',#60310,#19322,#19323);
#16582=AXIS2_PLACEMENT_3D('',#60311,#19324,#19325);
#16583=AXIS2_PLACEMENT_3D('',#60312,#19326,#19327);
#16584=AXIS2_PLACEMENT_3D('',#60313,#19328,#19329);
#16585=AXIS2_PLACEMENT_3D('',#60315,#19330,#19331);
#16586=AXIS2_PLACEMENT_3D('',#60317,#19332,#19333);
#16587=AXIS2_PLACEMENT_3D('',#60318,#19334,#19335);
#16588=AXIS2_PLACEMENT_3D('',#60320,#19336,#19337);
#16589=AXIS2_PLACEMENT_3D('',#60322,#19339,#19340);
#16590=AXIS2_PLACEMENT_3D('',#60325,#19342,#19343);
#16591=AXIS2_PLACEMENT_3D('',#60326,#19344,#19345);
#16592=AXIS2_PLACEMENT_3D('',#60328,#19346,#19347);
#16593=AXIS2_PLACEMENT_3D('',#60330,#19348,#19349);
#16594=AXIS2_PLACEMENT_3D('',#60331,#19350,#19351);
#16595=AXIS2_PLACEMENT_3D('',#60333,#19352,#19353);
#16596=AXIS2_PLACEMENT_3D('',#60335,#19355,#19356);
#16597=AXIS2_PLACEMENT_3D('',#60338,#19358,#19359);
#16598=AXIS2_PLACEMENT_3D('',#60339,#19360,#19361);
#16599=AXIS2_PLACEMENT_3D('',#60341,#19362,#19363);
#16600=AXIS2_PLACEMENT_3D('',#60343,#19364,#19365);
#16601=AXIS2_PLACEMENT_3D('',#60344,#19366,#19367);
#16602=AXIS2_PLACEMENT_3D('',#60346,#19368,#19369);
#16603=AXIS2_PLACEMENT_3D('',#60348,#19371,#19372);
#16604=AXIS2_PLACEMENT_3D('',#60351,#19374,#19375);
#16605=AXIS2_PLACEMENT_3D('',#60352,#19376,#19377);
#16606=AXIS2_PLACEMENT_3D('',#60354,#19378,#19379);
#16607=AXIS2_PLACEMENT_3D('',#60356,#19380,#19381);
#16608=AXIS2_PLACEMENT_3D('',#60357,#19382,#19383);
#16609=AXIS2_PLACEMENT_3D('',#60359,#19384,#19385);
#16610=AXIS2_PLACEMENT_3D('',#60361,#19387,#19388);
#16611=AXIS2_PLACEMENT_3D('',#60364,#19390,#19391);
#16612=AXIS2_PLACEMENT_3D('',#60365,#19392,#19393);
#16613=AXIS2_PLACEMENT_3D('',#60367,#19394,#19395);
#16614=AXIS2_PLACEMENT_3D('',#60370,#19397,#19398);
#16615=AXIS2_PLACEMENT_3D('',#60371,#19399,#19400);
#16616=AXIS2_PLACEMENT_3D('',#60373,#19401,#19402);
#16617=AXIS2_PLACEMENT_3D('',#60376,#19404,#19405);
#16618=AXIS2_PLACEMENT_3D('',#60377,#19406,#19407);
#16619=AXIS2_PLACEMENT_3D('',#60378,#19408,#19409);
#16620=AXIS2_PLACEMENT_3D('',#60379,#19410,#19411);
#16621=AXIS2_PLACEMENT_3D('',#60380,#19412,#19413);
#16622=AXIS2_PLACEMENT_3D('',#60382,#19414,#19415);
#16623=AXIS2_PLACEMENT_3D('',#60384,#19416,#19417);
#16624=AXIS2_PLACEMENT_3D('',#60385,#19418,#19419);
#16625=AXIS2_PLACEMENT_3D('',#60386,#19420,#19421);
#16626=AXIS2_PLACEMENT_3D('',#60389,#19423,#19424);
#16627=AXIS2_PLACEMENT_3D('',#60390,#19425,#19426);
#16628=AXIS2_PLACEMENT_3D('',#60392,#19427,#19428);
#16629=AXIS2_PLACEMENT_3D('',#60395,#19430,#19431);
#16630=AXIS2_PLACEMENT_3D('',#60396,#19432,#19433);
#16631=AXIS2_PLACEMENT_3D('',#60398,#19434,#19435);
#16632=AXIS2_PLACEMENT_3D('',#60400,#19437,#19438);
#16633=AXIS2_PLACEMENT_3D('',#60401,#19439,#19440);
#16634=AXIS2_PLACEMENT_3D('',#60402,#19441,#19442);
#16635=AXIS2_PLACEMENT_3D('',#60403,#19443,#19444);
#16636=AXIS2_PLACEMENT_3D('',#60405,#19445,#19446);
#16637=AXIS2_PLACEMENT_3D('',#60407,#19447,#19448);
#16638=AXIS2_PLACEMENT_3D('',#60408,#19449,#19450);
#16639=AXIS2_PLACEMENT_3D('',#60409,#19451,#19452);
#16640=AXIS2_PLACEMENT_3D('',#60411,#19453,#19454);
#16641=AXIS2_PLACEMENT_3D('',#60413,#19456,#19457);
#16642=AXIS2_PLACEMENT_3D('',#60416,#19459,#19460);
#16643=AXIS2_PLACEMENT_3D('',#60417,#19461,#19462);
#16644=AXIS2_PLACEMENT_3D('',#60419,#19463,#19464);
#16645=AXIS2_PLACEMENT_3D('',#60422,#19466,#19467);
#16646=AXIS2_PLACEMENT_3D('',#60423,#19468,#19469);
#16647=AXIS2_PLACEMENT_3D('',#60424,#19470,#19471);
#16648=AXIS2_PLACEMENT_3D('',#60425,#19472,#19473);
#16649=AXIS2_PLACEMENT_3D('',#60426,#19474,#19475);
#16650=AXIS2_PLACEMENT_3D('',#60429,#19476,#19477);
#16651=AXIS2_PLACEMENT_3D('',#60430,#19478,#19479);
#16652=AXIS2_PLACEMENT_3D('',#60431,#19480,#19481);
#16653=AXIS2_PLACEMENT_3D('',#60461,#19482,#19483);
#16654=AXIS2_PLACEMENT_3D('',#60476,#19484,#19485);
#16655=AXIS2_PLACEMENT_3D('',#60492,#19486,#19487);
#16656=AXIS2_PLACEMENT_3D('',#60493,#19488,#19489);
#16657=AXIS2_PLACEMENT_3D('',#60495,#19490,#19491);
#16658=AXIS2_PLACEMENT_3D('',#60512,#19493,#19494);
#16659=AXIS2_PLACEMENT_3D('',#60537,#19495,#19496);
#16660=AXIS2_PLACEMENT_3D('',#60562,#19497,#19498);
#16661=AXIS2_PLACEMENT_3D('',#60587,#19499,#19500);
#16662=AXIS2_PLACEMENT_3D('',#60617,#19501,#19502);
#16663=AXIS2_PLACEMENT_3D('',#60647,#19503,#19504);
#16664=AXIS2_PLACEMENT_3D('',#60674,#19505,#19506);
#16665=AXIS2_PLACEMENT_3D('',#60676,#19507,#19508);
#16666=AXIS2_PLACEMENT_3D('',#60706,#19509,#19510);
#16667=AXIS2_PLACEMENT_3D('',#60731,#19511,#19512);
#16668=AXIS2_PLACEMENT_3D('',#60756,#19513,#19514);
#16669=AXIS2_PLACEMENT_3D('',#60781,#19515,#19516);
#16670=AXIS2_PLACEMENT_3D('',#60794,#19517,#19518);
#16671=AXIS2_PLACEMENT_3D('',#60796,#19519,#19520);
#16672=AXIS2_PLACEMENT_3D('',#60797,#19521,#19522);
#16673=AXIS2_PLACEMENT_3D('',#60798,#19523,#19524);
#16674=AXIS2_PLACEMENT_3D('',#60826,#19525,#19526);
#16675=AXIS2_PLACEMENT_3D('',#60828,#19527,#19528);
#16676=AXIS2_PLACEMENT_3D('',#60829,#19529,#19530);
#16677=AXIS2_PLACEMENT_3D('',#60831,#19531,#19532);
#16678=AXIS2_PLACEMENT_3D('',#60832,#19533,#19534);
#16679=AXIS2_PLACEMENT_3D('',#60833,#19535,#19536);
#16680=AXIS2_PLACEMENT_3D('',#60862,#19537,#19538);
#16681=AXIS2_PLACEMENT_3D('',#60864,#19539,#19540);
#16682=AXIS2_PLACEMENT_3D('',#60865,#19541,#19542);
#16683=AXIS2_PLACEMENT_3D('',#60866,#19543,#19544);
#16684=AXIS2_PLACEMENT_3D('',#60868,#19545,#19546);
#16685=AXIS2_PLACEMENT_3D('',#60869,#19547,#19548);
#16686=AXIS2_PLACEMENT_3D('',#60870,#19549,#19550);
#16687=AXIS2_PLACEMENT_3D('',#60883,#19551,#19552);
#16688=AXIS2_PLACEMENT_3D('',#60905,#19553,#19554);
#16689=AXIS2_PLACEMENT_3D('',#60906,#19555,#19556);
#16690=AXIS2_PLACEMENT_3D('',#60908,#19557,#19558);
#16691=AXIS2_PLACEMENT_3D('',#60909,#19559,#19560);
#16692=AXIS2_PLACEMENT_3D('',#60910,#19561,#19562);
#16693=AXIS2_PLACEMENT_3D('',#60927,#19563,#19564);
#16694=AXIS2_PLACEMENT_3D('',#60945,#19565,#19566);
#16695=AXIS2_PLACEMENT_3D('',#60946,#19567,#19568);
#16696=AXIS2_PLACEMENT_3D('',#60948,#19569,#19570);
#16697=AXIS2_PLACEMENT_3D('',#60949,#19571,#19572);
#16698=AXIS2_PLACEMENT_3D('',#60950,#19573,#19574);
#16699=AXIS2_PLACEMENT_3D('',#60967,#19575,#19576);
#16700=AXIS2_PLACEMENT_3D('',#60983,#19577,#19578);
#16701=AXIS2_PLACEMENT_3D('',#60984,#19579,#19580);
#16702=AXIS2_PLACEMENT_3D('',#60986,#19581,#19582);
#16703=AXIS2_PLACEMENT_3D('',#60987,#19583,#19584);
#16704=AXIS2_PLACEMENT_3D('',#60988,#19585,#19586);
#16705=AXIS2_PLACEMENT_3D('',#61007,#19587,#19588);
#16706=AXIS2_PLACEMENT_3D('',#61023,#19589,#19590);
#16707=AXIS2_PLACEMENT_3D('',#61024,#19591,#19592);
#16708=AXIS2_PLACEMENT_3D('',#61026,#19593,#19594);
#16709=AXIS2_PLACEMENT_3D('',#61027,#19595,#19596);
#16710=AXIS2_PLACEMENT_3D('',#61028,#19597,#19598);
#16711=AXIS2_PLACEMENT_3D('',#61051,#19599,#19600);
#16712=AXIS2_PLACEMENT_3D('',#61063,#19601,#19602);
#16713=AXIS2_PLACEMENT_3D('',#61064,#19603,#19604);
#16714=AXIS2_PLACEMENT_3D('',#61066,#19605,#19606);
#16715=AXIS2_PLACEMENT_3D('',#61068,#19607,#19608);
#16716=AXIS2_PLACEMENT_3D('',#61069,#19609,#19610);
#16717=AXIS2_PLACEMENT_3D('',#61070,#19611,#19612);
#16718=AXIS2_PLACEMENT_3D('',#61098,#19613,#19614);
#16719=AXIS2_PLACEMENT_3D('',#61100,#19615,#19616);
#16720=AXIS2_PLACEMENT_3D('',#61101,#19617,#19618);
#16721=AXIS2_PLACEMENT_3D('',#61103,#19619,#19620);
#16722=AXIS2_PLACEMENT_3D('',#61104,#19621,#19622);
#16723=AXIS2_PLACEMENT_3D('',#61105,#19623,#19624);
#16724=AXIS2_PLACEMENT_3D('',#61133,#19625,#19626);
#16725=AXIS2_PLACEMENT_3D('',#61135,#19627,#19628);
#16726=AXIS2_PLACEMENT_3D('',#61136,#19629,#19630);
#16727=AXIS2_PLACEMENT_3D('',#61138,#19631,#19632);
#16728=AXIS2_PLACEMENT_3D('',#61139,#19633,#19634);
#16729=AXIS2_PLACEMENT_3D('',#61140,#19635,#19636);
#16730=AXIS2_PLACEMENT_3D('',#61168,#19637,#19638);
#16731=AXIS2_PLACEMENT_3D('',#61170,#19639,#19640);
#16732=AXIS2_PLACEMENT_3D('',#61171,#19641,#19642);
#16733=AXIS2_PLACEMENT_3D('',#61173,#19643,#19644);
#16734=AXIS2_PLACEMENT_3D('',#61174,#19645,#19646);
#16735=AXIS2_PLACEMENT_3D('',#61175,#19647,#19648);
#16736=AXIS2_PLACEMENT_3D('',#61203,#19649,#19650);
#16737=AXIS2_PLACEMENT_3D('',#61205,#19651,#19652);
#16738=AXIS2_PLACEMENT_3D('',#61206,#19653,#19654);
#16739=AXIS2_PLACEMENT_3D('',#61208,#19655,#19656);
#16740=AXIS2_PLACEMENT_3D('',#61210,#19658,#19659);
#16741=AXIS2_PLACEMENT_3D('',#61211,#19660,#19661);
#16742=AXIS2_PLACEMENT_3D('',#61212,#19662,#19663);
#16743=AXIS2_PLACEMENT_3D('',#61213,#19664,#19665);
#16744=AXIS2_PLACEMENT_3D('',#61214,#19666,#19667);
#16745=AXIS2_PLACEMENT_3D('',#61216,#19668,#19669);
#16746=AXIS2_PLACEMENT_3D('',#61219,#19671,#19672);
#16747=AXIS2_PLACEMENT_3D('',#61220,#19673,#19674);
#16748=AXIS2_PLACEMENT_3D('',#61222,#19675,#19676);
#16749=AXIS2_PLACEMENT_3D('',#61225,#19678,#19679);
#16750=AXIS2_PLACEMENT_3D('',#61226,#19680,#19681);
#16751=AXIS2_PLACEMENT_3D('',#61227,#19682,#19683);
#16752=AXIS2_PLACEMENT_3D('',#61228,#19684,#19685);
#16753=AXIS2_PLACEMENT_3D('',#61229,#19686,#19687);
#16754=AXIS2_PLACEMENT_3D('',#61245,#19689,#19690);
#16755=AXIS2_PLACEMENT_3D('',#61253,#19691,#19692);
#16756=AXIS2_PLACEMENT_3D('',#61301,#19694,#19695);
#16757=AXIS2_PLACEMENT_3D('',#61349,#19697,#19698);
#16758=AXIS2_PLACEMENT_3D('',#61403,#19700,#19701);
#16759=AXIS2_PLACEMENT_3D('',#61451,#19703,#19704);
#16760=AXIS2_PLACEMENT_3D('',#61499,#19706,#19707);
#16761=AXIS2_PLACEMENT_3D('',#61547,#19709,#19710);
#16762=AXIS2_PLACEMENT_3D('',#61601,#19712,#19713);
#16763=AXIS2_PLACEMENT_3D('',#61649,#19715,#19716);
#16764=AXIS2_PLACEMENT_3D('',#61697,#19718,#19719);
#16765=AXIS2_PLACEMENT_3D('',#61751,#19721,#19722);
#16766=AXIS2_PLACEMENT_3D('',#61799,#19724,#19725);
#16767=AXIS2_PLACEMENT_3D('',#61847,#19727,#19728);
#16768=AXIS2_PLACEMENT_3D('',#61898,#19730,#19731);
#16769=AXIS2_PLACEMENT_3D('',#61949,#19733,#19734);
#16770=AXIS2_PLACEMENT_3D('',#61997,#19736,#19737);
#16771=AXIS2_PLACEMENT_3D('',#62011,#19739,#19740);
#16772=AXIS2_PLACEMENT_3D('',#62019,#19741,#19742);
#16773=AXIS2_PLACEMENT_3D('',#62043,#19744,#19745);
#16774=AXIS2_PLACEMENT_3D('',#62067,#19747,#19748);
#16775=AXIS2_PLACEMENT_3D('',#62093,#19750,#19751);
#16776=AXIS2_PLACEMENT_3D('',#62117,#19753,#19754);
#16777=AXIS2_PLACEMENT_3D('',#62141,#19756,#19757);
#16778=AXIS2_PLACEMENT_3D('',#62166,#19759,#19760);
#16779=AXIS2_PLACEMENT_3D('',#62191,#19762,#19763);
#16780=AXIS2_PLACEMENT_3D('',#62215,#19765,#19766);
#16781=AXIS2_PLACEMENT_3D('',#62240,#19768,#19769);
#16782=AXIS2_PLACEMENT_3D('',#62265,#19771,#19772);
#16783=AXIS2_PLACEMENT_3D('',#62289,#19774,#19775);
#16784=AXIS2_PLACEMENT_3D('',#62313,#19777,#19778);
#16785=AXIS2_PLACEMENT_3D('',#62338,#19780,#19781);
#16786=AXIS2_PLACEMENT_3D('',#62363,#19783,#19784);
#16787=AXIS2_PLACEMENT_3D('',#62387,#19786,#19787);
#16788=AXIS2_PLACEMENT_3D('',#62576,#19788,#19789);
#16789=AXIS2_PLACEMENT_3D('',#62682,#19791,#19792);
#16790=AXIS2_PLACEMENT_3D('',#63214,#19793,#19794);
#16791=AXIS2_PLACEMENT_3D('',#63225,#19795,#19796);
#16792=AXIS2_PLACEMENT_3D('',#63759,#19797,#19798);
#16793=AXIS2_PLACEMENT_3D('',#63760,#19799,#19800);
#16794=AXIS2_PLACEMENT_3D('',#63769,#19805,#19806);
#16795=AXIS2_PLACEMENT_3D('',#63775,#19810,#19811);
#16796=AXIS2_PLACEMENT_3D('',#63781,#19815,#19816);
#16797=AXIS2_PLACEMENT_3D('',#63787,#19820,#19821);
#16798=AXIS2_PLACEMENT_3D('',#63793,#19825,#19826);
#16799=AXIS2_PLACEMENT_3D('',#63796,#19829,#19830);
#16800=AXIS2_PLACEMENT_3D('',#63797,#19831,#19832);
#16801=AXIS2_PLACEMENT_3D('',#63799,#19833,#19834);
#16802=AXIS2_PLACEMENT_3D('',#63800,#19835,#19836);
#16803=AXIS2_PLACEMENT_3D('',#63803,#19838,#19839);
#16804=AXIS2_PLACEMENT_3D('',#63804,#19840,#19841);
#16805=AXIS2_PLACEMENT_3D('',#63805,#19842,#19843);
#16806=AXIS2_PLACEMENT_3D('',#63806,#19844,#19845);
#16807=AXIS2_PLACEMENT_3D('',#63807,#19846,#19847);
#16808=AXIS2_PLACEMENT_3D('',#63808,#19848,#19849);
#16809=AXIS2_PLACEMENT_3D('',#63809,#19850,#19851);
#16810=AXIS2_PLACEMENT_3D('',#63810,#19852,#19853);
#16811=AXIS2_PLACEMENT_3D('',#63811,#19854,#19855);
#16812=AXIS2_PLACEMENT_3D('',#63812,#19856,#19857);
#16813=AXIS2_PLACEMENT_3D('',#63813,#19858,#19859);
#16814=AXIS2_PLACEMENT_3D('',#63814,#19860,#19861);
#16815=AXIS2_PLACEMENT_3D('',#63815,#19862,#19863);
#16816=AXIS2_PLACEMENT_3D('',#63816,#19864,#19865);
#16817=AXIS2_PLACEMENT_3D('',#63817,#19866,#19867);
#16818=AXIS2_PLACEMENT_3D('',#63818,#19868,#19869);
#16819=AXIS2_PLACEMENT_3D('',#63819,#19870,#19871);
#16820=AXIS2_PLACEMENT_3D('',#63820,#19872,#19873);
#16821=AXIS2_PLACEMENT_3D('',#63821,#19874,#19875);
#16822=AXIS2_PLACEMENT_3D('',#63822,#19876,#19877);
#16823=AXIS2_PLACEMENT_3D('',#63823,#19878,#19879);
#16824=AXIS2_PLACEMENT_3D('',#63824,#19880,#19881);
#16825=AXIS2_PLACEMENT_3D('',#63825,#19882,#19883);
#16826=AXIS2_PLACEMENT_3D('',#63826,#19884,#19885);
#16827=AXIS2_PLACEMENT_3D('',#63827,#19886,#19887);
#16828=AXIS2_PLACEMENT_3D('',#63828,#19888,#19889);
#16829=AXIS2_PLACEMENT_3D('',#63829,#19890,#19891);
#16830=AXIS2_PLACEMENT_3D('',#63830,#19892,#19893);
#16831=AXIS2_PLACEMENT_3D('',#63831,#19894,#19895);
#16832=AXIS2_PLACEMENT_3D('',#63832,#19896,#19897);
#16833=AXIS2_PLACEMENT_3D('',#63833,#19898,#19899);
#16834=AXIS2_PLACEMENT_3D('',#63834,#19900,#19901);
#16835=AXIS2_PLACEMENT_3D('',#63835,#19902,#19903);
#16836=AXIS2_PLACEMENT_3D('',#63836,#19904,#19905);
#16837=AXIS2_PLACEMENT_3D('',#63837,#19906,#19907);
#16838=AXIS2_PLACEMENT_3D('',#63838,#19908,#19909);
#16839=AXIS2_PLACEMENT_3D('',#63839,#19910,#19911);
#16840=AXIS2_PLACEMENT_3D('',#63840,#19912,#19913);
#16841=AXIS2_PLACEMENT_3D('',#63841,#19914,#19915);
#16842=AXIS2_PLACEMENT_3D('',#63842,#19916,#19917);
#16843=AXIS2_PLACEMENT_3D('',#63843,#19918,#19919);
#16844=AXIS2_PLACEMENT_3D('',#63844,#19920,#19921);
#16845=AXIS2_PLACEMENT_3D('',#63845,#19922,#19923);
#16846=AXIS2_PLACEMENT_3D('',#63846,#19924,#19925);
#16847=AXIS2_PLACEMENT_3D('',#63847,#19926,#19927);
#16848=AXIS2_PLACEMENT_3D('',#63848,#19928,#19929);
#16849=AXIS2_PLACEMENT_3D('',#63849,#19930,#19931);
#16850=AXIS2_PLACEMENT_3D('',#63850,#19932,#19933);
#16851=AXIS2_PLACEMENT_3D('',#63851,#19934,#19935);
#16852=AXIS2_PLACEMENT_3D('',#63852,#19936,#19937);
#16853=AXIS2_PLACEMENT_3D('',#63853,#19938,#19939);
#16854=AXIS2_PLACEMENT_3D('',#63854,#19940,#19941);
#16855=AXIS2_PLACEMENT_3D('',#63855,#19942,#19943);
#16856=AXIS2_PLACEMENT_3D('',#63856,#19944,#19945);
#16857=AXIS2_PLACEMENT_3D('',#63857,#19946,#19947);
#16858=AXIS2_PLACEMENT_3D('',#63858,#19948,#19949);
#16859=DIRECTION('axis',(0.,0.,1.));
#16860=DIRECTION('refdir',(1.,0.,0.));
#16861=DIRECTION('axis',(0.,0.,1.));
#16862=DIRECTION('refdir',(1.,0.,0.));
#16863=DIRECTION('center_axis',(0.,-1.,0.));
#16864=DIRECTION('ref_axis',(-1.,0.,0.));
#16865=DIRECTION('',(0.,0.,1.));
#16866=DIRECTION('',(-1.,0.,0.));
#16867=DIRECTION('',(0.,0.,-1.));
#16868=DIRECTION('',(1.,0.,0.));
#16869=DIRECTION('center_axis',(0.,0.,1.));
#16870=DIRECTION('ref_axis',(1.,0.,0.));
#16871=DIRECTION('center_axis',(0.,0.,-1.));
#16872=DIRECTION('ref_axis',(1.,0.,0.));
#16873=DIRECTION('',(0.,-1.,0.));
#16874=DIRECTION('',(-1.,0.,0.));
#16875=DIRECTION('center_axis',(0.,0.,-1.));
#16876=DIRECTION('ref_axis',(1.,0.,0.));
#16877=DIRECTION('center_axis',(0.,1.,0.));
#16878=DIRECTION('ref_axis',(1.,0.,0.));
#16879=DIRECTION('',(0.,0.,-1.));
#16880=DIRECTION('',(0.,0.,-1.));
#16881=DIRECTION('',(1.,0.,0.));
#16882=DIRECTION('center_axis',(-1.,0.,0.));
#16883=DIRECTION('ref_axis',(0.,1.,0.));
#16884=DIRECTION('',(0.,1.,0.));
#16885=DIRECTION('center_axis',(0.,0.,-1.));
#16886=DIRECTION('ref_axis',(-1.,0.,0.));
#16887=DIRECTION('center_axis',(0.,0.,1.));
#16888=DIRECTION('ref_axis',(1.,0.,0.));
#16889=DIRECTION('center_axis',(0.,0.,1.));
#16890=DIRECTION('ref_axis',(1.,0.,0.));
#16891=DIRECTION('center_axis',(0.,0.,-1.));
#16892=DIRECTION('ref_axis',(1.,0.,0.));
#16893=DIRECTION('center_axis',(0.,0.,-1.));
#16894=DIRECTION('ref_axis',(1.,0.,0.));
#16895=DIRECTION('center_axis',(0.,0.,-1.));
#16896=DIRECTION('ref_axis',(1.,0.,0.));
#16897=DIRECTION('center_axis',(0.,0.,-1.));
#16898=DIRECTION('ref_axis',(-1.,1.22464679914735E-16,0.));
#16899=DIRECTION('',(0.,0.,-1.));
#16900=DIRECTION('center_axis',(0.,0.,1.));
#16901=DIRECTION('ref_axis',(1.,0.,0.));
#16902=DIRECTION('',(0.,0.,1.));
#16903=DIRECTION('center_axis',(0.,0.,1.));
#16904=DIRECTION('ref_axis',(1.,0.,0.));
#16905=DIRECTION('center_axis',(0.,0.,-1.));
#16906=DIRECTION('ref_axis',(1.,0.,0.));
#16907=DIRECTION('',(0.,0.,1.));
#16908=DIRECTION('center_axis',(0.,0.,1.));
#16909=DIRECTION('ref_axis',(1.,0.,0.));
#16910=DIRECTION('',(0.,0.,-1.));
#16911=DIRECTION('center_axis',(0.,0.,1.));
#16912=DIRECTION('ref_axis',(1.,0.,0.));
#16913=DIRECTION('center_axis',(0.,0.,1.));
#16914=DIRECTION('ref_axis',(1.,0.,0.));
#16915=DIRECTION('',(0.,0.,-1.));
#16916=DIRECTION('center_axis',(0.,0.,-1.));
#16917=DIRECTION('ref_axis',(1.,0.,0.));
#16918=DIRECTION('center_axis',(0.,0.,-1.));
#16919=DIRECTION('ref_axis',(1.,0.,0.));
#16920=DIRECTION('center_axis',(0.,0.,-1.));
#16921=DIRECTION('ref_axis',(1.,0.,0.));
#16922=DIRECTION('',(0.,0.,-1.));
#16923=DIRECTION('center_axis',(0.,0.,1.));
#16924=DIRECTION('ref_axis',(1.,0.,0.));
#16925=DIRECTION('center_axis',(0.,0.,-1.));
#16926=DIRECTION('ref_axis',(1.,0.,0.));
#16927=DIRECTION('center_axis',(0.,0.,-1.));
#16928=DIRECTION('ref_axis',(1.,0.,0.));
#16929=DIRECTION('',(0.,0.,-1.));
#16930=DIRECTION('center_axis',(0.,0.,1.));
#16931=DIRECTION('ref_axis',(1.,0.,0.));
#16932=DIRECTION('center_axis',(0.,0.,-1.));
#16933=DIRECTION('ref_axis',(1.,0.,0.));
#16934=DIRECTION('center_axis',(0.,0.,-1.));
#16935=DIRECTION('ref_axis',(1.,0.,0.));
#16936=DIRECTION('',(0.,0.,-1.));
#16937=DIRECTION('center_axis',(0.,0.,1.));
#16938=DIRECTION('ref_axis',(1.,0.,0.));
#16939=DIRECTION('center_axis',(0.,0.,-1.));
#16940=DIRECTION('ref_axis',(1.,0.,0.));
#16941=DIRECTION('center_axis',(0.,0.,-1.));
#16942=DIRECTION('ref_axis',(1.,0.,0.));
#16943=DIRECTION('',(0.,0.,-1.));
#16944=DIRECTION('center_axis',(0.,0.,1.));
#16945=DIRECTION('ref_axis',(1.,0.,0.));
#16946=DIRECTION('center_axis',(0.,0.,-1.));
#16947=DIRECTION('ref_axis',(1.,0.,0.));
#16948=DIRECTION('center_axis',(0.,0.,-1.));
#16949=DIRECTION('ref_axis',(1.,0.,0.));
#16950=DIRECTION('',(0.,0.,-1.));
#16951=DIRECTION('center_axis',(0.,0.,1.));
#16952=DIRECTION('ref_axis',(1.,0.,0.));
#16953=DIRECTION('center_axis',(0.,0.,-1.));
#16954=DIRECTION('ref_axis',(1.,0.,0.));
#16955=DIRECTION('center_axis',(0.,0.,-1.));
#16956=DIRECTION('ref_axis',(1.,0.,0.));
#16957=DIRECTION('',(0.,0.,-1.));
#16958=DIRECTION('center_axis',(0.,0.,1.));
#16959=DIRECTION('ref_axis',(1.,0.,0.));
#16960=DIRECTION('center_axis',(0.,1.,0.));
#16961=DIRECTION('ref_axis',(-1.,0.,0.));
#16962=DIRECTION('',(-1.,0.,0.));
#16963=DIRECTION('',(0.,0.,1.));
#16964=DIRECTION('',(-1.,0.,0.));
#16965=DIRECTION('center_axis',(1.,0.,0.));
#16966=DIRECTION('ref_axis',(0.,1.,0.));
#16967=DIRECTION('',(0.,1.,0.));
#16968=DIRECTION('',(0.,1.,0.));
#16969=DIRECTION('',(0.,0.,1.));
#16970=DIRECTION('center_axis',(0.,-1.,0.));
#16971=DIRECTION('ref_axis',(1.,0.,0.));
#16972=DIRECTION('',(1.,0.,0.));
#16973=DIRECTION('',(1.,0.,0.));
#16974=DIRECTION('center_axis',(0.,0.,1.));
#16975=DIRECTION('ref_axis',(1.,0.,0.));
#16976=DIRECTION('center_axis',(0.,0.,1.));
#16977=DIRECTION('ref_axis',(1.,0.,0.));
#16978=DIRECTION('center_axis',(0.,0.,1.));
#16979=DIRECTION('ref_axis',(1.,0.,0.));
#16980=DIRECTION('center_axis',(0.,0.,1.));
#16981=DIRECTION('ref_axis',(1.,0.,0.));
#16982=DIRECTION('center_axis',(0.,0.,1.));
#16983=DIRECTION('ref_axis',(1.,0.,0.));
#16984=DIRECTION('center_axis',(0.,0.,-1.));
#16985=DIRECTION('ref_axis',(1.,0.,0.));
#16986=DIRECTION('center_axis',(0.,0.,1.));
#16987=DIRECTION('ref_axis',(1.,0.,0.));
#16988=DIRECTION('',(0.,0.,-1.));
#16989=DIRECTION('center_axis',(0.,0.,1.));
#16990=DIRECTION('ref_axis',(1.,0.,0.));
#16991=DIRECTION('',(0.,0.,-1.));
#16992=DIRECTION('center_axis',(0.,0.,1.));
#16993=DIRECTION('ref_axis',(1.,0.,0.));
#16994=DIRECTION('center_axis',(0.,0.,1.));
#16995=DIRECTION('ref_axis',(1.,0.,0.));
#16996=DIRECTION('center_axis',(0.,0.,-1.));
#16997=DIRECTION('ref_axis',(1.,0.,0.));
#16998=DIRECTION('',(0.,0.,-1.));
#16999=DIRECTION('',(0.,0.,-1.));
#17000=DIRECTION('center_axis',(0.,0.,-1.));
#17001=DIRECTION('ref_axis',(1.,0.,0.));
#17002=DIRECTION('center_axis',(0.,0.,1.));
#17003=DIRECTION('ref_axis',(1.,0.,0.));
#17004=DIRECTION('center_axis',(0.,0.,1.));
#17005=DIRECTION('ref_axis',(1.,0.,0.));
#17006=DIRECTION('axis',(0.,0.,1.));
#17007=DIRECTION('refdir',(1.,0.,0.));
#17008=DIRECTION('center_axis',(0.,0.,-1.));
#17009=DIRECTION('ref_axis',(1.,0.,0.));
#17010=DIRECTION('',(0.,0.,-1.));
#17011=DIRECTION('center_axis',(0.,0.,-1.));
#17012=DIRECTION('ref_axis',(1.,0.,0.));
#17013=DIRECTION('center_axis',(0.,0.,-1.));
#17014=DIRECTION('ref_axis',(1.,0.,0.));
#17015=DIRECTION('',(0.,0.,-1.));
#17016=DIRECTION('center_axis',(0.,0.,-1.));
#17017=DIRECTION('ref_axis',(1.,0.,0.));
#17018=DIRECTION('center_axis',(0.,0.,-1.));
#17019=DIRECTION('ref_axis',(1.,0.,0.));
#17020=DIRECTION('',(0.,0.,-1.));
#17021=DIRECTION('center_axis',(0.,0.,-1.));
#17022=DIRECTION('ref_axis',(1.,0.,0.));
#17023=DIRECTION('',(0.,0.,-1.));
#17024=DIRECTION('center_axis',(0.,0.,-1.));
#17025=DIRECTION('ref_axis',(1.,0.,0.));
#17026=DIRECTION('',(0.,0.,-1.));
#17027=DIRECTION('center_axis',(0.,0.,-1.));
#17028=DIRECTION('ref_axis',(1.,0.,0.));
#17029=DIRECTION('',(0.,0.,-1.));
#17030=DIRECTION('center_axis',(0.,0.,-1.));
#17031=DIRECTION('ref_axis',(0.936837928895156,-0.349763770255632,0.));
#17032=DIRECTION('',(0.,0.,-1.));
#17033=DIRECTION('center_axis',(0.,0.,-1.));
#17034=DIRECTION('ref_axis',(1.,0.,0.));
#17035=DIRECTION('center_axis',(0.,0.,-1.));
#17036=DIRECTION('ref_axis',(1.,-3.92491481346641E-15,0.));
#17037=DIRECTION('',(1.22464679914735E-16,-4.95661034150385E-31,-1.));
#17038=DIRECTION('center_axis',(0.,0.,1.));
#17039=DIRECTION('ref_axis',(1.,-3.92491481346641E-15,0.));
#17040=DIRECTION('center_axis',(0.,0.,-1.));
#17041=DIRECTION('ref_axis',(1.,-3.92491481346641E-15,0.));
#17042=DIRECTION('',(1.22464679914735E-16,-4.95661034150385E-31,-1.));
#17043=DIRECTION('center_axis',(0.,0.,-1.));
#17044=DIRECTION('ref_axis',(1.,-3.92491481346641E-15,0.));
#17045=DIRECTION('',(1.22464679914735E-16,-4.95661034150385E-31,-1.));
#17046=DIRECTION('center_axis',(0.,0.,-1.));
#17047=DIRECTION('ref_axis',(1.,-3.92491481346641E-15,0.));
#17048=DIRECTION('',(1.22464679914735E-16,-4.95661034150385E-31,-1.));
#17049=DIRECTION('center_axis',(0.,0.,-1.));
#17050=DIRECTION('ref_axis',(1.,-3.92491481346641E-15,0.));
#17051=DIRECTION('',(1.22464679914735E-16,-4.95661034150385E-31,-1.));
#17052=DIRECTION('center_axis',(0.,0.,-1.));
#17053=DIRECTION('ref_axis',(1.,-3.92491481346641E-15,0.));
#17054=DIRECTION('',(1.22464679914735E-16,-4.95661034150385E-31,-1.));
#17055=DIRECTION('center_axis',(0.,0.,-1.));
#17056=DIRECTION('ref_axis',(-0.608987936736927,-0.793179483414,0.));
#17057=DIRECTION('',(1.22464679914735E-16,-4.95661034150385E-31,-1.));
#17058=DIRECTION('center_axis',(0.,0.,-1.));
#17059=DIRECTION('ref_axis',(1.,-3.92491481346641E-15,0.));
#17060=DIRECTION('center_axis',(0.,0.,1.));
#17061=DIRECTION('ref_axis',(-1.,0.,0.));
#17062=DIRECTION('',(0.,0.,1.));
#17063=DIRECTION('center_axis',(0.,0.,-1.));
#17064=DIRECTION('ref_axis',(-1.,0.,0.));
#17065=DIRECTION('',(0.,0.,1.));
#17066=DIRECTION('center_axis',(0.,0.,-1.));
#17067=DIRECTION('ref_axis',(-1.,0.,0.));
#17068=DIRECTION('center_axis',(0.,0.,-1.));
#17069=DIRECTION('ref_axis',(-1.,0.,0.));
#17070=DIRECTION('center_axis',(0.,0.,1.));
#17071=DIRECTION('ref_axis',(-1.,0.,0.));
#17072=DIRECTION('',(0.,0.,1.));
#17073=DIRECTION('center_axis',(0.,0.,1.));
#17074=DIRECTION('ref_axis',(-1.,0.,0.));
#17075=DIRECTION('',(0.,0.,1.));
#17076=DIRECTION('center_axis',(0.,0.,1.));
#17077=DIRECTION('ref_axis',(-1.,0.,0.));
#17078=DIRECTION('',(0.,0.,1.));
#17079=DIRECTION('center_axis',(0.,0.,1.));
#17080=DIRECTION('ref_axis',(-1.,0.,0.));
#17081=DIRECTION('',(0.,0.,1.));
#17082=DIRECTION('center_axis',(0.,0.,1.));
#17083=DIRECTION('ref_axis',(-1.,0.,0.));
#17084=DIRECTION('',(0.,0.,1.));
#17085=DIRECTION('center_axis',(0.,0.,1.));
#17086=DIRECTION('ref_axis',(-1.,0.,0.));
#17087=DIRECTION('',(0.,0.,1.));
#17088=DIRECTION('center_axis',(0.,0.,1.));
#17089=DIRECTION('ref_axis',(-1.,0.,0.));
#17090=DIRECTION('',(0.,0.,1.));
#17091=DIRECTION('center_axis',(0.,0.,1.));
#17092=DIRECTION('ref_axis',(-1.,0.,0.));
#17093=DIRECTION('',(0.,0.,1.));
#17094=DIRECTION('center_axis',(0.,0.,1.));
#17095=DIRECTION('ref_axis',(-1.,0.,0.));
#17096=DIRECTION('',(0.,0.,1.));
#17097=DIRECTION('center_axis',(0.,0.,1.));
#17098=DIRECTION('ref_axis',(-1.,0.,0.));
#17099=DIRECTION('',(0.,0.,1.));
#17100=DIRECTION('center_axis',(0.,0.,1.));
#17101=DIRECTION('ref_axis',(-1.,0.,0.));
#17102=DIRECTION('',(0.,0.,1.));
#17103=DIRECTION('center_axis',(0.,0.,1.));
#17104=DIRECTION('ref_axis',(-1.,0.,0.));
#17105=DIRECTION('',(0.,0.,1.));
#17106=DIRECTION('center_axis',(0.,0.,1.));
#17107=DIRECTION('ref_axis',(-1.,0.,0.));
#17108=DIRECTION('',(0.,0.,1.));
#17109=DIRECTION('center_axis',(0.,0.,1.));
#17110=DIRECTION('ref_axis',(-1.,0.,0.));
#17111=DIRECTION('',(0.,0.,1.));
#17112=DIRECTION('center_axis',(0.,0.,1.));
#17113=DIRECTION('ref_axis',(-1.,0.,0.));
#17114=DIRECTION('',(0.,0.,1.));
#17115=DIRECTION('center_axis',(0.,0.,1.));
#17116=DIRECTION('ref_axis',(-1.,0.,0.));
#17117=DIRECTION('',(0.,0.,1.));
#17118=DIRECTION('center_axis',(0.,0.,1.));
#17119=DIRECTION('ref_axis',(-0.938438080411676,-0.34544749128232,0.));
#17120=DIRECTION('',(0.,0.,1.));
#17121=DIRECTION('center_axis',(0.,0.,-1.));
#17122=DIRECTION('ref_axis',(-1.,0.,0.));
#17123=DIRECTION('center_axis',(0.,0.,1.));
#17124=DIRECTION('ref_axis',(0.417702001320551,0.908584084217199,0.));
#17125=DIRECTION('',(-1.22464679914735E-16,-1.24549850322111E-29,1.));
#17126=DIRECTION('center_axis',(0.,0.,-1.));
#17127=DIRECTION('ref_axis',(-1.,-1.01580206170838E-13,0.));
#17128=DIRECTION('center_axis',(0.,0.,1.));
#17129=DIRECTION('ref_axis',(-1.,-1.01580206170838E-13,0.));
#17130=DIRECTION('',(-1.22464679914735E-16,-1.24549850322111E-29,1.));
#17131=DIRECTION('center_axis',(0.,0.,1.));
#17132=DIRECTION('ref_axis',(-1.,-1.01580206170838E-13,0.));
#17133=DIRECTION('',(-1.22464679914735E-16,-1.24549850322111E-29,1.));
#17134=DIRECTION('center_axis',(0.,0.,1.));
#17135=DIRECTION('ref_axis',(-1.,-1.01580206170838E-13,0.));
#17136=DIRECTION('',(-1.22464679914735E-16,-1.24549850322111E-29,1.));
#17137=DIRECTION('center_axis',(0.,0.,1.));
#17138=DIRECTION('ref_axis',(-1.,-1.01580206170838E-13,0.));
#17139=DIRECTION('',(-1.22464679914735E-16,-1.24549850322111E-29,1.));
#17140=DIRECTION('center_axis',(0.,0.,1.));
#17141=DIRECTION('ref_axis',(-1.,-1.01580206170838E-13,0.));
#17142=DIRECTION('',(-1.22464679914735E-16,-1.24549850322111E-29,1.));
#17143=DIRECTION('center_axis',(0.,0.,1.));
#17144=DIRECTION('ref_axis',(-1.,-1.01580206170838E-13,0.));
#17145=DIRECTION('',(-1.22464679914735E-16,-1.24549850322111E-29,1.));
#17146=DIRECTION('center_axis',(0.,0.,1.));
#17147=DIRECTION('ref_axis',(-1.,-1.01580206170838E-13,0.));
#17148=DIRECTION('',(-1.22464679914735E-16,-1.24549850322111E-29,1.));
#17149=DIRECTION('center_axis',(0.,0.,1.));
#17150=DIRECTION('ref_axis',(-1.,-1.01580206170838E-13,0.));
#17151=DIRECTION('',(-1.22464679914735E-16,-1.24549850322111E-29,1.));
#17152=DIRECTION('center_axis',(0.,0.,1.));
#17153=DIRECTION('ref_axis',(-1.,-1.01580206170838E-13,0.));
#17154=DIRECTION('',(-1.22464679914735E-16,-1.24549850322111E-29,1.));
#17155=DIRECTION('center_axis',(0.,0.,1.));
#17156=DIRECTION('ref_axis',(-1.,-1.01580206170838E-13,0.));
#17157=DIRECTION('',(-1.22464679914735E-16,-1.24549850322111E-29,1.));
#17158=DIRECTION('center_axis',(0.,0.,1.));
#17159=DIRECTION('ref_axis',(-1.,-1.01580206170838E-13,0.));
#17160=DIRECTION('',(-1.22464679914735E-16,-1.24549850322111E-29,1.));
#17161=DIRECTION('center_axis',(0.,0.,1.));
#17162=DIRECTION('ref_axis',(-1.,-1.01580206170838E-13,0.));
#17163=DIRECTION('',(-1.22464679914735E-16,-1.24549850322111E-29,1.));
#17164=DIRECTION('center_axis',(0.,0.,1.));
#17165=DIRECTION('ref_axis',(-1.,-1.01580206170838E-13,0.));
#17166=DIRECTION('',(-1.22464679914735E-16,-1.24549850322111E-29,1.));
#17167=DIRECTION('center_axis',(0.,0.,1.));
#17168=DIRECTION('ref_axis',(-1.,-1.01580206170838E-13,0.));
#17169=DIRECTION('',(-1.22464679914735E-16,-1.24549850322111E-29,1.));
#17170=DIRECTION('center_axis',(0.,0.,1.));
#17171=DIRECTION('ref_axis',(-1.,-1.01580206170838E-13,0.));
#17172=DIRECTION('',(-1.22464679914735E-16,-1.24549850322111E-29,1.));
#17173=DIRECTION('center_axis',(0.,0.,1.));
#17174=DIRECTION('ref_axis',(-1.,-1.01580206170838E-13,0.));
#17175=DIRECTION('',(-1.22464679914735E-16,-1.24549850322111E-29,1.));
#17176=DIRECTION('center_axis',(0.,0.,1.));
#17177=DIRECTION('ref_axis',(-1.,-1.01580206170838E-13,0.));
#17178=DIRECTION('',(-1.22464679914735E-16,-1.24549850322111E-29,1.));
#17179=DIRECTION('center_axis',(0.,0.,1.));
#17180=DIRECTION('ref_axis',(0.609342743503397,-0.792906943430157,0.));
#17181=DIRECTION('',(-1.22464679914735E-16,-1.24549850322111E-29,1.));
#17182=DIRECTION('center_axis',(0.,0.,1.));
#17183=DIRECTION('ref_axis',(-1.,-1.01580206170838E-13,0.));
#17184=DIRECTION('center_axis',(0.,0.,1.));
#17185=DIRECTION('ref_axis',(-1.,0.,0.));
#17186=DIRECTION('',(0.,0.,1.));
#17187=DIRECTION('center_axis',(0.,0.,-1.));
#17188=DIRECTION('ref_axis',(-1.,0.,0.));
#17189=DIRECTION('',(0.,0.,1.));
#17190=DIRECTION('center_axis',(0.,0.,-1.));
#17191=DIRECTION('ref_axis',(-1.,0.,0.));
#17192=DIRECTION('center_axis',(0.,0.,-1.));
#17193=DIRECTION('ref_axis',(-1.,0.,0.));
#17194=DIRECTION('center_axis',(0.,0.,1.));
#17195=DIRECTION('ref_axis',(-1.,0.,0.));
#17196=DIRECTION('',(0.,0.,1.));
#17197=DIRECTION('center_axis',(0.,0.,1.));
#17198=DIRECTION('ref_axis',(-1.,0.,0.));
#17199=DIRECTION('',(0.,0.,1.));
#17200=DIRECTION('center_axis',(0.,0.,1.));
#17201=DIRECTION('ref_axis',(-1.,0.,0.));
#17202=DIRECTION('',(0.,0.,1.));
#17203=DIRECTION('center_axis',(0.,0.,1.));
#17204=DIRECTION('ref_axis',(-1.,0.,0.));
#17205=DIRECTION('',(0.,0.,1.));
#17206=DIRECTION('center_axis',(0.,0.,1.));
#17207=DIRECTION('ref_axis',(-1.,0.,0.));
#17208=DIRECTION('',(0.,0.,1.));
#17209=DIRECTION('center_axis',(0.,0.,1.));
#17210=DIRECTION('ref_axis',(-1.,0.,0.));
#17211=DIRECTION('',(0.,0.,1.));
#17212=DIRECTION('center_axis',(0.,0.,1.));
#17213=DIRECTION('ref_axis',(-1.,0.,0.));
#17214=DIRECTION('',(0.,0.,1.));
#17215=DIRECTION('center_axis',(0.,0.,1.));
#17216=DIRECTION('ref_axis',(-1.,0.,0.));
#17217=DIRECTION('',(0.,0.,1.));
#17218=DIRECTION('center_axis',(0.,0.,1.));
#17219=DIRECTION('ref_axis',(-1.,0.,0.));
#17220=DIRECTION('',(0.,0.,1.));
#17221=DIRECTION('center_axis',(0.,0.,1.));
#17222=DIRECTION('ref_axis',(-1.,0.,0.));
#17223=DIRECTION('',(0.,0.,1.));
#17224=DIRECTION('center_axis',(0.,0.,1.));
#17225=DIRECTION('ref_axis',(-1.,0.,0.));
#17226=DIRECTION('',(0.,0.,1.));
#17227=DIRECTION('center_axis',(0.,0.,1.));
#17228=DIRECTION('ref_axis',(-1.,0.,0.));
#17229=DIRECTION('',(0.,0.,1.));
#17230=DIRECTION('center_axis',(0.,0.,1.));
#17231=DIRECTION('ref_axis',(-1.,0.,0.));
#17232=DIRECTION('',(0.,0.,1.));
#17233=DIRECTION('center_axis',(0.,0.,1.));
#17234=DIRECTION('ref_axis',(-1.,0.,0.));
#17235=DIRECTION('',(0.,0.,1.));
#17236=DIRECTION('center_axis',(0.,0.,1.));
#17237=DIRECTION('ref_axis',(-1.,0.,0.));
#17238=DIRECTION('',(0.,0.,1.));
#17239=DIRECTION('center_axis',(0.,0.,1.));
#17240=DIRECTION('ref_axis',(-1.,0.,0.));
#17241=DIRECTION('',(0.,0.,1.));
#17242=DIRECTION('center_axis',(0.,0.,1.));
#17243=DIRECTION('ref_axis',(-0.938438085006596,-0.345447478799822,0.));
#17244=DIRECTION('',(0.,0.,1.));
#17245=DIRECTION('center_axis',(0.,0.,-1.));
#17246=DIRECTION('ref_axis',(-1.,0.,0.));
#17247=DIRECTION('center_axis',(0.,0.,1.));
#17248=DIRECTION('ref_axis',(0.417701990298203,0.908584089284487,0.));
#17249=DIRECTION('',(-1.22464679914735E-16,-1.29843461996317E-29,1.));
#17250=DIRECTION('center_axis',(0.,0.,-1.));
#17251=DIRECTION('ref_axis',(-1.,-1.05902768135554E-13,0.));
#17252=DIRECTION('center_axis',(0.,0.,1.));
#17253=DIRECTION('ref_axis',(-1.,-1.05902768135554E-13,0.));
#17254=DIRECTION('',(-1.22464679914735E-16,-1.29843461996317E-29,1.));
#17255=DIRECTION('center_axis',(0.,0.,1.));
#17256=DIRECTION('ref_axis',(-1.,-1.05902768135554E-13,0.));
#17257=DIRECTION('',(-1.22464679914735E-16,-1.29843461996317E-29,1.));
#17258=DIRECTION('center_axis',(0.,0.,1.));
#17259=DIRECTION('ref_axis',(-1.,-1.05902768135554E-13,0.));
#17260=DIRECTION('',(-1.22464679914735E-16,-1.29843461996317E-29,1.));
#17261=DIRECTION('center_axis',(0.,0.,1.));
#17262=DIRECTION('ref_axis',(-1.,-1.05902768135554E-13,0.));
#17263=DIRECTION('',(-1.22464679914735E-16,-1.29843461996317E-29,1.));
#17264=DIRECTION('center_axis',(0.,0.,1.));
#17265=DIRECTION('ref_axis',(-1.,-1.05902768135554E-13,0.));
#17266=DIRECTION('',(-1.22464679914735E-16,-1.29843461996317E-29,1.));
#17267=DIRECTION('center_axis',(0.,0.,1.));
#17268=DIRECTION('ref_axis',(-1.,-1.05902768135554E-13,0.));
#17269=DIRECTION('',(-1.22464679914735E-16,-1.29843461996317E-29,1.));
#17270=DIRECTION('center_axis',(0.,0.,1.));
#17271=DIRECTION('ref_axis',(-1.,-1.05902768135554E-13,0.));
#17272=DIRECTION('',(-1.22464679914735E-16,-1.29843461996317E-29,1.));
#17273=DIRECTION('center_axis',(0.,0.,1.));
#17274=DIRECTION('ref_axis',(-1.,-1.05902768135554E-13,0.));
#17275=DIRECTION('',(-1.22464679914735E-16,-1.29843461996317E-29,1.));
#17276=DIRECTION('center_axis',(0.,0.,1.));
#17277=DIRECTION('ref_axis',(-1.,-1.05902768135554E-13,0.));
#17278=DIRECTION('',(-1.22464679914735E-16,-1.29843461996317E-29,1.));
#17279=DIRECTION('center_axis',(0.,0.,1.));
#17280=DIRECTION('ref_axis',(-1.,-1.05902768135554E-13,0.));
#17281=DIRECTION('',(-1.22464679914735E-16,-1.29843461996317E-29,1.));
#17282=DIRECTION('center_axis',(0.,0.,1.));
#17283=DIRECTION('ref_axis',(-1.,-1.05902768135554E-13,0.));
#17284=DIRECTION('',(-1.22464679914735E-16,-1.29843461996317E-29,1.));
#17285=DIRECTION('center_axis',(0.,0.,1.));
#17286=DIRECTION('ref_axis',(-1.,-1.05902768135554E-13,0.));
#17287=DIRECTION('',(-1.22464679914735E-16,-1.29843461996317E-29,1.));
#17288=DIRECTION('center_axis',(0.,0.,1.));
#17289=DIRECTION('ref_axis',(-1.,-1.05902768135554E-13,0.));
#17290=DIRECTION('',(-1.22464679914735E-16,-1.29843461996317E-29,1.));
#17291=DIRECTION('center_axis',(0.,0.,1.));
#17292=DIRECTION('ref_axis',(-1.,-1.05902768135554E-13,0.));
#17293=DIRECTION('',(-1.22464679914735E-16,-1.29843461996317E-29,1.));
#17294=DIRECTION('center_axis',(0.,0.,1.));
#17295=DIRECTION('ref_axis',(-1.,-1.05902768135554E-13,0.));
#17296=DIRECTION('',(-1.22464679914735E-16,-1.29843461996317E-29,1.));
#17297=DIRECTION('center_axis',(0.,0.,1.));
#17298=DIRECTION('ref_axis',(-1.,-1.05902768135554E-13,0.));
#17299=DIRECTION('',(-1.22464679914735E-16,-1.29843461996317E-29,1.));
#17300=DIRECTION('center_axis',(0.,0.,1.));
#17301=DIRECTION('ref_axis',(-1.,-1.05902768135554E-13,0.));
#17302=DIRECTION('',(-1.22464679914735E-16,-1.29843461996317E-29,1.));
#17303=DIRECTION('center_axis',(0.,0.,1.));
#17304=DIRECTION('ref_axis',(0.609342733687785,-0.792906950973377,0.));
#17305=DIRECTION('',(-1.22464679914735E-16,-1.29843461996317E-29,1.));
#17306=DIRECTION('center_axis',(0.,0.,1.));
#17307=DIRECTION('ref_axis',(-1.,-1.05902768135554E-13,0.));
#17308=DIRECTION('center_axis',(0.,0.,1.));
#17309=DIRECTION('ref_axis',(-1.,0.,0.));
#17310=DIRECTION('',(0.,0.,1.));
#17311=DIRECTION('center_axis',(0.,0.,-1.));
#17312=DIRECTION('ref_axis',(-1.,0.,0.));
#17313=DIRECTION('',(0.,0.,1.));
#17314=DIRECTION('center_axis',(0.,0.,-1.));
#17315=DIRECTION('ref_axis',(-1.,0.,0.));
#17316=DIRECTION('center_axis',(0.,0.,-1.));
#17317=DIRECTION('ref_axis',(-1.,0.,0.));
#17318=DIRECTION('center_axis',(0.,0.,1.));
#17319=DIRECTION('ref_axis',(-1.,0.,0.));
#17320=DIRECTION('',(0.,0.,1.));
#17321=DIRECTION('center_axis',(0.,0.,1.));
#17322=DIRECTION('ref_axis',(-1.,0.,0.));
#17323=DIRECTION('',(0.,0.,1.));
#17324=DIRECTION('center_axis',(0.,0.,1.));
#17325=DIRECTION('ref_axis',(-1.,0.,0.));
#17326=DIRECTION('',(0.,0.,1.));
#17327=DIRECTION('center_axis',(0.,0.,1.));
#17328=DIRECTION('ref_axis',(-1.,0.,0.));
#17329=DIRECTION('',(0.,0.,1.));
#17330=DIRECTION('center_axis',(0.,0.,1.));
#17331=DIRECTION('ref_axis',(-1.,0.,0.));
#17332=DIRECTION('',(0.,0.,1.));
#17333=DIRECTION('center_axis',(0.,0.,1.));
#17334=DIRECTION('ref_axis',(-1.,0.,0.));
#17335=DIRECTION('',(0.,0.,1.));
#17336=DIRECTION('center_axis',(0.,0.,1.));
#17337=DIRECTION('ref_axis',(-1.,0.,0.));
#17338=DIRECTION('',(0.,0.,1.));
#17339=DIRECTION('center_axis',(0.,0.,1.));
#17340=DIRECTION('ref_axis',(-1.,0.,0.));
#17341=DIRECTION('',(0.,0.,1.));
#17342=DIRECTION('center_axis',(0.,0.,1.));
#17343=DIRECTION('ref_axis',(-1.,0.,0.));
#17344=DIRECTION('',(0.,0.,1.));
#17345=DIRECTION('center_axis',(0.,0.,1.));
#17346=DIRECTION('ref_axis',(-1.,0.,0.));
#17347=DIRECTION('',(0.,0.,1.));
#17348=DIRECTION('center_axis',(0.,0.,1.));
#17349=DIRECTION('ref_axis',(-1.,0.,0.));
#17350=DIRECTION('',(0.,0.,1.));
#17351=DIRECTION('center_axis',(0.,0.,1.));
#17352=DIRECTION('ref_axis',(-1.,0.,0.));
#17353=DIRECTION('',(0.,0.,1.));
#17354=DIRECTION('center_axis',(0.,0.,1.));
#17355=DIRECTION('ref_axis',(-1.,0.,0.));
#17356=DIRECTION('',(0.,0.,1.));
#17357=DIRECTION('center_axis',(0.,0.,1.));
#17358=DIRECTION('ref_axis',(-1.,0.,0.));
#17359=DIRECTION('',(0.,0.,1.));
#17360=DIRECTION('center_axis',(0.,0.,1.));
#17361=DIRECTION('ref_axis',(-1.,0.,0.));
#17362=DIRECTION('',(0.,0.,1.));
#17363=DIRECTION('center_axis',(0.,0.,1.));
#17364=DIRECTION('ref_axis',(-1.,0.,0.));
#17365=DIRECTION('',(0.,0.,1.));
#17366=DIRECTION('center_axis',(0.,0.,1.));
#17367=DIRECTION('ref_axis',(-0.938438094004156,-0.345447454357167,0.));
#17368=DIRECTION('',(0.,0.,1.));
#17369=DIRECTION('center_axis',(0.,0.,-1.));
#17370=DIRECTION('ref_axis',(-1.,0.,0.));
#17371=DIRECTION('center_axis',(0.,0.,1.));
#17372=DIRECTION('ref_axis',(0.417701964204128,0.908584101280676,0.));
#17373=DIRECTION('',(-1.22464679914735E-16,-1.29843461996317E-29,1.));
#17374=DIRECTION('center_axis',(0.,0.,-1.));
#17375=DIRECTION('ref_axis',(-1.,-1.05902768135554E-13,0.));
#17376=DIRECTION('center_axis',(0.,0.,1.));
#17377=DIRECTION('ref_axis',(-1.,-1.05902768135554E-13,0.));
#17378=DIRECTION('',(-1.22464679914735E-16,-1.29843461996317E-29,1.));
#17379=DIRECTION('center_axis',(0.,0.,1.));
#17380=DIRECTION('ref_axis',(-1.,-1.05902768135554E-13,0.));
#17381=DIRECTION('',(-1.22464679914735E-16,-1.29843461996317E-29,1.));
#17382=DIRECTION('center_axis',(0.,0.,1.));
#17383=DIRECTION('ref_axis',(-1.,-1.05902768135554E-13,0.));
#17384=DIRECTION('',(-1.22464679914735E-16,-1.29843461996317E-29,1.));
#17385=DIRECTION('center_axis',(0.,0.,1.));
#17386=DIRECTION('ref_axis',(-1.,-1.05902768135554E-13,0.));
#17387=DIRECTION('',(-1.22464679914735E-16,-1.29843461996317E-29,1.));
#17388=DIRECTION('center_axis',(0.,0.,1.));
#17389=DIRECTION('ref_axis',(-1.,-1.05902768135554E-13,0.));
#17390=DIRECTION('',(-1.22464679914735E-16,-1.29843461996317E-29,1.));
#17391=DIRECTION('center_axis',(0.,0.,1.));
#17392=DIRECTION('ref_axis',(-1.,-1.05902768135554E-13,0.));
#17393=DIRECTION('',(-1.22464679914735E-16,-1.29843461996317E-29,1.));
#17394=DIRECTION('center_axis',(0.,0.,1.));
#17395=DIRECTION('ref_axis',(-1.,-1.05902768135554E-13,0.));
#17396=DIRECTION('',(-1.22464679914735E-16,-1.29843461996317E-29,1.));
#17397=DIRECTION('center_axis',(0.,0.,1.));
#17398=DIRECTION('ref_axis',(-1.,-1.05902768135554E-13,0.));
#17399=DIRECTION('',(-1.22464679914735E-16,-1.29843461996317E-29,1.));
#17400=DIRECTION('center_axis',(0.,0.,1.));
#17401=DIRECTION('ref_axis',(-1.,-1.05902768135554E-13,0.));
#17402=DIRECTION('',(-1.22464679914735E-16,-1.29843461996317E-29,1.));
#17403=DIRECTION('center_axis',(0.,0.,1.));
#17404=DIRECTION('ref_axis',(-1.,-1.05902768135554E-13,0.));
#17405=DIRECTION('',(-1.22464679914735E-16,-1.29843461996317E-29,1.));
#17406=DIRECTION('center_axis',(0.,0.,1.));
#17407=DIRECTION('ref_axis',(-1.,-1.05902768135554E-13,0.));
#17408=DIRECTION('',(-1.22464679914735E-16,-1.29843461996317E-29,1.));
#17409=DIRECTION('center_axis',(0.,0.,1.));
#17410=DIRECTION('ref_axis',(-1.,-1.05902768135554E-13,0.));
#17411=DIRECTION('',(-1.22464679914735E-16,-1.29843461996317E-29,1.));
#17412=DIRECTION('center_axis',(0.,0.,1.));
#17413=DIRECTION('ref_axis',(-1.,-1.05902768135554E-13,0.));
#17414=DIRECTION('',(-1.22464679914735E-16,-1.29843461996317E-29,1.));
#17415=DIRECTION('center_axis',(0.,0.,1.));
#17416=DIRECTION('ref_axis',(-1.,-1.05902768135554E-13,0.));
#17417=DIRECTION('',(-1.22464679914735E-16,-1.29843461996317E-29,1.));
#17418=DIRECTION('center_axis',(0.,0.,1.));
#17419=DIRECTION('ref_axis',(-1.,-1.05902768135554E-13,0.));
#17420=DIRECTION('',(-1.22464679914735E-16,-1.29843461996317E-29,1.));
#17421=DIRECTION('center_axis',(0.,0.,1.));
#17422=DIRECTION('ref_axis',(-1.,-1.05902768135554E-13,0.));
#17423=DIRECTION('',(-1.22464679914735E-16,-1.29843461996317E-29,1.));
#17424=DIRECTION('center_axis',(0.,0.,1.));
#17425=DIRECTION('ref_axis',(-1.,-1.05902768135554E-13,0.));
#17426=DIRECTION('',(-1.22464679914735E-16,-1.29843461996317E-29,1.));
#17427=DIRECTION('center_axis',(0.,0.,1.));
#17428=DIRECTION('ref_axis',(0.609342756385647,-0.792906933530248,0.));
#17429=DIRECTION('',(-1.22464679914735E-16,-1.29843461996317E-29,1.));
#17430=DIRECTION('center_axis',(0.,0.,1.));
#17431=DIRECTION('ref_axis',(-1.,-1.05902768135554E-13,0.));
#17432=DIRECTION('center_axis',(0.,0.,1.));
#17433=DIRECTION('ref_axis',(-1.,0.,0.));
#17434=DIRECTION('',(0.,0.,1.));
#17435=DIRECTION('center_axis',(0.,0.,-1.));
#17436=DIRECTION('ref_axis',(-1.,0.,0.));
#17437=DIRECTION('',(0.,0.,1.));
#17438=DIRECTION('center_axis',(0.,0.,-1.));
#17439=DIRECTION('ref_axis',(-1.,0.,0.));
#17440=DIRECTION('center_axis',(0.,0.,-1.));
#17441=DIRECTION('ref_axis',(-1.,0.,0.));
#17442=DIRECTION('center_axis',(0.,0.,1.));
#17443=DIRECTION('ref_axis',(-1.,0.,0.));
#17444=DIRECTION('',(0.,0.,1.));
#17445=DIRECTION('center_axis',(0.,0.,1.));
#17446=DIRECTION('ref_axis',(-1.,0.,0.));
#17447=DIRECTION('',(0.,0.,1.));
#17448=DIRECTION('center_axis',(0.,0.,1.));
#17449=DIRECTION('ref_axis',(-1.,0.,0.));
#17450=DIRECTION('',(0.,0.,1.));
#17451=DIRECTION('center_axis',(0.,0.,1.));
#17452=DIRECTION('ref_axis',(-1.,0.,0.));
#17453=DIRECTION('',(0.,0.,1.));
#17454=DIRECTION('center_axis',(0.,0.,1.));
#17455=DIRECTION('ref_axis',(-1.,0.,0.));
#17456=DIRECTION('',(0.,0.,1.));
#17457=DIRECTION('center_axis',(0.,0.,1.));
#17458=DIRECTION('ref_axis',(-1.,0.,0.));
#17459=DIRECTION('',(0.,0.,1.));
#17460=DIRECTION('center_axis',(0.,0.,1.));
#17461=DIRECTION('ref_axis',(-1.,0.,0.));
#17462=DIRECTION('',(0.,0.,1.));
#17463=DIRECTION('center_axis',(0.,0.,1.));
#17464=DIRECTION('ref_axis',(-1.,0.,0.));
#17465=DIRECTION('',(0.,0.,1.));
#17466=DIRECTION('center_axis',(0.,0.,1.));
#17467=DIRECTION('ref_axis',(-1.,0.,0.));
#17468=DIRECTION('',(0.,0.,1.));
#17469=DIRECTION('center_axis',(0.,0.,1.));
#17470=DIRECTION('ref_axis',(-1.,0.,0.));
#17471=DIRECTION('',(0.,0.,1.));
#17472=DIRECTION('center_axis',(0.,0.,1.));
#17473=DIRECTION('ref_axis',(-1.,0.,0.));
#17474=DIRECTION('',(0.,0.,1.));
#17475=DIRECTION('center_axis',(0.,0.,1.));
#17476=DIRECTION('ref_axis',(-1.,0.,0.));
#17477=DIRECTION('',(0.,0.,1.));
#17478=DIRECTION('center_axis',(0.,0.,1.));
#17479=DIRECTION('ref_axis',(-1.,0.,0.));
#17480=DIRECTION('',(0.,0.,1.));
#17481=DIRECTION('center_axis',(0.,0.,1.));
#17482=DIRECTION('ref_axis',(-1.,0.,0.));
#17483=DIRECTION('',(0.,0.,1.));
#17484=DIRECTION('center_axis',(0.,0.,1.));
#17485=DIRECTION('ref_axis',(-1.,0.,0.));
#17486=DIRECTION('',(0.,0.,1.));
#17487=DIRECTION('center_axis',(0.,0.,1.));
#17488=DIRECTION('ref_axis',(-1.,0.,0.));
#17489=DIRECTION('',(0.,0.,1.));
#17490=DIRECTION('center_axis',(0.,0.,1.));
#17491=DIRECTION('ref_axis',(-0.938438098661675,-0.345447441704612,0.));
#17492=DIRECTION('',(0.,0.,1.));
#17493=DIRECTION('center_axis',(0.,0.,-1.));
#17494=DIRECTION('ref_axis',(-1.,0.,0.));
#17495=DIRECTION('center_axis',(0.,0.,1.));
#17496=DIRECTION('ref_axis',(0.417701952176177,0.908584106810267,0.));
#17497=DIRECTION('',(-1.22464679914735E-16,-1.29843461996317E-29,1.));
#17498=DIRECTION('center_axis',(0.,0.,-1.));
#17499=DIRECTION('ref_axis',(-1.,-1.05902768135554E-13,0.));
#17500=DIRECTION('center_axis',(0.,0.,1.));
#17501=DIRECTION('ref_axis',(-1.,-1.05902768135554E-13,0.));
#17502=DIRECTION('',(-1.22464679914735E-16,-1.29843461996317E-29,1.));
#17503=DIRECTION('center_axis',(0.,0.,1.));
#17504=DIRECTION('ref_axis',(-1.,-1.05902768135554E-13,0.));
#17505=DIRECTION('',(-1.22464679914735E-16,-1.29843461996317E-29,1.));
#17506=DIRECTION('center_axis',(0.,0.,1.));
#17507=DIRECTION('ref_axis',(-1.,-1.05902768135554E-13,0.));
#17508=DIRECTION('',(-1.22464679914735E-16,-1.29843461996317E-29,1.));
#17509=DIRECTION('center_axis',(0.,0.,1.));
#17510=DIRECTION('ref_axis',(-1.,-1.05902768135554E-13,0.));
#17511=DIRECTION('',(-1.22464679914735E-16,-1.29843461996317E-29,1.));
#17512=DIRECTION('center_axis',(0.,0.,1.));
#17513=DIRECTION('ref_axis',(-1.,-1.05902768135554E-13,0.));
#17514=DIRECTION('',(-1.22464679914735E-16,-1.29843461996317E-29,1.));
#17515=DIRECTION('center_axis',(0.,0.,1.));
#17516=DIRECTION('ref_axis',(-1.,-1.05902768135554E-13,0.));
#17517=DIRECTION('',(-1.22464679914735E-16,-1.29843461996317E-29,1.));
#17518=DIRECTION('center_axis',(0.,0.,1.));
#17519=DIRECTION('ref_axis',(-1.,-1.05902768135554E-13,0.));
#17520=DIRECTION('',(-1.22464679914735E-16,-1.29843461996317E-29,1.));
#17521=DIRECTION('center_axis',(0.,0.,1.));
#17522=DIRECTION('ref_axis',(-1.,-1.05902768135554E-13,0.));
#17523=DIRECTION('',(-1.22464679914735E-16,-1.29843461996317E-29,1.));
#17524=DIRECTION('center_axis',(0.,0.,1.));
#17525=DIRECTION('ref_axis',(-1.,-1.05902768135554E-13,0.));
#17526=DIRECTION('',(-1.22464679914735E-16,-1.29843461996317E-29,1.));
#17527=DIRECTION('center_axis',(0.,0.,1.));
#17528=DIRECTION('ref_axis',(-1.,-1.05902768135554E-13,0.));
#17529=DIRECTION('',(-1.22464679914735E-16,-1.29843461996317E-29,1.));
#17530=DIRECTION('center_axis',(0.,0.,1.));
#17531=DIRECTION('ref_axis',(-1.,-1.05902768135554E-13,0.));
#17532=DIRECTION('',(-1.22464679914735E-16,-1.29843461996317E-29,1.));
#17533=DIRECTION('center_axis',(0.,0.,1.));
#17534=DIRECTION('ref_axis',(-1.,-1.05902768135554E-13,0.));
#17535=DIRECTION('',(-1.22464679914735E-16,-1.29843461996317E-29,1.));
#17536=DIRECTION('center_axis',(0.,0.,1.));
#17537=DIRECTION('ref_axis',(-1.,-1.05902768135554E-13,0.));
#17538=DIRECTION('',(-1.22464679914735E-16,-1.29843461996317E-29,1.));
#17539=DIRECTION('center_axis',(0.,0.,1.));
#17540=DIRECTION('ref_axis',(-1.,-1.05902768135554E-13,0.));
#17541=DIRECTION('',(-1.22464679914735E-16,-1.29843461996317E-29,1.));
#17542=DIRECTION('center_axis',(0.,0.,1.));
#17543=DIRECTION('ref_axis',(-1.,-1.05902768135554E-13,0.));
#17544=DIRECTION('',(-1.22464679914735E-16,-1.29843461996317E-29,1.));
#17545=DIRECTION('center_axis',(0.,0.,1.));
#17546=DIRECTION('ref_axis',(-1.,-1.05902768135554E-13,0.));
#17547=DIRECTION('',(-1.22464679914735E-16,-1.29843461996317E-29,1.));
#17548=DIRECTION('center_axis',(0.,0.,1.));
#17549=DIRECTION('ref_axis',(-1.,-1.05902768135554E-13,0.));
#17550=DIRECTION('',(-1.22464679914735E-16,-1.29843461996317E-29,1.));
#17551=DIRECTION('center_axis',(0.,0.,1.));
#17552=DIRECTION('ref_axis',(0.609342754269626,-0.792906935156394,0.));
#17553=DIRECTION('',(-1.22464679914735E-16,-1.29843461996317E-29,1.));
#17554=DIRECTION('center_axis',(0.,0.,1.));
#17555=DIRECTION('ref_axis',(-1.,-1.05902768135554E-13,0.));
#17556=DIRECTION('center_axis',(0.,0.,-1.));
#17557=DIRECTION('ref_axis',(1.,0.,0.));
#17558=DIRECTION('',(0.,0.,-1.));
#17559=DIRECTION('center_axis',(0.,0.,1.));
#17560=DIRECTION('ref_axis',(1.,0.,0.));
#17561=DIRECTION('',(0.,0.,-1.));
#17562=DIRECTION('center_axis',(0.,0.,1.));
#17563=DIRECTION('ref_axis',(1.,0.,0.));
#17564=DIRECTION('center_axis',(0.,0.,1.));
#17565=DIRECTION('ref_axis',(1.,0.,0.));
#17566=DIRECTION('center_axis',(0.,0.,-1.));
#17567=DIRECTION('ref_axis',(1.,0.,0.));
#17568=DIRECTION('',(0.,0.,-1.));
#17569=DIRECTION('center_axis',(0.,0.,-1.));
#17570=DIRECTION('ref_axis',(1.,0.,0.));
#17571=DIRECTION('',(0.,0.,-1.));
#17572=DIRECTION('center_axis',(0.,0.,-1.));
#17573=DIRECTION('ref_axis',(1.,0.,0.));
#17574=DIRECTION('',(0.,0.,-1.));
#17575=DIRECTION('center_axis',(0.,0.,-1.));
#17576=DIRECTION('ref_axis',(1.,0.,0.));
#17577=DIRECTION('',(0.,0.,-1.));
#17578=DIRECTION('center_axis',(0.,0.,-1.));
#17579=DIRECTION('ref_axis',(1.,0.,0.));
#17580=DIRECTION('',(0.,0.,-1.));
#17581=DIRECTION('center_axis',(0.,0.,-1.));
#17582=DIRECTION('ref_axis',(1.,0.,0.));
#17583=DIRECTION('',(0.,0.,-1.));
#17584=DIRECTION('center_axis',(0.,0.,-1.));
#17585=DIRECTION('ref_axis',(1.,0.,0.));
#17586=DIRECTION('',(0.,0.,-1.));
#17587=DIRECTION('center_axis',(0.,0.,-1.));
#17588=DIRECTION('ref_axis',(1.,0.,0.));
#17589=DIRECTION('',(0.,0.,-1.));
#17590=DIRECTION('center_axis',(0.,0.,-1.));
#17591=DIRECTION('ref_axis',(1.,0.,0.));
#17592=DIRECTION('',(0.,0.,-1.));
#17593=DIRECTION('center_axis',(0.,0.,-1.));
#17594=DIRECTION('ref_axis',(1.,0.,0.));
#17595=DIRECTION('',(0.,0.,-1.));
#17596=DIRECTION('center_axis',(0.,0.,-1.));
#17597=DIRECTION('ref_axis',(1.,0.,0.));
#17598=DIRECTION('',(0.,0.,-1.));
#17599=DIRECTION('center_axis',(0.,0.,-1.));
#17600=DIRECTION('ref_axis',(1.,0.,0.));
#17601=DIRECTION('',(0.,0.,-1.));
#17602=DIRECTION('center_axis',(0.,0.,-1.));
#17603=DIRECTION('ref_axis',(1.,0.,0.));
#17604=DIRECTION('',(0.,0.,-1.));
#17605=DIRECTION('center_axis',(0.,0.,-1.));
#17606=DIRECTION('ref_axis',(1.,0.,0.));
#17607=DIRECTION('',(0.,0.,-1.));
#17608=DIRECTION('center_axis',(0.,0.,-1.));
#17609=DIRECTION('ref_axis',(1.,0.,0.));
#17610=DIRECTION('',(0.,0.,-1.));
#17611=DIRECTION('center_axis',(0.,0.,-1.));
#17612=DIRECTION('ref_axis',(1.,0.,0.));
#17613=DIRECTION('',(0.,0.,-1.));
#17614=DIRECTION('center_axis',(0.,0.,-1.));
#17615=DIRECTION('ref_axis',(0.938439812457555,-0.345442785993033,0.));
#17616=DIRECTION('',(0.,0.,-1.));
#17617=DIRECTION('center_axis',(0.,0.,-1.));
#17618=DIRECTION('ref_axis',(1.,0.,0.));
#17619=DIRECTION('center_axis',(0.,0.,-1.));
#17620=DIRECTION('ref_axis',(-0.41770183671358,0.908584159891698,0.));
#17621=DIRECTION('',(1.22464679914735E-16,-1.35137073670524E-29,-1.));
#17622=DIRECTION('center_axis',(0.,0.,1.));
#17623=DIRECTION('ref_axis',(1.,-1.10225330100271E-13,0.));
#17624=DIRECTION('center_axis',(0.,0.,-1.));
#17625=DIRECTION('ref_axis',(1.,-1.10225330100271E-13,0.));
#17626=DIRECTION('',(1.22464679914735E-16,-1.35137073670524E-29,-1.));
#17627=DIRECTION('center_axis',(0.,0.,-1.));
#17628=DIRECTION('ref_axis',(1.,-1.10225330100271E-13,0.));
#17629=DIRECTION('',(1.22464679914735E-16,-1.35137073670524E-29,-1.));
#17630=DIRECTION('center_axis',(0.,0.,-1.));
#17631=DIRECTION('ref_axis',(1.,-1.10225330100271E-13,0.));
#17632=DIRECTION('',(1.22464679914735E-16,-1.35137073670524E-29,-1.));
#17633=DIRECTION('center_axis',(0.,0.,-1.));
#17634=DIRECTION('ref_axis',(1.,-1.10225330100271E-13,0.));
#17635=DIRECTION('',(1.22464679914735E-16,-1.35137073670524E-29,-1.));
#17636=DIRECTION('center_axis',(0.,0.,-1.));
#17637=DIRECTION('ref_axis',(1.,-1.10225330100271E-13,0.));
#17638=DIRECTION('',(1.22464679914735E-16,-1.35137073670524E-29,-1.));
#17639=DIRECTION('center_axis',(0.,0.,-1.));
#17640=DIRECTION('ref_axis',(1.,-1.10225330100271E-13,0.));
#17641=DIRECTION('',(1.22464679914735E-16,-1.35137073670524E-29,-1.));
#17642=DIRECTION('center_axis',(0.,0.,-1.));
#17643=DIRECTION('ref_axis',(1.,-1.10225330100271E-13,0.));
#17644=DIRECTION('',(1.22464679914735E-16,-1.35137073670524E-29,-1.));
#17645=DIRECTION('center_axis',(0.,0.,-1.));
#17646=DIRECTION('ref_axis',(1.,-1.10225330100271E-13,0.));
#17647=DIRECTION('',(1.22464679914735E-16,-1.35137073670524E-29,-1.));
#17648=DIRECTION('center_axis',(0.,0.,-1.));
#17649=DIRECTION('ref_axis',(1.,-1.10225330100271E-13,0.));
#17650=DIRECTION('',(1.22464679914735E-16,-1.35137073670524E-29,-1.));
#17651=DIRECTION('center_axis',(0.,0.,-1.));
#17652=DIRECTION('ref_axis',(1.,-1.10225330100271E-13,0.));
#17653=DIRECTION('',(1.22464679914735E-16,-1.35137073670524E-29,-1.));
#17654=DIRECTION('center_axis',(0.,0.,-1.));
#17655=DIRECTION('ref_axis',(1.,-1.10225330100271E-13,0.));
#17656=DIRECTION('',(1.22464679914735E-16,-1.35137073670524E-29,-1.));
#17657=DIRECTION('center_axis',(0.,0.,-1.));
#17658=DIRECTION('ref_axis',(1.,-1.10225330100271E-13,0.));
#17659=DIRECTION('',(1.22464679914735E-16,-1.35137073670524E-29,-1.));
#17660=DIRECTION('center_axis',(0.,0.,-1.));
#17661=DIRECTION('ref_axis',(1.,-1.10225330100271E-13,0.));
#17662=DIRECTION('',(1.22464679914735E-16,-1.35137073670524E-29,-1.));
#17663=DIRECTION('center_axis',(0.,0.,-1.));
#17664=DIRECTION('ref_axis',(1.,-1.10225330100271E-13,0.));
#17665=DIRECTION('',(1.22464679914735E-16,-1.35137073670524E-29,-1.));
#17666=DIRECTION('center_axis',(0.,0.,-1.));
#17667=DIRECTION('ref_axis',(1.,-1.10225330100271E-13,0.));
#17668=DIRECTION('',(1.22464679914735E-16,-1.35137073670524E-29,-1.));
#17669=DIRECTION('center_axis',(0.,0.,-1.));
#17670=DIRECTION('ref_axis',(1.,-1.10225330100271E-13,0.));
#17671=DIRECTION('',(1.22464679914735E-16,-1.35137073670524E-29,-1.));
#17672=DIRECTION('center_axis',(0.,0.,-1.));
#17673=DIRECTION('ref_axis',(1.,-1.10225330100271E-13,0.));
#17674=DIRECTION('',(1.22464679914735E-16,-1.35137073670524E-29,-1.));
#17675=DIRECTION('center_axis',(0.,0.,-1.));
#17676=DIRECTION('ref_axis',(-0.609338757688317,-0.792910006481731,0.));
#17677=DIRECTION('',(1.22464679914735E-16,-1.35137073670524E-29,-1.));
#17678=DIRECTION('center_axis',(0.,0.,-1.));
#17679=DIRECTION('ref_axis',(1.,-1.10225330100271E-13,0.));
#17680=DIRECTION('center_axis',(0.,0.,-1.));
#17681=DIRECTION('ref_axis',(1.,0.,0.));
#17682=DIRECTION('',(0.,0.,-1.));
#17683=DIRECTION('center_axis',(0.,0.,1.));
#17684=DIRECTION('ref_axis',(1.,0.,0.));
#17685=DIRECTION('',(0.,0.,-1.));
#17686=DIRECTION('center_axis',(0.,0.,1.));
#17687=DIRECTION('ref_axis',(1.,0.,0.));
#17688=DIRECTION('center_axis',(0.,0.,1.));
#17689=DIRECTION('ref_axis',(1.,0.,0.));
#17690=DIRECTION('center_axis',(0.,0.,-1.));
#17691=DIRECTION('ref_axis',(1.,0.,0.));
#17692=DIRECTION('',(0.,0.,-1.));
#17693=DIRECTION('center_axis',(0.,0.,-1.));
#17694=DIRECTION('ref_axis',(1.,0.,0.));
#17695=DIRECTION('',(0.,0.,-1.));
#17696=DIRECTION('center_axis',(0.,0.,-1.));
#17697=DIRECTION('ref_axis',(1.,0.,0.));
#17698=DIRECTION('',(0.,0.,-1.));
#17699=DIRECTION('center_axis',(0.,0.,-1.));
#17700=DIRECTION('ref_axis',(1.,0.,0.));
#17701=DIRECTION('',(0.,0.,-1.));
#17702=DIRECTION('center_axis',(0.,0.,-1.));
#17703=DIRECTION('ref_axis',(1.,0.,0.));
#17704=DIRECTION('',(0.,0.,-1.));
#17705=DIRECTION('center_axis',(0.,0.,-1.));
#17706=DIRECTION('ref_axis',(1.,0.,0.));
#17707=DIRECTION('',(0.,0.,-1.));
#17708=DIRECTION('center_axis',(0.,0.,-1.));
#17709=DIRECTION('ref_axis',(1.,0.,0.));
#17710=DIRECTION('',(0.,0.,-1.));
#17711=DIRECTION('center_axis',(0.,0.,-1.));
#17712=DIRECTION('ref_axis',(1.,0.,0.));
#17713=DIRECTION('',(0.,0.,-1.));
#17714=DIRECTION('center_axis',(0.,0.,-1.));
#17715=DIRECTION('ref_axis',(1.,0.,0.));
#17716=DIRECTION('',(0.,0.,-1.));
#17717=DIRECTION('center_axis',(0.,0.,-1.));
#17718=DIRECTION('ref_axis',(1.,0.,0.));
#17719=DIRECTION('',(0.,0.,-1.));
#17720=DIRECTION('center_axis',(0.,0.,-1.));
#17721=DIRECTION('ref_axis',(1.,0.,0.));
#17722=DIRECTION('',(0.,0.,-1.));
#17723=DIRECTION('center_axis',(0.,0.,-1.));
#17724=DIRECTION('ref_axis',(1.,0.,0.));
#17725=DIRECTION('',(0.,0.,-1.));
#17726=DIRECTION('center_axis',(0.,0.,-1.));
#17727=DIRECTION('ref_axis',(1.,0.,0.));
#17728=DIRECTION('',(0.,0.,-1.));
#17729=DIRECTION('center_axis',(0.,0.,-1.));
#17730=DIRECTION('ref_axis',(1.,0.,0.));
#17731=DIRECTION('',(0.,0.,-1.));
#17732=DIRECTION('center_axis',(0.,0.,-1.));
#17733=DIRECTION('ref_axis',(1.,0.,0.));
#17734=DIRECTION('',(0.,0.,-1.));
#17735=DIRECTION('center_axis',(0.,0.,-1.));
#17736=DIRECTION('ref_axis',(1.,0.,0.));
#17737=DIRECTION('',(0.,0.,-1.));
#17738=DIRECTION('center_axis',(0.,0.,-1.));
#17739=DIRECTION('ref_axis',(0.938439817930616,-0.345442771124758,0.));
#17740=DIRECTION('',(0.,0.,-1.));
#17741=DIRECTION('center_axis',(0.,0.,-1.));
#17742=DIRECTION('ref_axis',(1.,0.,0.));
#17743=DIRECTION('center_axis',(0.,0.,-1.));
#17744=DIRECTION('ref_axis',(-0.417701801892756,0.908584175899815,0.));
#17745=DIRECTION('',(1.22464679914735E-16,-1.37783879507626E-29,-1.));
#17746=DIRECTION('center_axis',(0.,0.,1.));
#17747=DIRECTION('ref_axis',(1.,-1.12386611082629E-13,0.));
#17748=DIRECTION('center_axis',(0.,0.,-1.));
#17749=DIRECTION('ref_axis',(1.,-1.12386611082629E-13,0.));
#17750=DIRECTION('',(1.22464679914735E-16,-1.37783879507626E-29,-1.));
#17751=DIRECTION('center_axis',(0.,0.,-1.));
#17752=DIRECTION('ref_axis',(1.,-1.12386611082629E-13,0.));
#17753=DIRECTION('',(1.22464679914735E-16,-1.37783879507626E-29,-1.));
#17754=DIRECTION('center_axis',(0.,0.,-1.));
#17755=DIRECTION('ref_axis',(1.,-1.12386611082629E-13,0.));
#17756=DIRECTION('',(1.22464679914735E-16,-1.37783879507626E-29,-1.));
#17757=DIRECTION('center_axis',(0.,0.,-1.));
#17758=DIRECTION('ref_axis',(1.,-1.12386611082629E-13,0.));
#17759=DIRECTION('',(1.22464679914735E-16,-1.37783879507626E-29,-1.));
#17760=DIRECTION('center_axis',(0.,0.,-1.));
#17761=DIRECTION('ref_axis',(1.,-1.12386611082629E-13,0.));
#17762=DIRECTION('',(1.22464679914735E-16,-1.37783879507626E-29,-1.));
#17763=DIRECTION('center_axis',(0.,0.,-1.));
#17764=DIRECTION('ref_axis',(1.,-1.12386611082629E-13,0.));
#17765=DIRECTION('',(1.22464679914735E-16,-1.37783879507626E-29,-1.));
#17766=DIRECTION('center_axis',(0.,0.,-1.));
#17767=DIRECTION('ref_axis',(1.,-1.12386611082629E-13,0.));
#17768=DIRECTION('',(1.22464679914735E-16,-1.37783879507626E-29,-1.));
#17769=DIRECTION('center_axis',(0.,0.,-1.));
#17770=DIRECTION('ref_axis',(1.,-1.12386611082629E-13,0.));
#17771=DIRECTION('',(1.22464679914735E-16,-1.37783879507626E-29,-1.));
#17772=DIRECTION('center_axis',(0.,0.,-1.));
#17773=DIRECTION('ref_axis',(1.,-1.12386611082629E-13,0.));
#17774=DIRECTION('',(1.22464679914735E-16,-1.37783879507626E-29,-1.));
#17775=DIRECTION('center_axis',(0.,0.,-1.));
#17776=DIRECTION('ref_axis',(1.,-1.12386611082629E-13,0.));
#17777=DIRECTION('',(1.22464679914735E-16,-1.37783879507626E-29,-1.));
#17778=DIRECTION('center_axis',(0.,0.,-1.));
#17779=DIRECTION('ref_axis',(1.,-1.12386611082629E-13,0.));
#17780=DIRECTION('',(1.22464679914735E-16,-1.37783879507626E-29,-1.));
#17781=DIRECTION('center_axis',(0.,0.,-1.));
#17782=DIRECTION('ref_axis',(1.,-1.12386611082629E-13,0.));
#17783=DIRECTION('',(1.22464679914735E-16,-1.37783879507626E-29,-1.));
#17784=DIRECTION('center_axis',(0.,0.,-1.));
#17785=DIRECTION('ref_axis',(1.,-1.12386611082629E-13,0.));
#17786=DIRECTION('',(1.22464679914735E-16,-1.37783879507626E-29,-1.));
#17787=DIRECTION('center_axis',(0.,0.,-1.));
#17788=DIRECTION('ref_axis',(1.,-1.12386611082629E-13,0.));
#17789=DIRECTION('',(1.22464679914735E-16,-1.37783879507626E-29,-1.));
#17790=DIRECTION('center_axis',(0.,0.,-1.));
#17791=DIRECTION('ref_axis',(1.,-1.12386611082629E-13,0.));
#17792=DIRECTION('',(1.22464679914735E-16,-1.37783879507626E-29,-1.));
#17793=DIRECTION('center_axis',(0.,0.,-1.));
#17794=DIRECTION('ref_axis',(1.,-1.12386611082629E-13,0.));
#17795=DIRECTION('',(1.22464679914735E-16,-1.37783879507626E-29,-1.));
#17796=DIRECTION('center_axis',(0.,0.,-1.));
#17797=DIRECTION('ref_axis',(1.,-1.12386611082629E-13,0.));
#17798=DIRECTION('',(1.22464679914735E-16,-1.37783879507626E-29,-1.));
#17799=DIRECTION('center_axis',(0.,0.,-1.));
#17800=DIRECTION('ref_axis',(-0.609338761677812,-0.792910003415867,0.));
#17801=DIRECTION('',(1.22464679914735E-16,-1.37783879507626E-29,-1.));
#17802=DIRECTION('center_axis',(0.,0.,-1.));
#17803=DIRECTION('ref_axis',(1.,-1.12386611082629E-13,0.));
#17804=DIRECTION('center_axis',(0.,0.,-1.));
#17805=DIRECTION('ref_axis',(1.,0.,0.));
#17806=DIRECTION('',(0.,0.,-1.));
#17807=DIRECTION('center_axis',(0.,0.,1.));
#17808=DIRECTION('ref_axis',(1.,0.,0.));
#17809=DIRECTION('',(0.,0.,-1.));
#17810=DIRECTION('center_axis',(0.,0.,1.));
#17811=DIRECTION('ref_axis',(1.,0.,0.));
#17812=DIRECTION('center_axis',(0.,0.,1.));
#17813=DIRECTION('ref_axis',(1.,0.,0.));
#17814=DIRECTION('center_axis',(0.,0.,-1.));
#17815=DIRECTION('ref_axis',(1.,0.,0.));
#17816=DIRECTION('',(0.,0.,-1.));
#17817=DIRECTION('center_axis',(0.,0.,-1.));
#17818=DIRECTION('ref_axis',(1.,0.,0.));
#17819=DIRECTION('',(0.,0.,-1.));
#17820=DIRECTION('center_axis',(0.,0.,-1.));
#17821=DIRECTION('ref_axis',(1.,0.,0.));
#17822=DIRECTION('',(0.,0.,-1.));
#17823=DIRECTION('center_axis',(0.,0.,-1.));
#17824=DIRECTION('ref_axis',(1.,0.,0.));
#17825=DIRECTION('',(0.,0.,-1.));
#17826=DIRECTION('center_axis',(0.,0.,-1.));
#17827=DIRECTION('ref_axis',(1.,0.,0.));
#17828=DIRECTION('',(0.,0.,-1.));
#17829=DIRECTION('center_axis',(0.,0.,-1.));
#17830=DIRECTION('ref_axis',(1.,0.,0.));
#17831=DIRECTION('',(0.,0.,-1.));
#17832=DIRECTION('center_axis',(0.,0.,-1.));
#17833=DIRECTION('ref_axis',(1.,0.,0.));
#17834=DIRECTION('',(0.,0.,-1.));
#17835=DIRECTION('center_axis',(0.,0.,-1.));
#17836=DIRECTION('ref_axis',(1.,0.,0.));
#17837=DIRECTION('',(0.,0.,-1.));
#17838=DIRECTION('center_axis',(0.,0.,-1.));
#17839=DIRECTION('ref_axis',(1.,0.,0.));
#17840=DIRECTION('',(0.,0.,-1.));
#17841=DIRECTION('center_axis',(0.,0.,-1.));
#17842=DIRECTION('ref_axis',(1.,0.,0.));
#17843=DIRECTION('',(0.,0.,-1.));
#17844=DIRECTION('center_axis',(0.,0.,-1.));
#17845=DIRECTION('ref_axis',(1.,0.,0.));
#17846=DIRECTION('',(0.,0.,-1.));
#17847=DIRECTION('center_axis',(0.,0.,-1.));
#17848=DIRECTION('ref_axis',(1.,0.,0.));
#17849=DIRECTION('',(0.,0.,-1.));
#17850=DIRECTION('center_axis',(0.,0.,-1.));
#17851=DIRECTION('ref_axis',(1.,0.,0.));
#17852=DIRECTION('',(0.,0.,-1.));
#17853=DIRECTION('center_axis',(0.,0.,-1.));
#17854=DIRECTION('ref_axis',(1.,0.,0.));
#17855=DIRECTION('',(0.,0.,-1.));
#17856=DIRECTION('center_axis',(0.,0.,-1.));
#17857=DIRECTION('ref_axis',(1.,0.,0.));
#17858=DIRECTION('',(0.,0.,-1.));
#17859=DIRECTION('center_axis',(0.,0.,-1.));
#17860=DIRECTION('ref_axis',(1.,0.,0.));
#17861=DIRECTION('',(0.,0.,-1.));
#17862=DIRECTION('center_axis',(0.,0.,-1.));
#17863=DIRECTION('ref_axis',(0.938439818752348,-0.345442768892418,0.));
#17864=DIRECTION('',(0.,0.,-1.));
#17865=DIRECTION('center_axis',(0.,0.,-1.));
#17866=DIRECTION('ref_axis',(1.,0.,0.));
#17867=DIRECTION('center_axis',(0.,0.,-1.));
#17868=DIRECTION('ref_axis',(-0.4177018103935,0.908584171991783,0.));
#17869=DIRECTION('',(1.22464679914735E-16,-1.32490267833421E-29,-1.));
#17870=DIRECTION('center_axis',(0.,0.,1.));
#17871=DIRECTION('ref_axis',(1.,-1.08064049117913E-13,0.));
#17872=DIRECTION('center_axis',(0.,0.,-1.));
#17873=DIRECTION('ref_axis',(1.,-1.08064049117913E-13,0.));
#17874=DIRECTION('',(1.22464679914735E-16,-1.32490267833421E-29,-1.));
#17875=DIRECTION('center_axis',(0.,0.,-1.));
#17876=DIRECTION('ref_axis',(1.,-1.08064049117913E-13,0.));
#17877=DIRECTION('',(1.22464679914735E-16,-1.32490267833421E-29,-1.));
#17878=DIRECTION('center_axis',(0.,0.,-1.));
#17879=DIRECTION('ref_axis',(1.,-1.08064049117913E-13,0.));
#17880=DIRECTION('',(1.22464679914735E-16,-1.32490267833421E-29,-1.));
#17881=DIRECTION('center_axis',(0.,0.,-1.));
#17882=DIRECTION('ref_axis',(1.,-1.08064049117913E-13,0.));
#17883=DIRECTION('',(1.22464679914735E-16,-1.32490267833421E-29,-1.));
#17884=DIRECTION('center_axis',(0.,0.,-1.));
#17885=DIRECTION('ref_axis',(1.,-1.08064049117913E-13,0.));
#17886=DIRECTION('',(1.22464679914735E-16,-1.32490267833421E-29,-1.));
#17887=DIRECTION('center_axis',(0.,0.,-1.));
#17888=DIRECTION('ref_axis',(1.,-1.08064049117913E-13,0.));
#17889=DIRECTION('',(1.22464679914735E-16,-1.32490267833421E-29,-1.));
#17890=DIRECTION('center_axis',(0.,0.,-1.));
#17891=DIRECTION('ref_axis',(1.,-1.08064049117913E-13,0.));
#17892=DIRECTION('',(1.22464679914735E-16,-1.32490267833421E-29,-1.));
#17893=DIRECTION('center_axis',(0.,0.,-1.));
#17894=DIRECTION('ref_axis',(1.,-1.08064049117913E-13,0.));
#17895=DIRECTION('',(1.22464679914735E-16,-1.32490267833421E-29,-1.));
#17896=DIRECTION('center_axis',(0.,0.,-1.));
#17897=DIRECTION('ref_axis',(1.,-1.08064049117913E-13,0.));
#17898=DIRECTION('',(1.22464679914735E-16,-1.32490267833421E-29,-1.));
#17899=DIRECTION('center_axis',(0.,0.,-1.));
#17900=DIRECTION('ref_axis',(1.,-1.08064049117913E-13,0.));
#17901=DIRECTION('',(1.22464679914735E-16,-1.32490267833421E-29,-1.));
#17902=DIRECTION('center_axis',(0.,0.,-1.));
#17903=DIRECTION('ref_axis',(1.,-1.08064049117913E-13,0.));
#17904=DIRECTION('',(1.22464679914735E-16,-1.32490267833421E-29,-1.));
#17905=DIRECTION('center_axis',(0.,0.,-1.));
#17906=DIRECTION('ref_axis',(1.,-1.08064049117913E-13,0.));
#17907=DIRECTION('',(1.22464679914735E-16,-1.32490267833421E-29,-1.));
#17908=DIRECTION('center_axis',(0.,0.,-1.));
#17909=DIRECTION('ref_axis',(1.,-1.08064049117913E-13,0.));
#17910=DIRECTION('',(1.22464679914735E-16,-1.32490267833421E-29,-1.));
#17911=DIRECTION('center_axis',(0.,0.,-1.));
#17912=DIRECTION('ref_axis',(1.,-1.08064049117913E-13,0.));
#17913=DIRECTION('',(1.22464679914735E-16,-1.32490267833421E-29,-1.));
#17914=DIRECTION('center_axis',(0.,0.,-1.));
#17915=DIRECTION('ref_axis',(1.,-1.08064049117913E-13,0.));
#17916=DIRECTION('',(1.22464679914735E-16,-1.32490267833421E-29,-1.));
#17917=DIRECTION('center_axis',(0.,0.,-1.));
#17918=DIRECTION('ref_axis',(1.,-1.08064049117913E-13,0.));
#17919=DIRECTION('',(1.22464679914735E-16,-1.32490267833421E-29,-1.));
#17920=DIRECTION('center_axis',(0.,0.,-1.));
#17921=DIRECTION('ref_axis',(1.,-1.08064049117913E-13,0.));
#17922=DIRECTION('',(1.22464679914735E-16,-1.32490267833421E-29,-1.));
#17923=DIRECTION('center_axis',(0.,0.,-1.));
#17924=DIRECTION('ref_axis',(-0.609338759590107,-0.792910005020235,0.));
#17925=DIRECTION('',(1.22464679914735E-16,-1.32490267833421E-29,-1.));
#17926=DIRECTION('center_axis',(0.,0.,-1.));
#17927=DIRECTION('ref_axis',(1.,-1.08064049117913E-13,0.));
#17928=DIRECTION('center_axis',(0.,0.,-1.));
#17929=DIRECTION('ref_axis',(1.,0.,0.));
#17930=DIRECTION('',(0.,0.,-1.));
#17931=DIRECTION('center_axis',(0.,0.,1.));
#17932=DIRECTION('ref_axis',(1.,0.,0.));
#17933=DIRECTION('',(0.,0.,-1.));
#17934=DIRECTION('center_axis',(0.,0.,1.));
#17935=DIRECTION('ref_axis',(1.,0.,0.));
#17936=DIRECTION('center_axis',(0.,0.,1.));
#17937=DIRECTION('ref_axis',(1.,0.,0.));
#17938=DIRECTION('center_axis',(0.,0.,-1.));
#17939=DIRECTION('ref_axis',(1.,0.,0.));
#17940=DIRECTION('',(0.,0.,-1.));
#17941=DIRECTION('center_axis',(0.,0.,-1.));
#17942=DIRECTION('ref_axis',(1.,0.,0.));
#17943=DIRECTION('',(0.,0.,-1.));
#17944=DIRECTION('center_axis',(0.,0.,-1.));
#17945=DIRECTION('ref_axis',(1.,0.,0.));
#17946=DIRECTION('',(0.,0.,-1.));
#17947=DIRECTION('center_axis',(0.,0.,-1.));
#17948=DIRECTION('ref_axis',(1.,0.,0.));
#17949=DIRECTION('',(0.,0.,-1.));
#17950=DIRECTION('center_axis',(0.,0.,-1.));
#17951=DIRECTION('ref_axis',(1.,0.,0.));
#17952=DIRECTION('',(0.,0.,-1.));
#17953=DIRECTION('center_axis',(0.,0.,-1.));
#17954=DIRECTION('ref_axis',(1.,0.,0.));
#17955=DIRECTION('',(0.,0.,-1.));
#17956=DIRECTION('center_axis',(0.,0.,-1.));
#17957=DIRECTION('ref_axis',(1.,0.,0.));
#17958=DIRECTION('',(0.,0.,-1.));
#17959=DIRECTION('center_axis',(0.,0.,-1.));
#17960=DIRECTION('ref_axis',(1.,0.,0.));
#17961=DIRECTION('',(0.,0.,-1.));
#17962=DIRECTION('center_axis',(0.,0.,-1.));
#17963=DIRECTION('ref_axis',(1.,0.,0.));
#17964=DIRECTION('',(0.,0.,-1.));
#17965=DIRECTION('center_axis',(0.,0.,-1.));
#17966=DIRECTION('ref_axis',(1.,0.,0.));
#17967=DIRECTION('',(0.,0.,-1.));
#17968=DIRECTION('center_axis',(0.,0.,-1.));
#17969=DIRECTION('ref_axis',(1.,0.,0.));
#17970=DIRECTION('',(0.,0.,-1.));
#17971=DIRECTION('center_axis',(0.,0.,-1.));
#17972=DIRECTION('ref_axis',(1.,0.,0.));
#17973=DIRECTION('',(0.,0.,-1.));
#17974=DIRECTION('center_axis',(0.,0.,-1.));
#17975=DIRECTION('ref_axis',(1.,0.,0.));
#17976=DIRECTION('',(0.,0.,-1.));
#17977=DIRECTION('center_axis',(0.,0.,-1.));
#17978=DIRECTION('ref_axis',(1.,0.,0.));
#17979=DIRECTION('',(0.,0.,-1.));
#17980=DIRECTION('center_axis',(0.,0.,-1.));
#17981=DIRECTION('ref_axis',(1.,0.,0.));
#17982=DIRECTION('',(0.,0.,-1.));
#17983=DIRECTION('center_axis',(0.,0.,-1.));
#17984=DIRECTION('ref_axis',(1.,0.,0.));
#17985=DIRECTION('',(0.,0.,-1.));
#17986=DIRECTION('center_axis',(0.,0.,-1.));
#17987=DIRECTION('ref_axis',(0.93843981373604,-0.345442782519866,0.));
#17988=DIRECTION('',(0.,0.,-1.));
#17989=DIRECTION('center_axis',(0.,0.,-1.));
#17990=DIRECTION('ref_axis',(1.,0.,0.));
#17991=DIRECTION('center_axis',(0.,0.,-1.));
#17992=DIRECTION('ref_axis',(-0.417701842212249,0.908584157363804,0.));
#17993=DIRECTION('',(1.22464679914735E-16,-1.40430685344729E-29,-1.));
#17994=DIRECTION('center_axis',(0.,0.,1.));
#17995=DIRECTION('ref_axis',(1.,-1.14547892064987E-13,0.));
#17996=DIRECTION('center_axis',(0.,0.,-1.));
#17997=DIRECTION('ref_axis',(1.,-1.14547892064987E-13,0.));
#17998=DIRECTION('',(1.22464679914735E-16,-1.40430685344729E-29,-1.));
#17999=DIRECTION('center_axis',(0.,0.,-1.));
#18000=DIRECTION('ref_axis',(1.,-1.14547892064987E-13,0.));
#18001=DIRECTION('',(1.22464679914735E-16,-1.40430685344729E-29,-1.));
#18002=DIRECTION('center_axis',(0.,0.,-1.));
#18003=DIRECTION('ref_axis',(1.,-1.14547892064987E-13,0.));
#18004=DIRECTION('',(1.22464679914735E-16,-1.40430685344729E-29,-1.));
#18005=DIRECTION('center_axis',(0.,0.,-1.));
#18006=DIRECTION('ref_axis',(1.,-1.14547892064987E-13,0.));
#18007=DIRECTION('',(1.22464679914735E-16,-1.40430685344729E-29,-1.));
#18008=DIRECTION('center_axis',(0.,0.,-1.));
#18009=DIRECTION('ref_axis',(1.,-1.14547892064987E-13,0.));
#18010=DIRECTION('',(1.22464679914735E-16,-1.40430685344729E-29,-1.));
#18011=DIRECTION('center_axis',(0.,0.,-1.));
#18012=DIRECTION('ref_axis',(1.,-1.14547892064987E-13,0.));
#18013=DIRECTION('',(1.22464679914735E-16,-1.40430685344729E-29,-1.));
#18014=DIRECTION('center_axis',(0.,0.,-1.));
#18015=DIRECTION('ref_axis',(1.,-1.14547892064987E-13,0.));
#18016=DIRECTION('',(1.22464679914735E-16,-1.40430685344729E-29,-1.));
#18017=DIRECTION('center_axis',(0.,0.,-1.));
#18018=DIRECTION('ref_axis',(1.,-1.14547892064987E-13,0.));
#18019=DIRECTION('',(1.22464679914735E-16,-1.40430685344729E-29,-1.));
#18020=DIRECTION('center_axis',(0.,0.,-1.));
#18021=DIRECTION('ref_axis',(1.,-1.14547892064987E-13,0.));
#18022=DIRECTION('',(1.22464679914735E-16,-1.40430685344729E-29,-1.));
#18023=DIRECTION('center_axis',(0.,0.,-1.));
#18024=DIRECTION('ref_axis',(1.,-1.14547892064987E-13,0.));
#18025=DIRECTION('',(1.22464679914735E-16,-1.40430685344729E-29,-1.));
#18026=DIRECTION('center_axis',(0.,0.,-1.));
#18027=DIRECTION('ref_axis',(1.,-1.14547892064987E-13,0.));
#18028=DIRECTION('',(1.22464679914735E-16,-1.40430685344729E-29,-1.));
#18029=DIRECTION('center_axis',(0.,0.,-1.));
#18030=DIRECTION('ref_axis',(1.,-1.14547892064987E-13,0.));
#18031=DIRECTION('',(1.22464679914735E-16,-1.40430685344729E-29,-1.));
#18032=DIRECTION('center_axis',(0.,0.,-1.));
#18033=DIRECTION('ref_axis',(1.,-1.14547892064987E-13,0.));
#18034=DIRECTION('',(1.22464679914735E-16,-1.40430685344729E-29,-1.));
#18035=DIRECTION('center_axis',(0.,0.,-1.));
#18036=DIRECTION('ref_axis',(1.,-1.14547892064987E-13,0.));
#18037=DIRECTION('',(1.22464679914735E-16,-1.40430685344729E-29,-1.));
#18038=DIRECTION('center_axis',(0.,0.,-1.));
#18039=DIRECTION('ref_axis',(1.,-1.14547892064987E-13,0.));
#18040=DIRECTION('',(1.22464679914735E-16,-1.40430685344729E-29,-1.));
#18041=DIRECTION('center_axis',(0.,0.,-1.));
#18042=DIRECTION('ref_axis',(1.,-1.14547892064987E-13,0.));
#18043=DIRECTION('',(1.22464679914735E-16,-1.40430685344729E-29,-1.));
#18044=DIRECTION('center_axis',(0.,0.,-1.));
#18045=DIRECTION('ref_axis',(1.,-1.14547892064987E-13,0.));
#18046=DIRECTION('',(1.22464679914735E-16,-1.40430685344729E-29,-1.));
#18047=DIRECTION('center_axis',(0.,0.,-1.));
#18048=DIRECTION('ref_axis',(-0.609338755970259,-0.792910007802031,0.));
#18049=DIRECTION('',(1.22464679914735E-16,-1.40430685344729E-29,-1.));
#18050=DIRECTION('center_axis',(0.,0.,-1.));
#18051=DIRECTION('ref_axis',(1.,-1.14547892064987E-13,0.));
#18052=DIRECTION('center_axis',(0.,0.,1.));
#18053=DIRECTION('ref_axis',(1.,0.,0.));
#18054=DIRECTION('center_axis',(0.,0.,-1.));
#18055=DIRECTION('ref_axis',(1.,-1.14547892064987E-13,0.));
#18056=DIRECTION('center_axis',(0.,0.,-1.));
#18057=DIRECTION('ref_axis',(1.,0.,0.));
#18058=DIRECTION('center_axis',(0.,0.,1.));
#18059=DIRECTION('ref_axis',(1.,0.,0.));
#18060=DIRECTION('center_axis',(0.,0.,-1.));
#18061=DIRECTION('ref_axis',(1.,-1.08064049117913E-13,0.));
#18062=DIRECTION('center_axis',(0.,0.,-1.));
#18063=DIRECTION('ref_axis',(1.,0.,0.));
#18064=DIRECTION('center_axis',(0.,0.,1.));
#18065=DIRECTION('ref_axis',(1.,0.,0.));
#18066=DIRECTION('center_axis',(0.,0.,-1.));
#18067=DIRECTION('ref_axis',(1.,-1.12386611082629E-13,0.));
#18068=DIRECTION('center_axis',(0.,0.,-1.));
#18069=DIRECTION('ref_axis',(1.,0.,0.));
#18070=DIRECTION('center_axis',(0.,0.,1.));
#18071=DIRECTION('ref_axis',(1.,0.,0.));
#18072=DIRECTION('center_axis',(0.,0.,-1.));
#18073=DIRECTION('ref_axis',(1.,-1.10225330100271E-13,0.));
#18074=DIRECTION('center_axis',(0.,0.,-1.));
#18075=DIRECTION('ref_axis',(1.,0.,0.));
#18076=DIRECTION('center_axis',(0.,0.,-1.));
#18077=DIRECTION('ref_axis',(1.,0.,0.));
#18078=DIRECTION('center_axis',(0.,0.,-1.));
#18079=DIRECTION('ref_axis',(1.,0.,0.));
#18080=DIRECTION('center_axis',(0.,0.,-1.));
#18081=DIRECTION('ref_axis',(1.,0.,0.));
#18082=DIRECTION('center_axis',(0.,0.,-1.));
#18083=DIRECTION('ref_axis',(1.,0.,0.));
#18084=DIRECTION('center_axis',(0.,0.,1.));
#18085=DIRECTION('ref_axis',(1.,0.,0.));
#18086=DIRECTION('center_axis',(0.,0.,1.));
#18087=DIRECTION('ref_axis',(-1.,-1.05902768135554E-13,0.));
#18088=DIRECTION('center_axis',(0.,0.,1.));
#18089=DIRECTION('ref_axis',(-1.,0.,0.));
#18090=DIRECTION('center_axis',(0.,0.,1.));
#18091=DIRECTION('ref_axis',(1.,0.,0.));
#18092=DIRECTION('center_axis',(0.,0.,1.));
#18093=DIRECTION('ref_axis',(-1.,-1.05902768135554E-13,0.));
#18094=DIRECTION('center_axis',(0.,0.,1.));
#18095=DIRECTION('ref_axis',(-1.,0.,0.));
#18096=DIRECTION('center_axis',(0.,0.,1.));
#18097=DIRECTION('ref_axis',(1.,0.,0.));
#18098=DIRECTION('center_axis',(0.,0.,1.));
#18099=DIRECTION('ref_axis',(-1.,-1.05902768135554E-13,0.));
#18100=DIRECTION('center_axis',(0.,0.,1.));
#18101=DIRECTION('ref_axis',(-1.,0.,0.));
#18102=DIRECTION('center_axis',(0.,0.,1.));
#18103=DIRECTION('ref_axis',(1.,0.,0.));
#18104=DIRECTION('center_axis',(0.,0.,1.));
#18105=DIRECTION('ref_axis',(-1.,-1.01580206170838E-13,0.));
#18106=DIRECTION('center_axis',(0.,0.,1.));
#18107=DIRECTION('ref_axis',(-1.,0.,0.));
#18108=DIRECTION('center_axis',(0.,0.,1.));
#18109=DIRECTION('ref_axis',(-1.,0.,0.));
#18110=DIRECTION('center_axis',(0.,0.,1.));
#18111=DIRECTION('ref_axis',(-1.,0.,0.));
#18112=DIRECTION('center_axis',(0.,0.,1.));
#18113=DIRECTION('ref_axis',(-1.,0.,0.));
#18114=DIRECTION('center_axis',(0.,0.,1.));
#18115=DIRECTION('ref_axis',(-1.,0.,0.));
#18116=DIRECTION('center_axis',(0.,-1.,0.));
#18117=DIRECTION('ref_axis',(-1.,0.,0.));
#18118=DIRECTION('',(0.,0.,-1.));
#18119=DIRECTION('',(-1.,0.,0.));
#18120=DIRECTION('',(0.,0.,-1.));
#18121=DIRECTION('',(1.,0.,0.));
#18122=DIRECTION('center_axis',(1.,0.,0.));
#18123=DIRECTION('ref_axis',(0.,-1.,0.));
#18124=DIRECTION('',(0.,-1.,0.));
#18125=DIRECTION('',(0.,0.,-1.));
#18126=DIRECTION('',(0.,1.,0.));
#18127=DIRECTION('center_axis',(0.,1.,0.));
#18128=DIRECTION('ref_axis',(1.,0.,0.));
#18129=DIRECTION('',(0.,0.,1.));
#18130=DIRECTION('',(-1.,0.,0.));
#18131=DIRECTION('',(1.,0.,0.));
#18132=DIRECTION('center_axis',(0.,0.,1.));
#18133=DIRECTION('ref_axis',(1.,0.,0.));
#18134=DIRECTION('center_axis',(0.,0.,1.));
#18135=DIRECTION('ref_axis',(1.,0.,0.));
#18136=DIRECTION('center_axis',(0.,0.,-1.));
#18137=DIRECTION('ref_axis',(1.,0.,0.));
#18138=DIRECTION('center_axis',(0.,0.,-1.));
#18139=DIRECTION('ref_axis',(1.,-3.92491481346641E-15,0.));
#18140=DIRECTION('center_axis',(0.,0.,1.));
#18141=DIRECTION('ref_axis',(1.,0.,0.));
#18142=DIRECTION('center_axis',(0.,0.,1.));
#18143=DIRECTION('ref_axis',(1.,0.,0.));
#18144=DIRECTION('',(1.,0.,0.));
#18145=DIRECTION('',(0.,1.,0.));
#18146=DIRECTION('',(-1.,0.,0.));
#18147=DIRECTION('center_axis',(0.,0.,-1.));
#18148=DIRECTION('ref_axis',(1.,0.,0.));
#18149=DIRECTION('center_axis',(0.,-1.,0.));
#18150=DIRECTION('ref_axis',(1.,0.,0.));
#18151=DIRECTION('',(0.,0.,1.));
#18152=DIRECTION('',(1.,0.,0.));
#18153=DIRECTION('',(0.,0.,1.));
#18154=DIRECTION('center_axis',(0.,1.,0.));
#18155=DIRECTION('ref_axis',(-1.,0.,0.));
#18156=DIRECTION('',(0.,0.,-1.));
#18157=DIRECTION('',(0.,0.,1.));
#18158=DIRECTION('',(-1.,0.,0.));
#18159=DIRECTION('center_axis',(1.,0.,0.));
#18160=DIRECTION('ref_axis',(0.,1.,0.));
#18161=DIRECTION('',(0.,1.,0.));
#18162=DIRECTION('center_axis',(0.,0.,1.));
#18163=DIRECTION('ref_axis',(1.,0.,0.));
#18164=DIRECTION('center_axis',(0.,0.,-1.));
#18165=DIRECTION('ref_axis',(1.,0.,0.));
#18166=DIRECTION('center_axis',(0.,0.,1.));
#18167=DIRECTION('ref_axis',(1.,0.,0.));
#18168=DIRECTION('center_axis',(0.,0.,-1.));
#18169=DIRECTION('ref_axis',(1.,0.,0.));
#18170=DIRECTION('center_axis',(0.,0.,-1.));
#18171=DIRECTION('ref_axis',(1.,0.,0.));
#18172=DIRECTION('center_axis',(0.,0.,1.));
#18173=DIRECTION('ref_axis',(1.,0.,0.));
#18174=DIRECTION('center_axis',(0.,0.,1.));
#18175=DIRECTION('ref_axis',(1.,0.,0.));
#18176=DIRECTION('center_axis',(0.,0.,-1.));
#18177=DIRECTION('ref_axis',(1.,0.,0.));
#18178=DIRECTION('center_axis',(0.,0.,1.));
#18179=DIRECTION('ref_axis',(1.,0.,0.));
#18180=DIRECTION('',(0.,0.,-1.));
#18181=DIRECTION('center_axis',(0.,0.,1.));
#18182=DIRECTION('ref_axis',(1.,0.,0.));
#18183=DIRECTION('',(0.,0.,-1.));
#18184=DIRECTION('center_axis',(0.,0.,-1.));
#18185=DIRECTION('ref_axis',(1.,0.,0.));
#18186=DIRECTION('center_axis',(0.,0.,1.));
#18187=DIRECTION('ref_axis',(1.,0.,0.));
#18188=DIRECTION('center_axis',(0.,0.,-1.));
#18189=DIRECTION('ref_axis',(1.,0.,0.));
#18190=DIRECTION('center_axis',(0.,0.,1.));
#18191=DIRECTION('ref_axis',(1.,0.,0.));
#18192=DIRECTION('center_axis',(0.,0.,1.));
#18193=DIRECTION('ref_axis',(1.,0.,0.));
#18194=DIRECTION('center_axis',(0.,0.,-1.));
#18195=DIRECTION('ref_axis',(1.,0.,0.));
#18196=DIRECTION('center_axis',(0.,0.,1.));
#18197=DIRECTION('ref_axis',(1.,0.,0.));
#18198=DIRECTION('',(0.,0.,-1.));
#18199=DIRECTION('center_axis',(0.,0.,1.));
#18200=DIRECTION('ref_axis',(1.,0.,0.));
#18201=DIRECTION('',(0.,0.,-1.));
#18202=DIRECTION('center_axis',(0.,0.,1.));
#18203=DIRECTION('ref_axis',(1.,0.,0.));
#18204=DIRECTION('center_axis',(0.,0.,-1.));
#18205=DIRECTION('ref_axis',(1.,0.,0.));
#18206=DIRECTION('',(0.,0.,-1.));
#18207=DIRECTION('center_axis',(0.,0.,1.));
#18208=DIRECTION('ref_axis',(1.,0.,0.));
#18209=DIRECTION('center_axis',(0.,0.,1.));
#18210=DIRECTION('ref_axis',(1.,0.,0.));
#18211=DIRECTION('center_axis',(0.,0.,1.));
#18212=DIRECTION('ref_axis',(1.,0.,0.));
#18213=DIRECTION('axis',(0.,0.,1.));
#18214=DIRECTION('refdir',(1.,0.,0.));
#18215=DIRECTION('center_axis',(-1.,0.,0.));
#18216=DIRECTION('ref_axis',(0.,-0.346908023969935,0.937899153910096));
#18217=DIRECTION('',(-1.,0.,0.));
#18218=DIRECTION('center_axis',(1.,0.,0.));
#18219=DIRECTION('ref_axis',(0.,1.,0.));
#18220=DIRECTION('center_axis',(1.,0.,0.));
#18221=DIRECTION('ref_axis',(0.,1.,0.));
#18222=DIRECTION('center_axis',(-1.,0.,0.));
#18223=DIRECTION('ref_axis',(0.,1.,0.));
#18224=DIRECTION('',(-1.,0.,0.));
#18225=DIRECTION('center_axis',(-1.,0.,0.));
#18226=DIRECTION('ref_axis',(0.,1.,0.));
#18227=DIRECTION('',(-1.,0.,0.));
#18228=DIRECTION('center_axis',(-1.,0.,0.));
#18229=DIRECTION('ref_axis',(0.,1.,0.));
#18230=DIRECTION('',(-1.,0.,0.));
#18231=DIRECTION('center_axis',(-1.,0.,0.));
#18232=DIRECTION('ref_axis',(0.,1.,0.));
#18233=DIRECTION('',(-1.,0.,0.));
#18234=DIRECTION('center_axis',(-1.,0.,0.));
#18235=DIRECTION('ref_axis',(0.,1.,0.));
#18236=DIRECTION('',(-1.,0.,0.));
#18237=DIRECTION('center_axis',(-1.,0.,0.));
#18238=DIRECTION('ref_axis',(0.,1.,0.));
#18239=DIRECTION('',(-1.,0.,0.));
#18240=DIRECTION('center_axis',(-1.,0.,0.));
#18241=DIRECTION('ref_axis',(0.,1.,0.));
#18242=DIRECTION('',(-1.,0.,0.));
#18243=DIRECTION('center_axis',(-1.,0.,0.));
#18244=DIRECTION('ref_axis',(0.,1.,0.));
#18245=DIRECTION('',(-1.,0.,0.));
#18246=DIRECTION('center_axis',(-1.,0.,0.));
#18247=DIRECTION('ref_axis',(0.,1.,0.));
#18248=DIRECTION('',(-1.,0.,0.));
#18249=DIRECTION('center_axis',(-1.,0.,0.));
#18250=DIRECTION('ref_axis',(0.,1.,0.));
#18251=DIRECTION('',(-1.,0.,0.));
#18252=DIRECTION('center_axis',(-1.,0.,0.));
#18253=DIRECTION('ref_axis',(0.,1.,0.));
#18254=DIRECTION('',(-1.,0.,0.));
#18255=DIRECTION('center_axis',(-1.,0.,0.));
#18256=DIRECTION('ref_axis',(0.,1.,0.));
#18257=DIRECTION('',(-1.,0.,0.));
#18258=DIRECTION('center_axis',(-1.,0.,0.));
#18259=DIRECTION('ref_axis',(0.,1.,0.));
#18260=DIRECTION('',(-1.,0.,0.));
#18261=DIRECTION('center_axis',(-1.,0.,0.));
#18262=DIRECTION('ref_axis',(0.,1.,0.));
#18263=DIRECTION('',(-1.,0.,0.));
#18264=DIRECTION('center_axis',(-1.,0.,0.));
#18265=DIRECTION('ref_axis',(0.,1.,0.));
#18266=DIRECTION('',(-1.,0.,0.));
#18267=DIRECTION('center_axis',(-1.,0.,0.));
#18268=DIRECTION('ref_axis',(0.,1.,0.));
#18269=DIRECTION('',(-1.,0.,0.));
#18270=DIRECTION('center_axis',(-1.,0.,0.));
#18271=DIRECTION('ref_axis',(0.,0.887282355496419,-0.461226648866614));
#18272=DIRECTION('',(-1.,0.,0.));
#18273=DIRECTION('center_axis',(-1.,0.,0.));
#18274=DIRECTION('ref_axis',(0.,1.,-1.07644854835951E-13));
#18275=DIRECTION('',(-1.,1.22464679914735E-16,-1.31976902897796E-29));
#18276=DIRECTION('center_axis',(1.,0.,0.));
#18277=DIRECTION('ref_axis',(0.,1.,-1.07644854835951E-13));
#18278=DIRECTION('center_axis',(1.,0.,0.));
#18279=DIRECTION('ref_axis',(0.,1.,-1.07644854835951E-13));
#18280=DIRECTION('center_axis',(-1.,0.,0.));
#18281=DIRECTION('ref_axis',(0.,1.,-1.07644854835951E-13));
#18282=DIRECTION('',(-1.,1.22464679914735E-16,-1.31976902897796E-29));
#18283=DIRECTION('center_axis',(-1.,0.,0.));
#18284=DIRECTION('ref_axis',(0.,1.,-1.07644854835951E-13));
#18285=DIRECTION('',(-1.,1.22464679914735E-16,-1.31976902897796E-29));
#18286=DIRECTION('center_axis',(-1.,0.,0.));
#18287=DIRECTION('ref_axis',(0.,1.,-1.07644854835951E-13));
#18288=DIRECTION('',(-1.,1.22464679914735E-16,-1.31976902897796E-29));
#18289=DIRECTION('center_axis',(-1.,0.,0.));
#18290=DIRECTION('ref_axis',(0.,1.,-1.07644854835951E-13));
#18291=DIRECTION('',(-1.,1.22464679914735E-16,-1.31976902897796E-29));
#18292=DIRECTION('center_axis',(-1.,0.,0.));
#18293=DIRECTION('ref_axis',(0.,1.,-1.07644854835951E-13));
#18294=DIRECTION('',(-1.,1.22464679914735E-16,-1.31976902897796E-29));
#18295=DIRECTION('center_axis',(-1.,0.,0.));
#18296=DIRECTION('ref_axis',(0.,1.,-1.07644854835951E-13));
#18297=DIRECTION('',(-1.,1.22464679914735E-16,-1.31976902897796E-29));
#18298=DIRECTION('center_axis',(-1.,0.,0.));
#18299=DIRECTION('ref_axis',(0.,1.,-1.07644854835951E-13));
#18300=DIRECTION('',(-1.,1.22464679914735E-16,-1.31976902897796E-29));
#18301=DIRECTION('center_axis',(-1.,0.,0.));
#18302=DIRECTION('ref_axis',(0.,1.,-1.07644854835951E-13));
#18303=DIRECTION('',(-1.,1.22464679914735E-16,-1.31976902897796E-29));
#18304=DIRECTION('center_axis',(-1.,0.,0.));
#18305=DIRECTION('ref_axis',(0.,1.,-1.07644854835951E-13));
#18306=DIRECTION('',(-1.,1.22464679914735E-16,-1.31976902897796E-29));
#18307=DIRECTION('center_axis',(-1.,0.,0.));
#18308=DIRECTION('ref_axis',(0.,1.,-1.07644854835951E-13));
#18309=DIRECTION('',(-1.,1.22464679914735E-16,-1.31976902897796E-29));
#18310=DIRECTION('center_axis',(-1.,0.,0.));
#18311=DIRECTION('ref_axis',(0.,1.,-1.07644854835951E-13));
#18312=DIRECTION('',(-1.,1.22464679914735E-16,-1.31976902897796E-29));
#18313=DIRECTION('center_axis',(-1.,0.,0.));
#18314=DIRECTION('ref_axis',(0.,1.,-1.07644854835951E-13));
#18315=DIRECTION('',(-1.,1.22464679914735E-16,-1.31976902897796E-29));
#18316=DIRECTION('center_axis',(-1.,0.,0.));
#18317=DIRECTION('ref_axis',(0.,1.,-1.07644854835951E-13));
#18318=DIRECTION('',(-1.,1.22464679914735E-16,-1.31976902897796E-29));
#18319=DIRECTION('center_axis',(-1.,0.,0.));
#18320=DIRECTION('ref_axis',(0.,1.,-1.07644854835951E-13));
#18321=DIRECTION('',(-1.,1.22464679914735E-16,-1.31976902897796E-29));
#18322=DIRECTION('center_axis',(-1.,0.,0.));
#18323=DIRECTION('ref_axis',(0.,1.,-1.07644854835951E-13));
#18324=DIRECTION('',(-1.,1.22464679914735E-16,-1.31976902897796E-29));
#18325=DIRECTION('center_axis',(-1.,0.,0.));
#18326=DIRECTION('ref_axis',(0.,1.,-1.07644854835951E-13));
#18327=DIRECTION('',(-1.,1.22464679914735E-16,-1.31976902897796E-29));
#18328=DIRECTION('center_axis',(-1.,0.,0.));
#18329=DIRECTION('ref_axis',(0.,-0.628210160162024,-0.778043697146377));
#18330=DIRECTION('',(-1.,1.22464679914735E-16,-1.31976902897796E-29));
#18331=DIRECTION('center_axis',(0.,0.,1.));
#18332=DIRECTION('ref_axis',(1.,0.,0.));
#18333=DIRECTION('center_axis',(0.,0.,1.));
#18334=DIRECTION('ref_axis',(1.,0.,0.));
#18335=DIRECTION('',(0.,0.,1.));
#18336=DIRECTION('center_axis',(0.,0.,1.));
#18337=DIRECTION('ref_axis',(1.,0.,0.));
#18338=DIRECTION('center_axis',(0.,0.,-1.));
#18339=DIRECTION('ref_axis',(-1.,0.,0.));
#18340=DIRECTION('center_axis',(0.,0.,-1.));
#18341=DIRECTION('ref_axis',(1.,0.,0.));
#18342=DIRECTION('center_axis',(0.,0.,1.));
#18343=DIRECTION('ref_axis',(1.,0.,0.));
#18344=DIRECTION('center_axis',(0.,0.,1.));
#18345=DIRECTION('ref_axis',(1.,0.,0.));
#18346=DIRECTION('center_axis',(0.,0.,1.));
#18347=DIRECTION('ref_axis',(1.,0.,0.));
#18348=DIRECTION('center_axis',(0.,0.,1.));
#18349=DIRECTION('ref_axis',(1.,0.,0.));
#18350=DIRECTION('',(0.,0.,-1.));
#18351=DIRECTION('center_axis',(0.,-1.,0.));
#18352=DIRECTION('ref_axis',(0.,0.,-1.));
#18353=DIRECTION('',(0.,0.,1.));
#18354=DIRECTION('',(1.,0.,0.));
#18355=DIRECTION('',(0.,0.,-1.));
#18356=DIRECTION('',(-1.,0.,0.));
#18357=DIRECTION('center_axis',(-1.,0.,0.));
#18358=DIRECTION('ref_axis',(0.,0.,1.));
#18359=DIRECTION('',(0.,-1.,0.));
#18360=DIRECTION('',(0.,1.,0.));
#18361=DIRECTION('',(0.,0.,1.));
#18362=DIRECTION('center_axis',(0.,0.,1.));
#18363=DIRECTION('ref_axis',(1.,0.,0.));
#18364=DIRECTION('center_axis',(0.,0.,1.));
#18365=DIRECTION('ref_axis',(1.,0.,0.));
#18366=DIRECTION('',(1.,0.,0.));
#18367=DIRECTION('center_axis',(0.,1.,0.));
#18368=DIRECTION('ref_axis',(0.,0.,1.));
#18369=DIRECTION('',(0.,0.,-1.));
#18370=DIRECTION('',(-1.,0.,0.));
#18371=DIRECTION('center_axis',(0.,0.,1.));
#18372=DIRECTION('ref_axis',(1.,0.,0.));
#18373=DIRECTION('center_axis',(0.,0.,-1.));
#18374=DIRECTION('ref_axis',(1.,0.,0.));
#18375=DIRECTION('center_axis',(0.,0.,-1.));
#18376=DIRECTION('ref_axis',(1.,0.,0.));
#18377=DIRECTION('center_axis',(-1.,0.,0.));
#18378=DIRECTION('ref_axis',(0.,1.,-1.07644854835951E-13));
#18379=DIRECTION('center_axis',(-1.,0.,0.));
#18380=DIRECTION('ref_axis',(0.,1.,0.));
#18381=DIRECTION('',(0.,0.,-1.));
#18382=DIRECTION('center_axis',(-1.,0.,0.));
#18383=DIRECTION('ref_axis',(0.,1.,0.));
#18384=DIRECTION('center_axis',(-1.,0.,0.));
#18385=DIRECTION('ref_axis',(0.,1.,0.));
#18386=DIRECTION('',(0.,0.,-1.));
#18387=DIRECTION('center_axis',(0.,0.,1.));
#18388=DIRECTION('ref_axis',(-1.,0.,0.));
#18389=DIRECTION('center_axis',(0.,0.,1.));
#18390=DIRECTION('ref_axis',(-1.,0.,0.));
#18391=DIRECTION('',(0.,0.,1.));
#18392=DIRECTION('',(0.,0.,1.));
#18393=DIRECTION('center_axis',(0.,0.,1.));
#18394=DIRECTION('ref_axis',(-1.,0.,0.));
#18395=DIRECTION('center_axis',(0.,0.,1.));
#18396=DIRECTION('ref_axis',(-1.,0.,0.));
#18397=DIRECTION('center_axis',(0.,0.,1.));
#18398=DIRECTION('ref_axis',(1.,0.,0.));
#18399=DIRECTION('center_axis',(0.,0.,1.));
#18400=DIRECTION('ref_axis',(1.,0.,0.));
#18401=DIRECTION('',(0.,0.,-1.));
#18402=DIRECTION('center_axis',(0.,0.,1.));
#18403=DIRECTION('ref_axis',(1.,0.,0.));
#18404=DIRECTION('center_axis',(0.,0.,1.));
#18405=DIRECTION('ref_axis',(1.,0.,0.));
#18406=DIRECTION('center_axis',(0.,0.,1.));
#18407=DIRECTION('ref_axis',(1.,0.,0.));
#18408=DIRECTION('center_axis',(0.,0.,1.));
#18409=DIRECTION('ref_axis',(1.,0.,0.));
#18410=DIRECTION('center_axis',(0.,0.,1.));
#18411=DIRECTION('ref_axis',(1.,0.,0.));
#18412=DIRECTION('center_axis',(0.,0.,1.));
#18413=DIRECTION('ref_axis',(1.,0.,0.));
#18414=DIRECTION('center_axis',(0.,0.,-1.));
#18415=DIRECTION('ref_axis',(1.,0.,0.));
#18416=DIRECTION('center_axis',(0.,0.,1.));
#18417=DIRECTION('ref_axis',(1.,0.,0.));
#18418=DIRECTION('',(0.,0.,-1.));
#18419=DIRECTION('center_axis',(0.,0.,1.));
#18420=DIRECTION('ref_axis',(1.,0.,0.));
#18421=DIRECTION('',(0.,0.,-1.));
#18422=DIRECTION('center_axis',(0.,0.,1.));
#18423=DIRECTION('ref_axis',(1.,0.,0.));
#18424=DIRECTION('center_axis',(0.,0.,1.));
#18425=DIRECTION('ref_axis',(1.,0.,0.));
#18426=DIRECTION('center_axis',(0.,0.,1.));
#18427=DIRECTION('ref_axis',(1.,0.,0.));
#18428=DIRECTION('center_axis',(0.,0.,1.));
#18429=DIRECTION('ref_axis',(1.,0.,0.));
#18430=DIRECTION('',(0.,0.,-1.));
#18431=DIRECTION('center_axis',(0.,0.,1.));
#18432=DIRECTION('ref_axis',(1.,0.,0.));
#18433=DIRECTION('center_axis',(0.,0.,1.));
#18434=DIRECTION('ref_axis',(1.,0.,0.));
#18435=DIRECTION('center_axis',(0.,0.,1.));
#18436=DIRECTION('ref_axis',(1.,0.,0.));
#18437=DIRECTION('',(0.,0.,-1.));
#18438=DIRECTION('axis',(0.,0.,1.));
#18439=DIRECTION('refdir',(1.,0.,0.));
#18440=DIRECTION('center_axis',(0.,0.,1.));
#18441=DIRECTION('ref_axis',(1.,0.,0.));
#18442=DIRECTION('center_axis',(0.,0.,-1.));
#18443=DIRECTION('ref_axis',(1.,0.,0.));
#18444=DIRECTION('',(0.,0.,-1.));
#18445=DIRECTION('center_axis',(0.,0.,-1.));
#18446=DIRECTION('ref_axis',(1.,0.,0.));
#18447=DIRECTION('center_axis',(0.,0.,1.));
#18448=DIRECTION('ref_axis',(1.,0.,0.));
#18449=DIRECTION('center_axis',(0.,0.,1.));
#18450=DIRECTION('ref_axis',(1.,0.,0.));
#18451=DIRECTION('',(0.,0.,-1.));
#18452=DIRECTION('center_axis',(0.,0.,1.));
#18453=DIRECTION('ref_axis',(1.,0.,0.));
#18454=DIRECTION('center_axis',(0.,0.,1.));
#18455=DIRECTION('ref_axis',(1.,0.,0.));
#18456=DIRECTION('center_axis',(0.,0.,1.));
#18457=DIRECTION('ref_axis',(1.,0.,0.));
#18458=DIRECTION('axis',(0.,0.,1.));
#18459=DIRECTION('refdir',(1.,0.,0.));
#18460=DIRECTION('center_axis',(0.,0.,1.));
#18461=DIRECTION('ref_axis',(1.,0.,0.));
#18462=DIRECTION('center_axis',(0.,0.,-1.));
#18463=DIRECTION('ref_axis',(1.,0.,0.));
#18464=DIRECTION('',(0.,0.,-1.));
#18465=DIRECTION('center_axis',(0.,0.,-1.));
#18466=DIRECTION('ref_axis',(1.,0.,0.));
#18467=DIRECTION('center_axis',(0.,0.,1.));
#18468=DIRECTION('ref_axis',(1.,0.,0.));
#18469=DIRECTION('center_axis',(0.,0.,1.));
#18470=DIRECTION('ref_axis',(1.,0.,0.));
#18471=DIRECTION('',(0.,0.,-1.));
#18472=DIRECTION('center_axis',(0.,0.,1.));
#18473=DIRECTION('ref_axis',(1.,0.,0.));
#18474=DIRECTION('center_axis',(0.,0.,1.));
#18475=DIRECTION('ref_axis',(1.,0.,0.));
#18476=DIRECTION('center_axis',(0.,0.,1.));
#18477=DIRECTION('ref_axis',(1.,0.,0.));
#18478=DIRECTION('axis',(0.,0.,1.));
#18479=DIRECTION('refdir',(1.,0.,0.));
#18480=DIRECTION('center_axis',(-1.,0.,0.));
#18481=DIRECTION('ref_axis',(0.,1.,0.));
#18482=DIRECTION('',(0.,0.,1.));
#18483=DIRECTION('',(0.,-1.,0.));
#18484=DIRECTION('',(0.,0.,-1.));
#18485=DIRECTION('',(0.,1.,0.));
#18486=DIRECTION('center_axis',(1.,0.,0.));
#18487=DIRECTION('ref_axis',(0.,-1.,0.));
#18488=DIRECTION('',(0.,0.,-1.));
#18489=DIRECTION('',(0.,-1.,0.));
#18490=DIRECTION('',(0.,0.,1.));
#18491=DIRECTION('',(0.,1.,0.));
#18492=DIRECTION('center_axis',(0.,0.,1.));
#18493=DIRECTION('ref_axis',(1.,0.,0.));
#18494=DIRECTION('center_axis',(0.,0.,1.));
#18495=DIRECTION('ref_axis',(1.,0.,0.));
#18496=DIRECTION('center_axis',(0.,0.,-1.));
#18497=DIRECTION('ref_axis',(1.,0.,0.));
#18498=DIRECTION('center_axis',(0.,0.,1.));
#18499=DIRECTION('ref_axis',(6.12323399573677E-17,-1.,0.));
#18500=DIRECTION('center_axis',(0.,0.,-1.));
#18501=DIRECTION('ref_axis',(1.,0.,0.));
#18502=DIRECTION('center_axis',(0.,0.,1.));
#18503=DIRECTION('ref_axis',(6.12323399573677E-17,-1.,0.));
#18504=DIRECTION('center_axis',(0.,0.,1.));
#18505=DIRECTION('ref_axis',(1.,0.,0.));
#18506=DIRECTION('center_axis',(0.,0.,1.));
#18507=DIRECTION('ref_axis',(1.,0.,0.));
#18508=DIRECTION('axis',(0.,0.,1.));
#18509=DIRECTION('refdir',(1.,0.,0.));
#18510=DIRECTION('center_axis',(0.,1.,0.));
#18511=DIRECTION('ref_axis',(-1.,0.,0.));
#18512=DIRECTION('',(-1.,0.,0.));
#18513=DIRECTION('',(0.,0.,1.));
#18514=DIRECTION('',(-1.,0.,0.));
#18515=DIRECTION('',(0.,0.,1.));
#18516=DIRECTION('center_axis',(1.,0.,0.));
#18517=DIRECTION('ref_axis',(0.,1.,0.));
#18518=DIRECTION('',(0.,1.,0.));
#18519=DIRECTION('',(0.,1.,0.));
#18520=DIRECTION('',(0.,0.,1.));
#18521=DIRECTION('center_axis',(0.,-1.,0.));
#18522=DIRECTION('ref_axis',(1.,0.,0.));
#18523=DIRECTION('',(1.,0.,0.));
#18524=DIRECTION('',(1.,0.,0.));
#18525=DIRECTION('',(0.,0.,1.));
#18526=DIRECTION('center_axis',(-1.,0.,0.));
#18527=DIRECTION('ref_axis',(0.,-1.,0.));
#18528=DIRECTION('',(0.,-1.,0.));
#18529=DIRECTION('',(0.,-1.,0.));
#18530=DIRECTION('center_axis',(0.,0.,1.));
#18531=DIRECTION('ref_axis',(1.,0.,0.));
#18532=DIRECTION('center_axis',(0.,0.,1.));
#18533=DIRECTION('ref_axis',(1.,0.,0.));
#18534=DIRECTION('axis',(0.,0.,1.));
#18535=DIRECTION('refdir',(1.,0.,0.));
#18536=DIRECTION('center_axis',(0.,0.,1.));
#18537=DIRECTION('ref_axis',(1.,0.,0.));
#18538=DIRECTION('',(0.,0.,-1.));
#18539=DIRECTION('center_axis',(0.,0.,1.));
#18540=DIRECTION('ref_axis',(1.,0.,0.));
#18541=DIRECTION('center_axis',(0.,0.,1.));
#18542=DIRECTION('ref_axis',(1.,0.,0.));
#18543=DIRECTION('',(0.,0.,-1.));
#18544=DIRECTION('center_axis',(0.,0.,1.));
#18545=DIRECTION('ref_axis',(1.,0.,0.));
#18546=DIRECTION('',(0.,0.,-1.));
#18547=DIRECTION('center_axis',(0.,0.,1.));
#18548=DIRECTION('ref_axis',(1.,0.,0.));
#18549=DIRECTION('',(0.,0.,-1.));
#18550=DIRECTION('center_axis',(0.,0.,1.));
#18551=DIRECTION('ref_axis',(1.,0.,0.));
#18552=DIRECTION('',(0.,0.,-1.));
#18553=DIRECTION('center_axis',(0.,0.,1.));
#18554=DIRECTION('ref_axis',(1.,0.,0.));
#18555=DIRECTION('',(0.,0.,-1.));
#18556=DIRECTION('center_axis',(0.,0.,1.));
#18557=DIRECTION('ref_axis',(1.,0.,0.));
#18558=DIRECTION('',(0.,0.,-1.));
#18559=DIRECTION('center_axis',(0.,0.,1.));
#18560=DIRECTION('ref_axis',(1.,0.,0.));
#18561=DIRECTION('',(0.,0.,-1.));
#18562=DIRECTION('center_axis',(0.,0.,1.));
#18563=DIRECTION('ref_axis',(1.,0.,0.));
#18564=DIRECTION('',(0.,0.,-1.));
#18565=DIRECTION('center_axis',(0.,0.,1.));
#18566=DIRECTION('ref_axis',(1.,0.,0.));
#18567=DIRECTION('',(0.,0.,-1.));
#18568=DIRECTION('center_axis',(0.,0.,1.));
#18569=DIRECTION('ref_axis',(1.,0.,0.));
#18570=DIRECTION('',(0.,0.,-1.));
#18571=DIRECTION('center_axis',(0.,0.,1.));
#18572=DIRECTION('ref_axis',(1.,0.,0.));
#18573=DIRECTION('',(0.,0.,-1.));
#18574=DIRECTION('center_axis',(0.,0.,1.));
#18575=DIRECTION('ref_axis',(1.,0.,0.));
#18576=DIRECTION('',(0.,0.,-1.));
#18577=DIRECTION('center_axis',(0.,0.,1.));
#18578=DIRECTION('ref_axis',(1.,0.,0.));
#18579=DIRECTION('',(0.,0.,-1.));
#18580=DIRECTION('center_axis',(0.,0.,1.));
#18581=DIRECTION('ref_axis',(1.,0.,0.));
#18582=DIRECTION('',(0.,0.,-1.));
#18583=DIRECTION('center_axis',(0.,0.,1.));
#18584=DIRECTION('ref_axis',(1.,0.,0.));
#18585=DIRECTION('',(0.,0.,-1.));
#18586=DIRECTION('center_axis',(0.,0.,1.));
#18587=DIRECTION('ref_axis',(1.,0.,0.));
#18588=DIRECTION('',(0.,0.,-1.));
#18589=DIRECTION('center_axis',(0.,0.,1.));
#18590=DIRECTION('ref_axis',(1.,0.,0.));
#18591=DIRECTION('',(0.,0.,-1.));
#18592=DIRECTION('center_axis',(0.,0.,1.));
#18593=DIRECTION('ref_axis',(1.,0.,0.));
#18594=DIRECTION('',(0.,0.,-1.));
#18595=DIRECTION('center_axis',(0.,0.,1.));
#18596=DIRECTION('ref_axis',(1.,0.,0.));
#18597=DIRECTION('',(0.,0.,-1.));
#18598=DIRECTION('center_axis',(0.,0.,1.));
#18599=DIRECTION('ref_axis',(1.,0.,0.));
#18600=DIRECTION('',(0.,0.,-1.));
#18601=DIRECTION('center_axis',(0.,0.,1.));
#18602=DIRECTION('ref_axis',(1.,0.,0.));
#18603=DIRECTION('',(0.,0.,-1.));
#18604=DIRECTION('center_axis',(0.,0.,1.));
#18605=DIRECTION('ref_axis',(1.,0.,0.));
#18606=DIRECTION('',(0.,0.,-1.));
#18607=DIRECTION('center_axis',(0.,0.,1.));
#18608=DIRECTION('ref_axis',(1.,0.,0.));
#18609=DIRECTION('',(0.,0.,-1.));
#18610=DIRECTION('center_axis',(0.,0.,1.));
#18611=DIRECTION('ref_axis',(1.,0.,0.));
#18612=DIRECTION('',(0.,0.,-1.));
#18613=DIRECTION('center_axis',(0.,0.,1.));
#18614=DIRECTION('ref_axis',(1.,0.,0.));
#18615=DIRECTION('',(0.,0.,-1.));
#18616=DIRECTION('center_axis',(0.,0.,1.));
#18617=DIRECTION('ref_axis',(1.,0.,0.));
#18618=DIRECTION('',(0.,0.,-1.));
#18619=DIRECTION('center_axis',(0.,0.,1.));
#18620=DIRECTION('ref_axis',(1.,0.,0.));
#18621=DIRECTION('',(0.,0.,-1.));
#18622=DIRECTION('center_axis',(0.,0.,1.));
#18623=DIRECTION('ref_axis',(1.,0.,0.));
#18624=DIRECTION('',(0.,0.,-1.));
#18625=DIRECTION('center_axis',(0.,0.,1.));
#18626=DIRECTION('ref_axis',(1.,0.,0.));
#18627=DIRECTION('',(0.,0.,-1.));
#18628=DIRECTION('center_axis',(0.,0.,1.));
#18629=DIRECTION('ref_axis',(1.,0.,0.));
#18630=DIRECTION('',(0.,0.,-1.));
#18631=DIRECTION('center_axis',(0.,0.,1.));
#18632=DIRECTION('ref_axis',(1.,0.,0.));
#18633=DIRECTION('',(0.,0.,-1.));
#18634=DIRECTION('center_axis',(0.,0.,1.));
#18635=DIRECTION('ref_axis',(1.,0.,0.));
#18636=DIRECTION('',(0.,0.,-1.));
#18637=DIRECTION('center_axis',(0.,0.,1.));
#18638=DIRECTION('ref_axis',(1.,0.,0.));
#18639=DIRECTION('',(0.,0.,-1.));
#18640=DIRECTION('center_axis',(0.,0.,1.));
#18641=DIRECTION('ref_axis',(1.,0.,0.));
#18642=DIRECTION('',(0.,0.,-1.));
#18643=DIRECTION('center_axis',(0.,0.,1.));
#18644=DIRECTION('ref_axis',(1.,0.,0.));
#18645=DIRECTION('',(0.,0.,-1.));
#18646=DIRECTION('center_axis',(0.,0.,1.));
#18647=DIRECTION('ref_axis',(1.,0.,0.));
#18648=DIRECTION('',(0.,0.,-1.));
#18649=DIRECTION('center_axis',(0.,0.,1.));
#18650=DIRECTION('ref_axis',(1.,0.,0.));
#18651=DIRECTION('',(0.,0.,-1.));
#18652=DIRECTION('center_axis',(0.,0.,1.));
#18653=DIRECTION('ref_axis',(1.,0.,0.));
#18654=DIRECTION('',(0.,0.,-1.));
#18655=DIRECTION('center_axis',(0.,0.,1.));
#18656=DIRECTION('ref_axis',(1.,0.,0.));
#18657=DIRECTION('',(0.,0.,-1.));
#18658=DIRECTION('center_axis',(0.,0.,1.));
#18659=DIRECTION('ref_axis',(1.,0.,0.));
#18660=DIRECTION('',(0.,0.,-1.));
#18661=DIRECTION('center_axis',(0.,0.,1.));
#18662=DIRECTION('ref_axis',(1.,0.,0.));
#18663=DIRECTION('',(0.,0.,-1.));
#18664=DIRECTION('center_axis',(0.,0.,1.));
#18665=DIRECTION('ref_axis',(1.,0.,0.));
#18666=DIRECTION('',(0.,0.,-1.));
#18667=DIRECTION('center_axis',(0.,0.,1.));
#18668=DIRECTION('ref_axis',(1.,0.,0.));
#18669=DIRECTION('',(0.,0.,-1.));
#18670=DIRECTION('center_axis',(0.,0.,1.));
#18671=DIRECTION('ref_axis',(1.,0.,0.));
#18672=DIRECTION('',(0.,0.,-1.));
#18673=DIRECTION('center_axis',(0.,0.,1.));
#18674=DIRECTION('ref_axis',(1.,0.,0.));
#18675=DIRECTION('',(0.,0.,-1.));
#18676=DIRECTION('center_axis',(0.,0.,1.));
#18677=DIRECTION('ref_axis',(1.,0.,0.));
#18678=DIRECTION('',(0.,0.,-1.));
#18679=DIRECTION('center_axis',(0.,0.,1.));
#18680=DIRECTION('ref_axis',(1.,0.,0.));
#18681=DIRECTION('',(0.,0.,-1.));
#18682=DIRECTION('center_axis',(0.,0.,1.));
#18683=DIRECTION('ref_axis',(1.,0.,0.));
#18684=DIRECTION('',(0.,0.,-1.));
#18685=DIRECTION('center_axis',(0.,0.,1.));
#18686=DIRECTION('ref_axis',(1.,0.,0.));
#18687=DIRECTION('',(0.,0.,-1.));
#18688=DIRECTION('center_axis',(0.,0.,1.));
#18689=DIRECTION('ref_axis',(1.,0.,0.));
#18690=DIRECTION('',(0.,0.,-1.));
#18691=DIRECTION('center_axis',(0.,0.,1.));
#18692=DIRECTION('ref_axis',(1.,0.,0.));
#18693=DIRECTION('',(0.,0.,-1.));
#18694=DIRECTION('center_axis',(0.,0.,1.));
#18695=DIRECTION('ref_axis',(1.,0.,0.));
#18696=DIRECTION('',(0.,0.,-1.));
#18697=DIRECTION('center_axis',(0.,0.,1.));
#18698=DIRECTION('ref_axis',(1.,0.,0.));
#18699=DIRECTION('',(0.,0.,-1.));
#18700=DIRECTION('center_axis',(0.,0.,1.));
#18701=DIRECTION('ref_axis',(1.,0.,0.));
#18702=DIRECTION('',(0.,0.,-1.));
#18703=DIRECTION('center_axis',(0.,0.,1.));
#18704=DIRECTION('ref_axis',(1.,0.,0.));
#18705=DIRECTION('',(0.,0.,-1.));
#18706=DIRECTION('center_axis',(0.,0.,1.));
#18707=DIRECTION('ref_axis',(1.,0.,0.));
#18708=DIRECTION('',(0.,0.,-1.));
#18709=DIRECTION('center_axis',(0.,0.,1.));
#18710=DIRECTION('ref_axis',(1.,0.,0.));
#18711=DIRECTION('',(0.,0.,-1.));
#18712=DIRECTION('center_axis',(0.,0.,1.));
#18713=DIRECTION('ref_axis',(1.,0.,0.));
#18714=DIRECTION('',(0.,0.,-1.));
#18715=DIRECTION('center_axis',(0.,0.,1.));
#18716=DIRECTION('ref_axis',(1.,0.,0.));
#18717=DIRECTION('',(0.,0.,-1.));
#18718=DIRECTION('center_axis',(0.,0.,1.));
#18719=DIRECTION('ref_axis',(1.,0.,0.));
#18720=DIRECTION('',(0.,0.,-1.));
#18721=DIRECTION('center_axis',(0.,0.,1.));
#18722=DIRECTION('ref_axis',(1.,0.,0.));
#18723=DIRECTION('',(0.,0.,-1.));
#18724=DIRECTION('center_axis',(0.,0.,1.));
#18725=DIRECTION('ref_axis',(1.,0.,0.));
#18726=DIRECTION('',(0.,0.,-1.));
#18727=DIRECTION('center_axis',(0.,0.,1.));
#18728=DIRECTION('ref_axis',(1.,0.,0.));
#18729=DIRECTION('',(0.,0.,-1.));
#18730=DIRECTION('center_axis',(0.,0.,1.));
#18731=DIRECTION('ref_axis',(1.,0.,0.));
#18732=DIRECTION('',(0.,0.,-1.));
#18733=DIRECTION('center_axis',(0.,0.,1.));
#18734=DIRECTION('ref_axis',(1.,0.,0.));
#18735=DIRECTION('',(0.,0.,-1.));
#18736=DIRECTION('center_axis',(0.,0.,1.));
#18737=DIRECTION('ref_axis',(1.,0.,0.));
#18738=DIRECTION('',(0.,0.,-1.));
#18739=DIRECTION('center_axis',(0.,0.,1.));
#18740=DIRECTION('ref_axis',(1.,0.,0.));
#18741=DIRECTION('',(0.,0.,-1.));
#18742=DIRECTION('center_axis',(0.,0.,1.));
#18743=DIRECTION('ref_axis',(1.,0.,0.));
#18744=DIRECTION('',(0.,0.,-1.));
#18745=DIRECTION('center_axis',(0.,0.,1.));
#18746=DIRECTION('ref_axis',(1.,0.,0.));
#18747=DIRECTION('',(0.,0.,-1.));
#18748=DIRECTION('center_axis',(0.,0.,1.));
#18749=DIRECTION('ref_axis',(1.,0.,0.));
#18750=DIRECTION('',(0.,0.,-1.));
#18751=DIRECTION('center_axis',(0.,0.,1.));
#18752=DIRECTION('ref_axis',(1.,0.,0.));
#18753=DIRECTION('',(0.,0.,-1.));
#18754=DIRECTION('center_axis',(0.,0.,1.));
#18755=DIRECTION('ref_axis',(1.,0.,0.));
#18756=DIRECTION('',(0.,0.,-1.));
#18757=DIRECTION('center_axis',(0.,0.,1.));
#18758=DIRECTION('ref_axis',(1.,0.,0.));
#18759=DIRECTION('',(0.,0.,-1.));
#18760=DIRECTION('center_axis',(0.,0.,1.));
#18761=DIRECTION('ref_axis',(1.,0.,0.));
#18762=DIRECTION('',(0.,0.,-1.));
#18763=DIRECTION('center_axis',(0.,0.,1.));
#18764=DIRECTION('ref_axis',(1.,0.,0.));
#18765=DIRECTION('',(0.,0.,-1.));
#18766=DIRECTION('center_axis',(0.,0.,1.));
#18767=DIRECTION('ref_axis',(1.,0.,0.));
#18768=DIRECTION('',(0.,0.,-1.));
#18769=DIRECTION('center_axis',(0.,0.,1.));
#18770=DIRECTION('ref_axis',(1.,0.,0.));
#18771=DIRECTION('',(0.,0.,-1.));
#18772=DIRECTION('center_axis',(0.,0.,1.));
#18773=DIRECTION('ref_axis',(1.,0.,0.));
#18774=DIRECTION('center_axis',(0.,0.,-1.));
#18775=DIRECTION('ref_axis',(1.,0.,0.));
#18776=DIRECTION('',(0.,0.,-1.));
#18777=DIRECTION('center_axis',(0.,0.,1.));
#18778=DIRECTION('ref_axis',(1.,0.,0.));
#18779=DIRECTION('',(0.,0.,-1.));
#18780=DIRECTION('center_axis',(0.,0.,1.));
#18781=DIRECTION('ref_axis',(1.,0.,0.));
#18782=DIRECTION('center_axis',(0.,0.,1.));
#18783=DIRECTION('ref_axis',(-0.45747178569478,-0.889224136701894,0.));
#18784=DIRECTION('',(0.,0.,1.));
#18785=DIRECTION('center_axis',(0.,0.,1.));
#18786=DIRECTION('ref_axis',(1.,-1.39943489555162E-12,0.));
#18787=DIRECTION('center_axis',(0.,0.,1.));
#18788=DIRECTION('ref_axis',(1.,-1.39943489555162E-12,0.));
#18789=DIRECTION('',(0.,0.,1.));
#18790=DIRECTION('center_axis',(0.,0.,1.));
#18791=DIRECTION('ref_axis',(1.,-1.39943489555162E-12,0.));
#18792=DIRECTION('',(0.,0.,1.));
#18793=DIRECTION('center_axis',(0.,0.,1.));
#18794=DIRECTION('ref_axis',(1.,-1.39943489555162E-12,0.));
#18795=DIRECTION('',(0.,0.,1.));
#18796=DIRECTION('center_axis',(0.,0.,1.));
#18797=DIRECTION('ref_axis',(1.,-1.39943489555162E-12,0.));
#18798=DIRECTION('',(0.,0.,1.));
#18799=DIRECTION('center_axis',(0.,0.,1.));
#18800=DIRECTION('ref_axis',(1.,-1.39943489555162E-12,0.));
#18801=DIRECTION('',(0.,0.,1.));
#18802=DIRECTION('center_axis',(0.,0.,1.));
#18803=DIRECTION('ref_axis',(1.,-1.39943489555162E-12,0.));
#18804=DIRECTION('',(0.,0.,1.));
#18805=DIRECTION('center_axis',(0.,0.,1.));
#18806=DIRECTION('ref_axis',(1.,-1.39943489555162E-12,0.));
#18807=DIRECTION('',(0.,0.,1.));
#18808=DIRECTION('center_axis',(0.,0.,1.));
#18809=DIRECTION('ref_axis',(1.,-1.39943489555162E-12,0.));
#18810=DIRECTION('',(0.,0.,1.));
#18811=DIRECTION('center_axis',(0.,0.,1.));
#18812=DIRECTION('ref_axis',(1.,-1.39943489555162E-12,0.));
#18813=DIRECTION('',(0.,0.,1.));
#18814=DIRECTION('center_axis',(0.,0.,1.));
#18815=DIRECTION('ref_axis',(1.,-1.39943489555162E-12,0.));
#18816=DIRECTION('',(0.,0.,1.));
#18817=DIRECTION('center_axis',(0.,0.,1.));
#18818=DIRECTION('ref_axis',(1.,-1.39943489555162E-12,0.));
#18819=DIRECTION('',(0.,0.,1.));
#18820=DIRECTION('center_axis',(0.,0.,1.));
#18821=DIRECTION('ref_axis',(1.,-1.39943489555162E-12,0.));
#18822=DIRECTION('',(0.,0.,1.));
#18823=DIRECTION('center_axis',(0.,0.,1.));
#18824=DIRECTION('ref_axis',(1.,-1.39943489555162E-12,0.));
#18825=DIRECTION('',(0.,0.,1.));
#18826=DIRECTION('center_axis',(0.,0.,1.));
#18827=DIRECTION('ref_axis',(1.,-1.39943489555162E-12,0.));
#18828=DIRECTION('',(0.,0.,1.));
#18829=DIRECTION('center_axis',(0.,0.,1.));
#18830=DIRECTION('ref_axis',(1.,-1.39943489555162E-12,0.));
#18831=DIRECTION('',(0.,0.,1.));
#18832=DIRECTION('center_axis',(0.,0.,1.));
#18833=DIRECTION('ref_axis',(1.,-1.39943489555162E-12,0.));
#18834=DIRECTION('',(0.,0.,1.));
#18835=DIRECTION('center_axis',(0.,0.,1.));
#18836=DIRECTION('ref_axis',(1.,-1.39943489555162E-12,0.));
#18837=DIRECTION('',(0.,0.,1.));
#18838=DIRECTION('center_axis',(0.,0.,1.));
#18839=DIRECTION('ref_axis',(1.,-1.39943489555162E-12,0.));
#18840=DIRECTION('',(0.,0.,1.));
#18841=DIRECTION('center_axis',(0.,0.,1.));
#18842=DIRECTION('ref_axis',(1.,-1.39943489555162E-12,0.));
#18843=DIRECTION('',(0.,0.,1.));
#18844=DIRECTION('center_axis',(0.,0.,1.));
#18845=DIRECTION('ref_axis',(1.,-1.39943489555162E-12,0.));
#18846=DIRECTION('',(0.,0.,1.));
#18847=DIRECTION('center_axis',(0.,0.,1.));
#18848=DIRECTION('ref_axis',(1.,-1.39943489555162E-12,0.));
#18849=DIRECTION('',(0.,0.,1.));
#18850=DIRECTION('center_axis',(0.,0.,1.));
#18851=DIRECTION('ref_axis',(1.,-1.39943489555162E-12,0.));
#18852=DIRECTION('',(0.,0.,1.));
#18853=DIRECTION('center_axis',(0.,0.,1.));
#18854=DIRECTION('ref_axis',(1.,-1.39943489555162E-12,0.));
#18855=DIRECTION('',(0.,0.,1.));
#18856=DIRECTION('center_axis',(0.,0.,1.));
#18857=DIRECTION('ref_axis',(1.,-1.39943489555162E-12,0.));
#18858=DIRECTION('',(0.,0.,1.));
#18859=DIRECTION('center_axis',(0.,0.,1.));
#18860=DIRECTION('ref_axis',(1.,-1.39943489555162E-12,0.));
#18861=DIRECTION('',(0.,0.,1.));
#18862=DIRECTION('center_axis',(0.,0.,1.));
#18863=DIRECTION('ref_axis',(1.,-1.39943489555162E-12,0.));
#18864=DIRECTION('',(0.,0.,1.));
#18865=DIRECTION('center_axis',(0.,0.,1.));
#18866=DIRECTION('ref_axis',(1.,-1.39943489555162E-12,0.));
#18867=DIRECTION('',(0.,0.,1.));
#18868=DIRECTION('center_axis',(0.,0.,1.));
#18869=DIRECTION('ref_axis',(1.,-1.39943489555162E-12,0.));
#18870=DIRECTION('',(0.,0.,1.));
#18871=DIRECTION('center_axis',(0.,0.,1.));
#18872=DIRECTION('ref_axis',(1.,-1.39943489555162E-12,0.));
#18873=DIRECTION('',(0.,0.,1.));
#18874=DIRECTION('center_axis',(0.,0.,1.));
#18875=DIRECTION('ref_axis',(1.,-1.39943489555162E-12,0.));
#18876=DIRECTION('',(0.,0.,1.));
#18877=DIRECTION('center_axis',(0.,0.,1.));
#18878=DIRECTION('ref_axis',(1.,-1.39943489555162E-12,0.));
#18879=DIRECTION('',(0.,0.,1.));
#18880=DIRECTION('center_axis',(0.,0.,1.));
#18881=DIRECTION('ref_axis',(1.,-1.39943489555162E-12,0.));
#18882=DIRECTION('',(0.,0.,1.));
#18883=DIRECTION('center_axis',(0.,0.,1.));
#18884=DIRECTION('ref_axis',(1.,-1.39943489555162E-12,0.));
#18885=DIRECTION('',(0.,0.,1.));
#18886=DIRECTION('center_axis',(0.,0.,1.));
#18887=DIRECTION('ref_axis',(1.,-1.39943489555162E-12,0.));
#18888=DIRECTION('',(0.,0.,1.));
#18889=DIRECTION('center_axis',(0.,0.,1.));
#18890=DIRECTION('ref_axis',(1.,-1.39943489555162E-12,0.));
#18891=DIRECTION('',(0.,0.,1.));
#18892=DIRECTION('center_axis',(0.,0.,1.));
#18893=DIRECTION('ref_axis',(1.,-1.39943489555162E-12,0.));
#18894=DIRECTION('',(0.,0.,1.));
#18895=DIRECTION('center_axis',(0.,0.,1.));
#18896=DIRECTION('ref_axis',(1.,-1.39943489555162E-12,0.));
#18897=DIRECTION('',(0.,0.,1.));
#18898=DIRECTION('center_axis',(0.,0.,1.));
#18899=DIRECTION('ref_axis',(1.,-1.39943489555162E-12,0.));
#18900=DIRECTION('',(0.,0.,1.));
#18901=DIRECTION('center_axis',(0.,0.,1.));
#18902=DIRECTION('ref_axis',(1.,-1.39943489555162E-12,0.));
#18903=DIRECTION('',(0.,0.,1.));
#18904=DIRECTION('center_axis',(0.,0.,1.));
#18905=DIRECTION('ref_axis',(1.,-1.39943489555162E-12,0.));
#18906=DIRECTION('',(0.,0.,1.));
#18907=DIRECTION('center_axis',(0.,0.,1.));
#18908=DIRECTION('ref_axis',(1.,-1.39943489555162E-12,0.));
#18909=DIRECTION('',(0.,0.,1.));
#18910=DIRECTION('center_axis',(0.,0.,1.));
#18911=DIRECTION('ref_axis',(1.,-1.39943489555162E-12,0.));
#18912=DIRECTION('',(0.,0.,1.));
#18913=DIRECTION('center_axis',(0.,0.,1.));
#18914=DIRECTION('ref_axis',(1.,-1.39943489555162E-12,0.));
#18915=DIRECTION('',(0.,0.,1.));
#18916=DIRECTION('center_axis',(0.,0.,1.));
#18917=DIRECTION('ref_axis',(1.,-1.39943489555162E-12,0.));
#18918=DIRECTION('',(0.,0.,1.));
#18919=DIRECTION('center_axis',(0.,0.,1.));
#18920=DIRECTION('ref_axis',(1.,-1.39943489555162E-12,0.));
#18921=DIRECTION('',(0.,0.,1.));
#18922=DIRECTION('center_axis',(0.,0.,1.));
#18923=DIRECTION('ref_axis',(1.,-1.39943489555162E-12,0.));
#18924=DIRECTION('',(0.,0.,1.));
#18925=DIRECTION('center_axis',(0.,0.,1.));
#18926=DIRECTION('ref_axis',(1.,-1.39943489555162E-12,0.));
#18927=DIRECTION('',(0.,0.,1.));
#18928=DIRECTION('center_axis',(0.,0.,1.));
#18929=DIRECTION('ref_axis',(1.,-1.39943489555162E-12,0.));
#18930=DIRECTION('',(0.,0.,1.));
#18931=DIRECTION('center_axis',(0.,0.,1.));
#18932=DIRECTION('ref_axis',(1.,-1.39943489555162E-12,0.));
#18933=DIRECTION('',(0.,0.,1.));
#18934=DIRECTION('center_axis',(0.,0.,1.));
#18935=DIRECTION('ref_axis',(1.,-1.39943489555162E-12,0.));
#18936=DIRECTION('',(0.,0.,1.));
#18937=DIRECTION('center_axis',(0.,0.,1.));
#18938=DIRECTION('ref_axis',(1.,-1.39943489555162E-12,0.));
#18939=DIRECTION('',(0.,0.,1.));
#18940=DIRECTION('center_axis',(0.,0.,1.));
#18941=DIRECTION('ref_axis',(1.,-1.39943489555162E-12,0.));
#18942=DIRECTION('',(0.,0.,1.));
#18943=DIRECTION('center_axis',(0.,0.,1.));
#18944=DIRECTION('ref_axis',(1.,-1.39943489555162E-12,0.));
#18945=DIRECTION('',(0.,0.,1.));
#18946=DIRECTION('center_axis',(0.,0.,1.));
#18947=DIRECTION('ref_axis',(1.,-1.39943489555162E-12,0.));
#18948=DIRECTION('',(0.,0.,1.));
#18949=DIRECTION('center_axis',(0.,0.,1.));
#18950=DIRECTION('ref_axis',(1.,-1.39943489555162E-12,0.));
#18951=DIRECTION('',(0.,0.,1.));
#18952=DIRECTION('center_axis',(0.,0.,1.));
#18953=DIRECTION('ref_axis',(1.,-1.39943489555162E-12,0.));
#18954=DIRECTION('',(0.,0.,1.));
#18955=DIRECTION('center_axis',(0.,0.,1.));
#18956=DIRECTION('ref_axis',(1.,-1.39943489555162E-12,0.));
#18957=DIRECTION('',(0.,0.,1.));
#18958=DIRECTION('center_axis',(0.,0.,1.));
#18959=DIRECTION('ref_axis',(1.,-1.39943489555162E-12,0.));
#18960=DIRECTION('',(0.,0.,1.));
#18961=DIRECTION('center_axis',(0.,0.,1.));
#18962=DIRECTION('ref_axis',(1.,-1.39943489555162E-12,0.));
#18963=DIRECTION('',(0.,0.,1.));
#18964=DIRECTION('center_axis',(0.,0.,1.));
#18965=DIRECTION('ref_axis',(1.,-1.39943489555162E-12,0.));
#18966=DIRECTION('',(0.,0.,1.));
#18967=DIRECTION('center_axis',(0.,0.,1.));
#18968=DIRECTION('ref_axis',(1.,-1.39943489555162E-12,0.));
#18969=DIRECTION('',(0.,0.,1.));
#18970=DIRECTION('center_axis',(0.,0.,1.));
#18971=DIRECTION('ref_axis',(1.,-1.39943489555162E-12,0.));
#18972=DIRECTION('',(0.,0.,1.));
#18973=DIRECTION('center_axis',(0.,0.,1.));
#18974=DIRECTION('ref_axis',(1.,-1.39943489555162E-12,0.));
#18975=DIRECTION('',(0.,0.,1.));
#18976=DIRECTION('center_axis',(0.,0.,1.));
#18977=DIRECTION('ref_axis',(1.,-1.39943489555162E-12,0.));
#18978=DIRECTION('',(0.,0.,1.));
#18979=DIRECTION('center_axis',(0.,0.,1.));
#18980=DIRECTION('ref_axis',(1.,-1.39943489555162E-12,0.));
#18981=DIRECTION('',(0.,0.,1.));
#18982=DIRECTION('center_axis',(0.,0.,1.));
#18983=DIRECTION('ref_axis',(1.,-1.39943489555162E-12,0.));
#18984=DIRECTION('',(0.,0.,1.));
#18985=DIRECTION('center_axis',(0.,0.,1.));
#18986=DIRECTION('ref_axis',(1.,-1.39943489555162E-12,0.));
#18987=DIRECTION('',(0.,0.,1.));
#18988=DIRECTION('center_axis',(0.,0.,1.));
#18989=DIRECTION('ref_axis',(1.,-1.39943489555162E-12,0.));
#18990=DIRECTION('',(0.,0.,1.));
#18991=DIRECTION('center_axis',(0.,0.,1.));
#18992=DIRECTION('ref_axis',(1.,-1.39943489555162E-12,0.));
#18993=DIRECTION('',(0.,0.,1.));
#18994=DIRECTION('center_axis',(0.,0.,1.));
#18995=DIRECTION('ref_axis',(1.,-1.39943489555162E-12,0.));
#18996=DIRECTION('',(0.,0.,1.));
#18997=DIRECTION('center_axis',(0.,0.,1.));
#18998=DIRECTION('ref_axis',(1.,-1.39943489555162E-12,0.));
#18999=DIRECTION('',(0.,0.,1.));
#19000=DIRECTION('center_axis',(0.,0.,1.));
#19001=DIRECTION('ref_axis',(1.,-1.39943489555162E-12,0.));
#19002=DIRECTION('',(0.,0.,1.));
#19003=DIRECTION('center_axis',(0.,0.,1.));
#19004=DIRECTION('ref_axis',(1.,-1.39943489555162E-12,0.));
#19005=DIRECTION('',(0.,0.,1.));
#19006=DIRECTION('center_axis',(0.,0.,1.));
#19007=DIRECTION('ref_axis',(1.,-1.39943489555162E-12,0.));
#19008=DIRECTION('',(0.,0.,1.));
#19009=DIRECTION('center_axis',(0.,0.,1.));
#19010=DIRECTION('ref_axis',(1.,-1.39943489555162E-12,0.));
#19011=DIRECTION('',(0.,0.,1.));
#19012=DIRECTION('center_axis',(0.,0.,1.));
#19013=DIRECTION('ref_axis',(1.,-1.39943489555162E-12,0.));
#19014=DIRECTION('',(0.,0.,1.));
#19015=DIRECTION('center_axis',(0.,0.,1.));
#19016=DIRECTION('ref_axis',(1.,-1.39943489555162E-12,0.));
#19017=DIRECTION('',(0.,0.,1.));
#19018=DIRECTION('center_axis',(0.,0.,1.));
#19019=DIRECTION('ref_axis',(1.,-1.39943489555162E-12,0.));
#19020=DIRECTION('',(0.,0.,1.));
#19021=DIRECTION('center_axis',(0.,0.,1.));
#19022=DIRECTION('ref_axis',(1.,-1.39943489555162E-12,0.));
#19023=DIRECTION('',(0.,0.,1.));
#19024=DIRECTION('center_axis',(0.,0.,1.));
#19025=DIRECTION('ref_axis',(-0.640826195965856,0.767685994768649,0.));
#19026=DIRECTION('center_axis',(0.,0.,-1.));
#19027=DIRECTION('ref_axis',(1.,0.,0.));
#19028=DIRECTION('center_axis',(0.,0.,1.));
#19029=DIRECTION('ref_axis',(1.,0.,0.));
#19030=DIRECTION('center_axis',(0.,0.,-1.));
#19031=DIRECTION('ref_axis',(1.,-1.39943489555162E-12,0.));
#19032=DIRECTION('center_axis',(0.,0.,1.));
#19033=DIRECTION('ref_axis',(1.,0.,0.));
#19034=DIRECTION('center_axis',(0.,0.,1.));
#19035=DIRECTION('ref_axis',(1.,0.,0.));
#19036=DIRECTION('',(0.,0.,1.));
#19037=DIRECTION('center_axis',(0.,0.,1.));
#19038=DIRECTION('ref_axis',(1.,0.,0.));
#19039=DIRECTION('center_axis',(0.,0.,-1.));
#19040=DIRECTION('ref_axis',(-1.,0.,0.));
#19041=DIRECTION('center_axis',(0.,0.,1.));
#19042=DIRECTION('ref_axis',(1.,0.,0.));
#19043=DIRECTION('center_axis',(0.,0.,1.));
#19044=DIRECTION('ref_axis',(1.,0.,0.));
#19045=DIRECTION('center_axis',(0.,0.,1.));
#19046=DIRECTION('ref_axis',(1.,0.,0.));
#19047=DIRECTION('center_axis',(0.,0.,-1.));
#19048=DIRECTION('ref_axis',(1.,0.,0.));
#19049=DIRECTION('',(0.,0.,-1.));
#19050=DIRECTION('center_axis',(0.,0.,1.));
#19051=DIRECTION('ref_axis',(1.,0.,0.));
#19052=DIRECTION('center_axis',(0.,0.,1.));
#19053=DIRECTION('ref_axis',(1.,-1.39943489555162E-12,0.));
#19054=DIRECTION('center_axis',(0.,0.,1.));
#19055=DIRECTION('ref_axis',(1.,0.,0.));
#19056=DIRECTION('center_axis',(0.,0.,-1.));
#19057=DIRECTION('ref_axis',(1.,0.,0.));
#19058=DIRECTION('center_axis',(0.,0.,-1.));
#19059=DIRECTION('ref_axis',(1.,0.,0.));
#19060=DIRECTION('',(0.,0.,-1.));
#19061=DIRECTION('center_axis',(0.,0.,1.));
#19062=DIRECTION('ref_axis',(1.,0.,0.));
#19063=DIRECTION('center_axis',(0.,0.,-1.));
#19064=DIRECTION('ref_axis',(1.,0.,0.));
#19065=DIRECTION('center_axis',(0.,0.,-1.));
#19066=DIRECTION('ref_axis',(1.,0.,0.));
#19067=DIRECTION('',(0.,0.,-1.));
#19068=DIRECTION('center_axis',(0.,0.,1.));
#19069=DIRECTION('ref_axis',(1.,0.,0.));
#19070=DIRECTION('center_axis',(0.,0.,-1.));
#19071=DIRECTION('ref_axis',(1.,0.,0.));
#19072=DIRECTION('center_axis',(0.,0.,-1.));
#19073=DIRECTION('ref_axis',(1.,0.,0.));
#19074=DIRECTION('',(0.,0.,-1.));
#19075=DIRECTION('center_axis',(0.,0.,1.));
#19076=DIRECTION('ref_axis',(1.,0.,0.));
#19077=DIRECTION('center_axis',(0.,0.,-1.));
#19078=DIRECTION('ref_axis',(1.,0.,0.));
#19079=DIRECTION('center_axis',(0.,0.,-1.));
#19080=DIRECTION('ref_axis',(1.,0.,0.));
#19081=DIRECTION('',(0.,0.,-1.));
#19082=DIRECTION('center_axis',(0.,0.,1.));
#19083=DIRECTION('ref_axis',(1.,0.,0.));
#19084=DIRECTION('center_axis',(0.,0.,-1.));
#19085=DIRECTION('ref_axis',(1.,0.,0.));
#19086=DIRECTION('center_axis',(0.,0.,-1.));
#19087=DIRECTION('ref_axis',(1.,0.,0.));
#19088=DIRECTION('',(0.,0.,-1.));
#19089=DIRECTION('center_axis',(0.,0.,1.));
#19090=DIRECTION('ref_axis',(1.,0.,0.));
#19091=DIRECTION('center_axis',(0.,0.,-1.));
#19092=DIRECTION('ref_axis',(1.,0.,0.));
#19093=DIRECTION('center_axis',(0.,0.,-1.));
#19094=DIRECTION('ref_axis',(1.,0.,0.));
#19095=DIRECTION('',(0.,0.,-1.));
#19096=DIRECTION('center_axis',(0.,0.,1.));
#19097=DIRECTION('ref_axis',(1.,0.,0.));
#19098=DIRECTION('center_axis',(0.,0.,1.));
#19099=DIRECTION('ref_axis',(1.,0.,0.));
#19100=DIRECTION('center_axis',(0.,0.,1.));
#19101=DIRECTION('ref_axis',(1.,0.,0.));
#19102=DIRECTION('center_axis',(0.,0.,1.));
#19103=DIRECTION('ref_axis',(1.,0.,0.));
#19104=DIRECTION('center_axis',(0.,0.,1.));
#19105=DIRECTION('ref_axis',(1.,0.,0.));
#19106=DIRECTION('center_axis',(0.,0.,1.));
#19107=DIRECTION('ref_axis',(1.,0.,0.));
#19108=DIRECTION('',(0.,0.,-1.));
#19109=DIRECTION('center_axis',(0.,0.,1.));
#19110=DIRECTION('ref_axis',(1.,0.,0.));
#19111=DIRECTION('center_axis',(0.,0.,1.));
#19112=DIRECTION('ref_axis',(1.,0.,0.));
#19113=DIRECTION('center_axis',(0.,0.,1.));
#19114=DIRECTION('ref_axis',(1.,0.,0.));
#19115=DIRECTION('center_axis',(0.,0.,1.));
#19116=DIRECTION('ref_axis',(1.,0.,0.));
#19117=DIRECTION('',(0.,0.,-1.));
#19118=DIRECTION('axis',(0.,0.,1.));
#19119=DIRECTION('refdir',(1.,0.,0.));
#19120=DIRECTION('center_axis',(0.,0.,1.));
#19121=DIRECTION('ref_axis',(1.,0.,0.));
#19122=DIRECTION('center_axis',(0.,0.,-1.));
#19123=DIRECTION('ref_axis',(1.,0.,0.));
#19124=DIRECTION('',(0.,0.,-1.));
#19125=DIRECTION('center_axis',(0.,0.,-1.));
#19126=DIRECTION('ref_axis',(1.,0.,0.));
#19127=DIRECTION('center_axis',(0.,0.,1.));
#19128=DIRECTION('ref_axis',(1.,0.,0.));
#19129=DIRECTION('center_axis',(0.,0.,1.));
#19130=DIRECTION('ref_axis',(1.,0.,0.));
#19131=DIRECTION('',(0.,0.,-1.));
#19132=DIRECTION('center_axis',(0.,0.,1.));
#19133=DIRECTION('ref_axis',(1.,0.,0.));
#19134=DIRECTION('center_axis',(0.,0.,1.));
#19135=DIRECTION('ref_axis',(1.,0.,0.));
#19136=DIRECTION('center_axis',(0.,0.,1.));
#19137=DIRECTION('ref_axis',(1.,0.,0.));
#19138=DIRECTION('axis',(0.,0.,1.));
#19139=DIRECTION('refdir',(1.,0.,0.));
#19140=DIRECTION('center_axis',(-1.,0.,0.));
#19141=DIRECTION('ref_axis',(0.,1.,0.));
#19142=DIRECTION('',(0.,0.,1.));
#19143=DIRECTION('',(0.,-1.,0.));
#19144=DIRECTION('',(0.,0.,-1.));
#19145=DIRECTION('',(0.,1.,0.));
#19146=DIRECTION('center_axis',(1.,0.,0.));
#19147=DIRECTION('ref_axis',(0.,-1.,0.));
#19148=DIRECTION('',(0.,0.,-1.));
#19149=DIRECTION('',(0.,-1.,0.));
#19150=DIRECTION('',(0.,0.,1.));
#19151=DIRECTION('',(0.,1.,0.));
#19152=DIRECTION('center_axis',(0.,0.,1.));
#19153=DIRECTION('ref_axis',(1.,0.,0.));
#19154=DIRECTION('center_axis',(0.,0.,1.));
#19155=DIRECTION('ref_axis',(1.,0.,0.));
#19156=DIRECTION('center_axis',(0.,0.,-1.));
#19157=DIRECTION('ref_axis',(1.,0.,0.));
#19158=DIRECTION('center_axis',(0.,0.,1.));
#19159=DIRECTION('ref_axis',(6.12323399573677E-17,-1.,0.));
#19160=DIRECTION('center_axis',(0.,0.,-1.));
#19161=DIRECTION('ref_axis',(1.,0.,0.));
#19162=DIRECTION('center_axis',(0.,0.,1.));
#19163=DIRECTION('ref_axis',(6.12323399573677E-17,-1.,0.));
#19164=DIRECTION('center_axis',(0.,0.,1.));
#19165=DIRECTION('ref_axis',(1.,0.,0.));
#19166=DIRECTION('center_axis',(0.,0.,1.));
#19167=DIRECTION('ref_axis',(1.,0.,0.));
#19168=DIRECTION('axis',(0.,0.,1.));
#19169=DIRECTION('refdir',(1.,0.,0.));
#19170=DIRECTION('center_axis',(0.,0.,1.));
#19171=DIRECTION('ref_axis',(1.,0.,0.));
#19172=DIRECTION('',(0.,0.,-1.));
#19173=DIRECTION('center_axis',(0.,0.,-1.));
#19174=DIRECTION('ref_axis',(1.,0.,0.));
#19175=DIRECTION('center_axis',(0.,0.,1.));
#19176=DIRECTION('ref_axis',(1.,0.,0.));
#19177=DIRECTION('',(0.,0.,-1.));
#19178=DIRECTION('center_axis',(0.,0.,1.));
#19179=DIRECTION('ref_axis',(1.,0.,0.));
#19180=DIRECTION('',(0.,0.,-1.));
#19181=DIRECTION('center_axis',(0.,0.,1.));
#19182=DIRECTION('ref_axis',(1.,0.,0.));
#19183=DIRECTION('',(0.,0.,-1.));
#19184=DIRECTION('center_axis',(0.,0.,1.));
#19185=DIRECTION('ref_axis',(1.,0.,0.));
#19186=DIRECTION('',(0.,0.,-1.));
#19187=DIRECTION('center_axis',(0.,0.,1.));
#19188=DIRECTION('ref_axis',(1.,0.,0.));
#19189=DIRECTION('',(0.,0.,-1.));
#19190=DIRECTION('center_axis',(0.,0.,1.));
#19191=DIRECTION('ref_axis',(1.,0.,0.));
#19192=DIRECTION('',(0.,0.,-1.));
#19193=DIRECTION('center_axis',(0.,0.,1.));
#19194=DIRECTION('ref_axis',(1.,0.,0.));
#19195=DIRECTION('',(0.,0.,-1.));
#19196=DIRECTION('center_axis',(0.,0.,1.));
#19197=DIRECTION('ref_axis',(1.,0.,0.));
#19198=DIRECTION('',(0.,0.,-1.));
#19199=DIRECTION('center_axis',(0.,0.,1.));
#19200=DIRECTION('ref_axis',(1.,0.,0.));
#19201=DIRECTION('',(0.,0.,-1.));
#19202=DIRECTION('center_axis',(0.,0.,1.));
#19203=DIRECTION('ref_axis',(1.,0.,0.));
#19204=DIRECTION('',(0.,0.,-1.));
#19205=DIRECTION('center_axis',(0.,0.,1.));
#19206=DIRECTION('ref_axis',(1.,0.,0.));
#19207=DIRECTION('',(0.,0.,-1.));
#19208=DIRECTION('center_axis',(0.,0.,1.));
#19209=DIRECTION('ref_axis',(1.,0.,0.));
#19210=DIRECTION('',(0.,0.,-1.));
#19211=DIRECTION('center_axis',(0.,0.,1.));
#19212=DIRECTION('ref_axis',(1.,0.,0.));
#19213=DIRECTION('',(0.,0.,-1.));
#19214=DIRECTION('center_axis',(0.,0.,1.));
#19215=DIRECTION('ref_axis',(1.,0.,0.));
#19216=DIRECTION('',(0.,0.,-1.));
#19217=DIRECTION('center_axis',(0.,0.,1.));
#19218=DIRECTION('ref_axis',(1.,0.,0.));
#19219=DIRECTION('',(0.,0.,-1.));
#19220=DIRECTION('center_axis',(0.,0.,1.));
#19221=DIRECTION('ref_axis',(1.,0.,0.));
#19222=DIRECTION('',(0.,0.,-1.));
#19223=DIRECTION('center_axis',(0.,0.,1.));
#19224=DIRECTION('ref_axis',(1.,0.,0.));
#19225=DIRECTION('',(0.,0.,-1.));
#19226=DIRECTION('center_axis',(0.,0.,1.));
#19227=DIRECTION('ref_axis',(-0.457769008694702,-0.889071164012572,0.));
#19228=DIRECTION('',(0.,0.,1.));
#19229=DIRECTION('center_axis',(0.,0.,1.));
#19230=DIRECTION('ref_axis',(1.,1.45731777125179E-13,0.));
#19231=DIRECTION('center_axis',(0.,0.,1.));
#19232=DIRECTION('ref_axis',(1.,1.45731777125179E-13,0.));
#19233=DIRECTION('',(0.,0.,1.));
#19234=DIRECTION('center_axis',(0.,0.,1.));
#19235=DIRECTION('ref_axis',(1.,1.45731777125179E-13,0.));
#19236=DIRECTION('',(0.,0.,1.));
#19237=DIRECTION('center_axis',(0.,0.,1.));
#19238=DIRECTION('ref_axis',(1.,1.45731777125179E-13,0.));
#19239=DIRECTION('',(0.,0.,1.));
#19240=DIRECTION('center_axis',(0.,0.,1.));
#19241=DIRECTION('ref_axis',(1.,1.45731777125179E-13,0.));
#19242=DIRECTION('',(0.,0.,1.));
#19243=DIRECTION('center_axis',(0.,0.,1.));
#19244=DIRECTION('ref_axis',(1.,1.45731777125179E-13,0.));
#19245=DIRECTION('',(0.,0.,1.));
#19246=DIRECTION('center_axis',(0.,0.,1.));
#19247=DIRECTION('ref_axis',(1.,1.45731777125179E-13,0.));
#19248=DIRECTION('',(0.,0.,1.));
#19249=DIRECTION('center_axis',(0.,0.,1.));
#19250=DIRECTION('ref_axis',(1.,1.45731777125179E-13,0.));
#19251=DIRECTION('',(0.,0.,1.));
#19252=DIRECTION('center_axis',(0.,0.,1.));
#19253=DIRECTION('ref_axis',(1.,1.45731777125179E-13,0.));
#19254=DIRECTION('',(0.,0.,1.));
#19255=DIRECTION('center_axis',(0.,0.,1.));
#19256=DIRECTION('ref_axis',(1.,1.45731777125179E-13,0.));
#19257=DIRECTION('',(0.,0.,1.));
#19258=DIRECTION('center_axis',(0.,0.,1.));
#19259=DIRECTION('ref_axis',(1.,1.45731777125179E-13,0.));
#19260=DIRECTION('',(0.,0.,1.));
#19261=DIRECTION('center_axis',(0.,0.,1.));
#19262=DIRECTION('ref_axis',(1.,1.45731777125179E-13,0.));
#19263=DIRECTION('',(0.,0.,1.));
#19264=DIRECTION('center_axis',(0.,0.,1.));
#19265=DIRECTION('ref_axis',(1.,1.45731777125179E-13,0.));
#19266=DIRECTION('',(0.,0.,1.));
#19267=DIRECTION('center_axis',(0.,0.,1.));
#19268=DIRECTION('ref_axis',(1.,1.45731777125179E-13,0.));
#19269=DIRECTION('',(0.,0.,1.));
#19270=DIRECTION('center_axis',(0.,0.,1.));
#19271=DIRECTION('ref_axis',(1.,1.45731777125179E-13,0.));
#19272=DIRECTION('',(0.,0.,1.));
#19273=DIRECTION('center_axis',(0.,0.,1.));
#19274=DIRECTION('ref_axis',(1.,1.45731777125179E-13,0.));
#19275=DIRECTION('',(0.,0.,1.));
#19276=DIRECTION('center_axis',(0.,0.,1.));
#19277=DIRECTION('ref_axis',(1.,1.45731777125179E-13,0.));
#19278=DIRECTION('',(0.,0.,1.));
#19279=DIRECTION('center_axis',(0.,0.,1.));
#19280=DIRECTION('ref_axis',(1.,1.45731777125179E-13,0.));
#19281=DIRECTION('',(0.,0.,1.));
#19282=DIRECTION('center_axis',(-1.60246890531964E-16,-1.,0.));
#19283=DIRECTION('ref_axis',(1.,-1.60246890531964E-16,0.));
#19284=DIRECTION('',(1.,-1.60246890531964E-16,0.));
#19285=DIRECTION('',(0.,0.,1.));
#19286=DIRECTION('',(1.,-1.60246890531964E-16,0.));
#19287=DIRECTION('',(0.,0.,1.));
#19288=DIRECTION('center_axis',(-0.866025403784439,-0.5,0.));
#19289=DIRECTION('ref_axis',(0.5,-0.866025403784439,0.));
#19290=DIRECTION('',(0.5,-0.866025403784439,0.));
#19291=DIRECTION('',(0.,0.,1.));
#19292=DIRECTION('',(0.5,-0.866025403784439,0.));
#19293=DIRECTION('center_axis',(-0.866025403784439,0.5,0.));
#19294=DIRECTION('ref_axis',(-0.5,-0.866025403784439,0.));
#19295=DIRECTION('',(-0.5,-0.866025403784439,0.));
#19296=DIRECTION('',(0.,0.,1.));
#19297=DIRECTION('',(-0.5,-0.866025403784439,0.));
#19298=DIRECTION('center_axis',(1.60246890531964E-16,1.,0.));
#19299=DIRECTION('ref_axis',(-1.,1.60246890531964E-16,0.));
#19300=DIRECTION('',(-1.,1.60246890531964E-16,0.));
#19301=DIRECTION('',(0.,0.,1.));
#19302=DIRECTION('',(-1.,1.60246890531964E-16,0.));
#19303=DIRECTION('center_axis',(0.866025403784439,0.5,0.));
#19304=DIRECTION('ref_axis',(-0.5,0.866025403784439,0.));
#19305=DIRECTION('',(-0.5,0.866025403784439,0.));
#19306=DIRECTION('',(0.,0.,1.));
#19307=DIRECTION('',(-0.5,0.866025403784439,0.));
#19308=DIRECTION('center_axis',(0.866025403784439,-0.5,0.));
#19309=DIRECTION('ref_axis',(0.5,0.866025403784439,0.));
#19310=DIRECTION('',(0.5,0.866025403784439,0.));
#19311=DIRECTION('',(0.5,0.866025403784439,0.));
#19312=DIRECTION('center_axis',(0.,0.,1.));
#19313=DIRECTION('ref_axis',(1.,0.,0.));
#19314=DIRECTION('center_axis',(0.,0.,1.));
#19315=DIRECTION('ref_axis',(1.,1.45731777125179E-13,0.));
#19316=DIRECTION('center_axis',(0.,0.,-1.));
#19317=DIRECTION('ref_axis',(1.,1.45731777125179E-13,0.));
#19318=DIRECTION('center_axis',(0.,0.,1.));
#19319=DIRECTION('ref_axis',(1.,0.,0.));
#19320=DIRECTION('center_axis',(0.,0.,-1.));
#19321=DIRECTION('ref_axis',(1.,0.,0.));
#19322=DIRECTION('center_axis',(0.,0.,1.));
#19323=DIRECTION('ref_axis',(1.,0.,0.));
#19324=DIRECTION('center_axis',(0.,0.,1.));
#19325=DIRECTION('ref_axis',(1.,0.,0.));
#19326=DIRECTION('axis',(0.,0.,1.));
#19327=DIRECTION('refdir',(1.,0.,0.));
#19328=DIRECTION('center_axis',(0.,0.,-1.));
#19329=DIRECTION('ref_axis',(1.,0.,0.));
#19330=DIRECTION('center_axis',(0.,0.,-1.));
#19331=DIRECTION('ref_axis',(1.,0.,0.));
#19332=DIRECTION('center_axis',(0.,0.,-1.));
#19333=DIRECTION('ref_axis',(1.,0.,0.));
#19334=DIRECTION('center_axis',(0.,0.,-1.));
#19335=DIRECTION('ref_axis',(1.,0.,0.));
#19336=DIRECTION('center_axis',(0.,0.,-1.));
#19337=DIRECTION('ref_axis',(1.,0.,0.));
#19338=DIRECTION('',(0.,0.,-1.));
#19339=DIRECTION('center_axis',(0.,0.,-1.));
#19340=DIRECTION('ref_axis',(1.,0.,0.));
#19341=DIRECTION('',(0.,0.,-1.));
#19342=DIRECTION('center_axis',(0.,0.,1.));
#19343=DIRECTION('ref_axis',(1.,0.,0.));
#19344=DIRECTION('center_axis',(0.,0.,-1.));
#19345=DIRECTION('ref_axis',(1.,0.,0.));
#19346=DIRECTION('center_axis',(0.,0.,-1.));
#19347=DIRECTION('ref_axis',(1.,0.,0.));
#19348=DIRECTION('center_axis',(0.,0.,-1.));
#19349=DIRECTION('ref_axis',(1.,0.,0.));
#19350=DIRECTION('center_axis',(0.,0.,-1.));
#19351=DIRECTION('ref_axis',(1.,0.,0.));
#19352=DIRECTION('center_axis',(0.,0.,-1.));
#19353=DIRECTION('ref_axis',(1.,0.,0.));
#19354=DIRECTION('',(0.,0.,-1.));
#19355=DIRECTION('center_axis',(0.,0.,-1.));
#19356=DIRECTION('ref_axis',(1.,0.,0.));
#19357=DIRECTION('',(0.,0.,-1.));
#19358=DIRECTION('center_axis',(0.,0.,1.));
#19359=DIRECTION('ref_axis',(1.,0.,0.));
#19360=DIRECTION('center_axis',(0.,0.,-1.));
#19361=DIRECTION('ref_axis',(1.,0.,0.));
#19362=DIRECTION('center_axis',(0.,0.,-1.));
#19363=DIRECTION('ref_axis',(1.,0.,0.));
#19364=DIRECTION('center_axis',(0.,0.,-1.));
#19365=DIRECTION('ref_axis',(1.,0.,0.));
#19366=DIRECTION('center_axis',(0.,0.,-1.));
#19367=DIRECTION('ref_axis',(1.,0.,0.));
#19368=DIRECTION('center_axis',(0.,0.,-1.));
#19369=DIRECTION('ref_axis',(1.,0.,0.));
#19370=DIRECTION('',(0.,0.,-1.));
#19371=DIRECTION('center_axis',(0.,0.,-1.));
#19372=DIRECTION('ref_axis',(1.,0.,0.));
#19373=DIRECTION('',(0.,0.,-1.));
#19374=DIRECTION('center_axis',(0.,0.,1.));
#19375=DIRECTION('ref_axis',(1.,0.,0.));
#19376=DIRECTION('center_axis',(0.,0.,-1.));
#19377=DIRECTION('ref_axis',(1.,0.,0.));
#19378=DIRECTION('center_axis',(0.,0.,-1.));
#19379=DIRECTION('ref_axis',(1.,0.,0.));
#19380=DIRECTION('center_axis',(0.,0.,-1.));
#19381=DIRECTION('ref_axis',(1.,0.,0.));
#19382=DIRECTION('center_axis',(0.,0.,-1.));
#19383=DIRECTION('ref_axis',(1.,0.,0.));
#19384=DIRECTION('center_axis',(0.,0.,-1.));
#19385=DIRECTION('ref_axis',(1.,0.,0.));
#19386=DIRECTION('',(0.,0.,-1.));
#19387=DIRECTION('center_axis',(0.,0.,-1.));
#19388=DIRECTION('ref_axis',(1.,0.,0.));
#19389=DIRECTION('',(0.,0.,-1.));
#19390=DIRECTION('center_axis',(0.,0.,1.));
#19391=DIRECTION('ref_axis',(1.,0.,0.));
#19392=DIRECTION('center_axis',(0.,0.,1.));
#19393=DIRECTION('ref_axis',(1.,0.,0.));
#19394=DIRECTION('center_axis',(0.,0.,-1.));
#19395=DIRECTION('ref_axis',(1.,0.,0.));
#19396=DIRECTION('',(0.,0.,-1.));
#19397=DIRECTION('center_axis',(0.,0.,-1.));
#19398=DIRECTION('ref_axis',(1.,0.,0.));
#19399=DIRECTION('center_axis',(0.,0.,1.));
#19400=DIRECTION('ref_axis',(1.,0.,0.));
#19401=DIRECTION('center_axis',(0.,0.,1.));
#19402=DIRECTION('ref_axis',(1.,0.,0.));
#19403=DIRECTION('',(0.,0.,-1.));
#19404=DIRECTION('center_axis',(0.,0.,1.));
#19405=DIRECTION('ref_axis',(1.,0.,0.));
#19406=DIRECTION('center_axis',(0.,0.,1.));
#19407=DIRECTION('ref_axis',(1.,0.,0.));
#19408=DIRECTION('center_axis',(0.,0.,1.));
#19409=DIRECTION('ref_axis',(1.,0.,0.));
#19410=DIRECTION('axis',(0.,0.,1.));
#19411=DIRECTION('refdir',(1.,0.,0.));
#19412=DIRECTION('center_axis',(0.,0.,1.));
#19413=DIRECTION('ref_axis',(1.,0.,0.));
#19414=DIRECTION('center_axis',(0.,0.,1.));
#19415=DIRECTION('ref_axis',(1.,0.,0.));
#19416=DIRECTION('center_axis',(-1.22464679914735E-16,1.,0.));
#19417=DIRECTION('ref_axis',(-1.,-1.22464679914735E-16,0.));
#19418=DIRECTION('center_axis',(0.,0.,-1.));
#19419=DIRECTION('ref_axis',(1.,0.,0.));
#19420=DIRECTION('center_axis',(0.,0.,1.));
#19421=DIRECTION('ref_axis',(1.,0.,0.));
#19422=DIRECTION('',(0.,0.,-1.));
#19423=DIRECTION('center_axis',(0.,0.,1.));
#19424=DIRECTION('ref_axis',(1.,0.,0.));
#19425=DIRECTION('center_axis',(0.,0.,1.));
#19426=DIRECTION('ref_axis',(1.,0.,0.));
#19427=DIRECTION('center_axis',(0.,0.,-1.));
#19428=DIRECTION('ref_axis',(1.,0.,0.));
#19429=DIRECTION('',(0.,0.,-1.));
#19430=DIRECTION('center_axis',(0.,0.,-1.));
#19431=DIRECTION('ref_axis',(1.,0.,0.));
#19432=DIRECTION('center_axis',(0.,0.,1.));
#19433=DIRECTION('ref_axis',(1.,0.,0.));
#19434=DIRECTION('center_axis',(0.,0.,1.));
#19435=DIRECTION('ref_axis',(1.,0.,0.));
#19436=DIRECTION('',(0.,0.,-1.));
#19437=DIRECTION('center_axis',(0.,0.,1.));
#19438=DIRECTION('ref_axis',(1.,0.,0.));
#19439=DIRECTION('center_axis',(0.,0.,1.));
#19440=DIRECTION('ref_axis',(1.,0.,0.));
#19441=DIRECTION('axis',(0.,0.,1.));
#19442=DIRECTION('refdir',(1.,0.,0.));
#19443=DIRECTION('center_axis',(0.,0.,1.));
#19444=DIRECTION('ref_axis',(1.,0.,0.));
#19445=DIRECTION('center_axis',(0.,0.,1.));
#19446=DIRECTION('ref_axis',(1.,0.,0.));
#19447=DIRECTION('center_axis',(-1.22464679914735E-16,1.,0.));
#19448=DIRECTION('ref_axis',(-1.,-1.22464679914735E-16,0.));
#19449=DIRECTION('center_axis',(0.,0.,-1.));
#19450=DIRECTION('ref_axis',(1.,0.,0.));
#19451=DIRECTION('center_axis',(0.,0.,1.));
#19452=DIRECTION('ref_axis',(1.,0.,0.));
#19453=DIRECTION('center_axis',(0.,0.,-1.));
#19454=DIRECTION('ref_axis',(1.,0.,0.));
#19455=DIRECTION('',(0.,0.,-1.));
#19456=DIRECTION('center_axis',(0.,0.,1.));
#19457=DIRECTION('ref_axis',(1.,0.,0.));
#19458=DIRECTION('',(0.,0.,-1.));
#19459=DIRECTION('center_axis',(0.,0.,-1.));
#19460=DIRECTION('ref_axis',(1.,0.,0.));
#19461=DIRECTION('center_axis',(0.,0.,1.));
#19462=DIRECTION('ref_axis',(1.,0.,0.));
#19463=DIRECTION('center_axis',(0.,0.,1.));
#19464=DIRECTION('ref_axis',(1.,0.,0.));
#19465=DIRECTION('',(0.,0.,-1.));
#19466=DIRECTION('center_axis',(0.,0.,1.));
#19467=DIRECTION('ref_axis',(1.,0.,0.));
#19468=DIRECTION('center_axis',(0.,0.,1.));
#19469=DIRECTION('ref_axis',(1.,0.,0.));
#19470=DIRECTION('center_axis',(0.,0.,1.));
#19471=DIRECTION('ref_axis',(1.,0.,0.));
#19472=DIRECTION('axis',(0.,0.,1.));
#19473=DIRECTION('refdir',(1.,0.,0.));
#19474=DIRECTION('center_axis',(6.12323399573677E-17,0.,1.));
#19475=DIRECTION('ref_axis',(1.,0.,0.));
#19476=DIRECTION('center_axis',(1.22464679914735E-16,-1.,0.));
#19477=DIRECTION('ref_axis',(-1.,-1.22464679914735E-16,0.));
#19478=DIRECTION('axis',(0.,0.,1.));
#19479=DIRECTION('refdir',(1.,0.,0.));
#19480=DIRECTION('center_axis',(0.,0.,1.));
#19481=DIRECTION('ref_axis',(1.,0.,0.));
#19482=DIRECTION('center_axis',(0.,0.,1.));
#19483=DIRECTION('ref_axis',(0.,-1.,0.));
#19484=DIRECTION('center_axis',(0.,1.,0.));
#19485=DIRECTION('ref_axis',(-1.,0.,0.));
#19486=DIRECTION('center_axis',(0.,0.,1.));
#19487=DIRECTION('ref_axis',(0.,-1.,0.));
#19488=DIRECTION('center_axis',(0.,0.,1.));
#19489=DIRECTION('ref_axis',(1.,0.,0.));
#19490=DIRECTION('center_axis',(0.,0.,-1.));
#19491=DIRECTION('ref_axis',(1.,0.,0.));
#19492=DIRECTION('',(0.,0.,-1.));
#19493=DIRECTION('center_axis',(0.,0.,-1.));
#19494=DIRECTION('ref_axis',(1.,0.,0.));
#19495=DIRECTION('center_axis',(0.,0.,-1.));
#19496=DIRECTION('ref_axis',(1.,0.,0.));
#19497=DIRECTION('center_axis',(0.,0.,-1.));
#19498=DIRECTION('ref_axis',(1.,0.,0.));
#19499=DIRECTION('center_axis',(0.,0.,-1.));
#19500=DIRECTION('ref_axis',(1.,0.,0.));
#19501=DIRECTION('center_axis',(0.,0.,-1.));
#19502=DIRECTION('ref_axis',(1.,0.,0.));
#19503=DIRECTION('center_axis',(0.,0.,-1.));
#19504=DIRECTION('ref_axis',(1.,0.,0.));
#19505=DIRECTION('center_axis',(0.,0.,-1.));
#19506=DIRECTION('ref_axis',(1.,0.,0.));
#19507=DIRECTION('center_axis',(0.,0.,-1.));
#19508=DIRECTION('ref_axis',(1.,0.,0.));
#19509=DIRECTION('center_axis',(0.,0.,-1.));
#19510=DIRECTION('ref_axis',(1.,0.,0.));
#19511=DIRECTION('center_axis',(0.,0.,-1.));
#19512=DIRECTION('ref_axis',(1.,0.,0.));
#19513=DIRECTION('center_axis',(0.,0.,-1.));
#19514=DIRECTION('ref_axis',(1.,0.,0.));
#19515=DIRECTION('center_axis',(0.,0.,-1.));
#19516=DIRECTION('ref_axis',(1.,0.,0.));
#19517=DIRECTION('center_axis',(0.,0.,1.));
#19518=DIRECTION('ref_axis',(1.,0.,0.));
#19519=DIRECTION('center_axis',(0.,0.,1.));
#19520=DIRECTION('ref_axis',(1.,0.,0.));
#19521=DIRECTION('center_axis',(0.,0.,1.));
#19522=DIRECTION('ref_axis',(0.,-1.,0.));
#19523=DIRECTION('center_axis',(0.,0.,1.));
#19524=DIRECTION('ref_axis',(1.,0.,0.));
#19525=DIRECTION('center_axis',(0.,0.,1.));
#19526=DIRECTION('ref_axis',(0.,-1.,0.));
#19527=DIRECTION('center_axis',(0.,1.,0.));
#19528=DIRECTION('ref_axis',(-1.,0.,0.));
#19529=DIRECTION('center_axis',(0.,0.,1.));
#19530=DIRECTION('ref_axis',(1.,0.,0.));
#19531=DIRECTION('center_axis',(0.,0.,1.));
#19532=DIRECTION('ref_axis',(1.,0.,0.));
#19533=DIRECTION('center_axis',(0.,0.,1.));
#19534=DIRECTION('ref_axis',(0.,-1.,0.));
#19535=DIRECTION('center_axis',(6.12323399573677E-17,0.,1.));
#19536=DIRECTION('ref_axis',(1.,0.,0.));
#19537=DIRECTION('center_axis',(0.,0.,1.));
#19538=DIRECTION('ref_axis',(0.,-1.,0.));
#19539=DIRECTION('center_axis',(0.,1.,0.));
#19540=DIRECTION('ref_axis',(-1.,0.,0.));
#19541=DIRECTION('center_axis',(0.,0.,1.));
#19542=DIRECTION('ref_axis',(0.,-1.,0.));
#19543=DIRECTION('center_axis',(0.,0.,1.));
#19544=DIRECTION('ref_axis',(1.,0.,0.));
#19545=DIRECTION('center_axis',(0.,0.,1.));
#19546=DIRECTION('ref_axis',(1.,0.,0.));
#19547=DIRECTION('center_axis',(0.,0.,1.));
#19548=DIRECTION('ref_axis',(0.,-1.,0.));
#19549=DIRECTION('center_axis',(0.,0.,1.));
#19550=DIRECTION('ref_axis',(1.,0.,0.));
#19551=DIRECTION('center_axis',(0.,0.,1.));
#19552=DIRECTION('ref_axis',(0.,-1.,0.));
#19553=DIRECTION('center_axis',(0.,1.,0.));
#19554=DIRECTION('ref_axis',(-1.,0.,0.));
#19555=DIRECTION('center_axis',(0.,0.,1.));
#19556=DIRECTION('ref_axis',(1.,0.,0.));
#19557=DIRECTION('center_axis',(0.,0.,1.));
#19558=DIRECTION('ref_axis',(1.,0.,0.));
#19559=DIRECTION('center_axis',(0.,0.,1.));
#19560=DIRECTION('ref_axis',(0.,-1.,0.));
#19561=DIRECTION('center_axis',(0.,0.,1.));
#19562=DIRECTION('ref_axis',(1.,0.,0.));
#19563=DIRECTION('center_axis',(0.,0.,1.));
#19564=DIRECTION('ref_axis',(0.,-1.,0.));
#19565=DIRECTION('center_axis',(0.,1.,0.));
#19566=DIRECTION('ref_axis',(-1.,0.,0.));
#19567=DIRECTION('center_axis',(0.,0.,1.));
#19568=DIRECTION('ref_axis',(1.,0.,0.));
#19569=DIRECTION('center_axis',(0.,0.,1.));
#19570=DIRECTION('ref_axis',(1.,0.,0.));
#19571=DIRECTION('center_axis',(0.,0.,1.));
#19572=DIRECTION('ref_axis',(0.,-1.,0.));
#19573=DIRECTION('center_axis',(0.,0.,1.));
#19574=DIRECTION('ref_axis',(1.,0.,0.));
#19575=DIRECTION('center_axis',(0.,0.,1.));
#19576=DIRECTION('ref_axis',(0.,-1.,0.));
#19577=DIRECTION('center_axis',(-1.22464679914735E-16,1.,0.));
#19578=DIRECTION('ref_axis',(-1.,-1.22464679914735E-16,0.));
#19579=DIRECTION('center_axis',(0.,0.,1.));
#19580=DIRECTION('ref_axis',(1.,0.,0.));
#19581=DIRECTION('center_axis',(0.,0.,1.));
#19582=DIRECTION('ref_axis',(1.,0.,0.));
#19583=DIRECTION('center_axis',(0.,0.,1.));
#19584=DIRECTION('ref_axis',(0.,-1.,0.));
#19585=DIRECTION('center_axis',(0.,0.,1.));
#19586=DIRECTION('ref_axis',(1.,0.,0.));
#19587=DIRECTION('center_axis',(0.,0.,1.));
#19588=DIRECTION('ref_axis',(0.,-1.,0.));
#19589=DIRECTION('center_axis',(0.,1.,0.));
#19590=DIRECTION('ref_axis',(-1.,0.,0.));
#19591=DIRECTION('center_axis',(0.,0.,1.));
#19592=DIRECTION('ref_axis',(1.,0.,0.));
#19593=DIRECTION('center_axis',(0.,0.,1.));
#19594=DIRECTION('ref_axis',(1.,0.,0.));
#19595=DIRECTION('center_axis',(0.,0.,1.));
#19596=DIRECTION('ref_axis',(0.,-1.,0.));
#19597=DIRECTION('center_axis',(0.,0.,1.));
#19598=DIRECTION('ref_axis',(1.,0.,0.));
#19599=DIRECTION('center_axis',(0.,0.,1.));
#19600=DIRECTION('ref_axis',(0.,-1.,0.));
#19601=DIRECTION('center_axis',(0.,1.,0.));
#19602=DIRECTION('ref_axis',(-1.,0.,0.));
#19603=DIRECTION('center_axis',(0.,0.,1.));
#19604=DIRECTION('ref_axis',(1.,0.,0.));
#19605=DIRECTION('center_axis',(0.,0.,1.));
#19606=DIRECTION('ref_axis',(1.,0.,0.));
#19607=DIRECTION('center_axis',(0.,0.,1.));
#19608=DIRECTION('ref_axis',(0.,-1.,0.));
#19609=DIRECTION('center_axis',(0.,0.,1.));
#19610=DIRECTION('ref_axis',(0.,-1.,0.));
#19611=DIRECTION('center_axis',(6.12323399573677E-17,0.,1.));
#19612=DIRECTION('ref_axis',(1.,0.,0.));
#19613=DIRECTION('center_axis',(0.,0.,1.));
#19614=DIRECTION('ref_axis',(0.,-1.,0.));
#19615=DIRECTION('center_axis',(0.,1.,0.));
#19616=DIRECTION('ref_axis',(-1.,0.,0.));
#19617=DIRECTION('center_axis',(0.,0.,1.));
#19618=DIRECTION('ref_axis',(1.,0.,0.));
#19619=DIRECTION('center_axis',(0.,0.,1.));
#19620=DIRECTION('ref_axis',(1.,0.,0.));
#19621=DIRECTION('center_axis',(0.,0.,1.));
#19622=DIRECTION('ref_axis',(0.,-1.,0.));
#19623=DIRECTION('center_axis',(0.,0.,1.));
#19624=DIRECTION('ref_axis',(1.,0.,0.));
#19625=DIRECTION('center_axis',(0.,0.,1.));
#19626=DIRECTION('ref_axis',(0.,-1.,0.));
#19627=DIRECTION('center_axis',(0.,1.,0.));
#19628=DIRECTION('ref_axis',(-1.,0.,0.));
#19629=DIRECTION('center_axis',(0.,0.,1.));
#19630=DIRECTION('ref_axis',(1.,0.,0.));
#19631=DIRECTION('center_axis',(0.,0.,1.));
#19632=DIRECTION('ref_axis',(1.,0.,0.));
#19633=DIRECTION('center_axis',(0.,0.,1.));
#19634=DIRECTION('ref_axis',(0.,-1.,0.));
#19635=DIRECTION('center_axis',(0.,0.,1.));
#19636=DIRECTION('ref_axis',(1.,0.,0.));
#19637=DIRECTION('center_axis',(0.,0.,1.));
#19638=DIRECTION('ref_axis',(0.,-1.,0.));
#19639=DIRECTION('center_axis',(0.,1.,0.));
#19640=DIRECTION('ref_axis',(-1.,0.,0.));
#19641=DIRECTION('center_axis',(0.,0.,1.));
#19642=DIRECTION('ref_axis',(1.,0.,0.));
#19643=DIRECTION('center_axis',(0.,0.,1.));
#19644=DIRECTION('ref_axis',(1.,0.,0.));
#19645=DIRECTION('center_axis',(0.,0.,1.));
#19646=DIRECTION('ref_axis',(0.,-1.,0.));
#19647=DIRECTION('center_axis',(0.,0.,1.));
#19648=DIRECTION('ref_axis',(1.,0.,0.));
#19649=DIRECTION('center_axis',(0.,0.,1.));
#19650=DIRECTION('ref_axis',(0.,-1.,0.));
#19651=DIRECTION('center_axis',(-1.22464679914735E-16,1.,0.));
#19652=DIRECTION('ref_axis',(-1.,-1.22464679914735E-16,0.));
#19653=DIRECTION('center_axis',(0.,0.,1.));
#19654=DIRECTION('ref_axis',(1.,0.,0.));
#19655=DIRECTION('center_axis',(0.,0.,1.));
#19656=DIRECTION('ref_axis',(1.,0.,0.));
#19657=DIRECTION('',(0.,0.,-1.));
#19658=DIRECTION('center_axis',(0.,0.,1.));
#19659=DIRECTION('ref_axis',(1.,0.,0.));
#19660=DIRECTION('center_axis',(0.,0.,1.));
#19661=DIRECTION('ref_axis',(1.,0.,0.));
#19662=DIRECTION('center_axis',(0.,0.,1.));
#19663=DIRECTION('ref_axis',(1.,0.,0.));
#19664=DIRECTION('axis',(0.,0.,1.));
#19665=DIRECTION('refdir',(1.,0.,0.));
#19666=DIRECTION('center_axis',(0.,0.,1.));
#19667=DIRECTION('ref_axis',(1.,0.,0.));
#19668=DIRECTION('center_axis',(0.,0.,-1.));
#19669=DIRECTION('ref_axis',(1.,0.,0.));
#19670=DIRECTION('',(0.,0.,-1.));
#19671=DIRECTION('center_axis',(0.,0.,-1.));
#19672=DIRECTION('ref_axis',(1.,0.,0.));
#19673=DIRECTION('center_axis',(0.,0.,1.));
#19674=DIRECTION('ref_axis',(1.,0.,0.));
#19675=DIRECTION('center_axis',(0.,0.,1.));
#19676=DIRECTION('ref_axis',(1.,0.,0.));
#19677=DIRECTION('',(0.,0.,-1.));
#19678=DIRECTION('center_axis',(0.,0.,1.));
#19679=DIRECTION('ref_axis',(1.,0.,0.));
#19680=DIRECTION('center_axis',(0.,0.,1.));
#19681=DIRECTION('ref_axis',(1.,0.,0.));
#19682=DIRECTION('center_axis',(0.,0.,1.));
#19683=DIRECTION('ref_axis',(1.,0.,0.));
#19684=DIRECTION('axis',(0.,0.,1.));
#19685=DIRECTION('refdir',(1.,0.,0.));
#19686=DIRECTION('center_axis',(0.,0.,1.));
#19687=DIRECTION('ref_axis',(1.,0.,0.));
#19688=DIRECTION('',(0.,0.,-1.));
#19689=DIRECTION('center_axis',(0.,0.,-1.));
#19690=DIRECTION('ref_axis',(1.,0.,0.));
#19691=DIRECTION('center_axis',(0.,0.,1.));
#19692=DIRECTION('ref_axis',(1.,0.,0.));
#19693=DIRECTION('',(0.,0.,-1.));
#19694=DIRECTION('center_axis',(0.,0.,1.));
#19695=DIRECTION('ref_axis',(1.,0.,0.));
#19696=DIRECTION('',(0.,0.,-1.));
#19697=DIRECTION('center_axis',(0.,0.,1.));
#19698=DIRECTION('ref_axis',(1.,0.,0.));
#19699=DIRECTION('',(0.,0.,-1.));
#19700=DIRECTION('center_axis',(0.,0.,1.));
#19701=DIRECTION('ref_axis',(1.,0.,0.));
#19702=DIRECTION('',(0.,0.,-1.));
#19703=DIRECTION('center_axis',(0.,0.,1.));
#19704=DIRECTION('ref_axis',(1.,0.,0.));
#19705=DIRECTION('',(0.,0.,-1.));
#19706=DIRECTION('center_axis',(0.,0.,1.));
#19707=DIRECTION('ref_axis',(1.,0.,0.));
#19708=DIRECTION('',(0.,0.,-1.));
#19709=DIRECTION('center_axis',(0.,0.,1.));
#19710=DIRECTION('ref_axis',(1.,0.,0.));
#19711=DIRECTION('',(0.,0.,-1.));
#19712=DIRECTION('center_axis',(0.,0.,1.));
#19713=DIRECTION('ref_axis',(1.,0.,0.));
#19714=DIRECTION('',(0.,0.,-1.));
#19715=DIRECTION('center_axis',(0.,0.,1.));
#19716=DIRECTION('ref_axis',(1.,0.,0.));
#19717=DIRECTION('',(0.,0.,-1.));
#19718=DIRECTION('center_axis',(0.,0.,1.));
#19719=DIRECTION('ref_axis',(1.,0.,0.));
#19720=DIRECTION('',(0.,0.,-1.));
#19721=DIRECTION('center_axis',(0.,0.,1.));
#19722=DIRECTION('ref_axis',(1.,0.,0.));
#19723=DIRECTION('',(0.,0.,-1.));
#19724=DIRECTION('center_axis',(0.,0.,1.));
#19725=DIRECTION('ref_axis',(1.,0.,0.));
#19726=DIRECTION('',(0.,0.,-1.));
#19727=DIRECTION('center_axis',(0.,0.,1.));
#19728=DIRECTION('ref_axis',(1.,0.,0.));
#19729=DIRECTION('',(0.,0.,-1.));
#19730=DIRECTION('center_axis',(0.,0.,1.));
#19731=DIRECTION('ref_axis',(1.,0.,0.));
#19732=DIRECTION('',(0.,0.,-1.));
#19733=DIRECTION('center_axis',(0.,0.,1.));
#19734=DIRECTION('ref_axis',(1.,0.,0.));
#19735=DIRECTION('',(0.,0.,-1.));
#19736=DIRECTION('center_axis',(0.,0.,1.));
#19737=DIRECTION('ref_axis',(1.,1.29731060939901E-13,0.));
#19738=DIRECTION('',(0.,0.,1.));
#19739=DIRECTION('center_axis',(0.,0.,-1.));
#19740=DIRECTION('ref_axis',(1.,1.29731060939901E-13,0.));
#19741=DIRECTION('center_axis',(0.,0.,1.));
#19742=DIRECTION('ref_axis',(1.,1.29731060939901E-13,0.));
#19743=DIRECTION('',(0.,0.,1.));
#19744=DIRECTION('center_axis',(0.,0.,1.));
#19745=DIRECTION('ref_axis',(1.,1.29731060939901E-13,0.));
#19746=DIRECTION('',(0.,0.,1.));
#19747=DIRECTION('center_axis',(0.,0.,1.));
#19748=DIRECTION('ref_axis',(1.,1.29731060939901E-13,0.));
#19749=DIRECTION('',(0.,0.,1.));
#19750=DIRECTION('center_axis',(0.,0.,1.));
#19751=DIRECTION('ref_axis',(1.,1.29731060939901E-13,0.));
#19752=DIRECTION('',(0.,0.,1.));
#19753=DIRECTION('center_axis',(0.,0.,1.));
#19754=DIRECTION('ref_axis',(1.,1.29731060939901E-13,0.));
#19755=DIRECTION('',(0.,0.,1.));
#19756=DIRECTION('center_axis',(0.,0.,1.));
#19757=DIRECTION('ref_axis',(1.,1.29731060939901E-13,0.));
#19758=DIRECTION('',(0.,0.,1.));
#19759=DIRECTION('center_axis',(0.,0.,1.));
#19760=DIRECTION('ref_axis',(1.,1.29731060939901E-13,0.));
#19761=DIRECTION('',(0.,0.,1.));
#19762=DIRECTION('center_axis',(0.,0.,1.));
#19763=DIRECTION('ref_axis',(1.,1.29731060939901E-13,0.));
#19764=DIRECTION('',(0.,0.,1.));
#19765=DIRECTION('center_axis',(0.,0.,1.));
#19766=DIRECTION('ref_axis',(1.,1.29731060939901E-13,0.));
#19767=DIRECTION('',(0.,0.,1.));
#19768=DIRECTION('center_axis',(0.,0.,1.));
#19769=DIRECTION('ref_axis',(1.,1.29731060939901E-13,0.));
#19770=DIRECTION('',(0.,0.,1.));
#19771=DIRECTION('center_axis',(0.,0.,1.));
#19772=DIRECTION('ref_axis',(1.,1.29731060939901E-13,0.));
#19773=DIRECTION('',(0.,0.,1.));
#19774=DIRECTION('center_axis',(0.,0.,1.));
#19775=DIRECTION('ref_axis',(1.,1.29731060939901E-13,0.));
#19776=DIRECTION('',(0.,0.,1.));
#19777=DIRECTION('center_axis',(0.,0.,1.));
#19778=DIRECTION('ref_axis',(1.,1.29731060939901E-13,0.));
#19779=DIRECTION('',(0.,0.,1.));
#19780=DIRECTION('center_axis',(0.,0.,1.));
#19781=DIRECTION('ref_axis',(1.,1.29731060939901E-13,0.));
#19782=DIRECTION('',(0.,0.,1.));
#19783=DIRECTION('center_axis',(0.,0.,1.));
#19784=DIRECTION('ref_axis',(1.,1.29731060939901E-13,0.));
#19785=DIRECTION('',(0.,0.,1.));
#19786=DIRECTION('center_axis',(0.,0.,-1.));
#19787=DIRECTION('ref_axis',(1.,0.,0.));
#19788=DIRECTION('center_axis',(0.,0.,-1.));
#19789=DIRECTION('ref_axis',(1.,0.,0.));
#19790=DIRECTION('',(0.707106781186548,8.65956056235494E-17,0.707106781186547));
#19791=DIRECTION('center_axis',(0.,0.,1.));
#19792=DIRECTION('ref_axis',(1.,0.,0.));
#19793=DIRECTION('center_axis',(0.,0.,1.));
#19794=DIRECTION('ref_axis',(1.,1.29731060939901E-13,0.));
#19795=DIRECTION('center_axis',(0.,0.,-1.));
#19796=DIRECTION('ref_axis',(1.,1.29731060939901E-13,0.));
#19797=DIRECTION('center_axis',(0.,0.,1.));
#19798=DIRECTION('ref_axis',(1.,0.,0.));
#19799=DIRECTION('center_axis',(-1.60246890531964E-16,-1.,0.));
#19800=DIRECTION('ref_axis',(1.,-1.60246890531964E-16,0.));
#19801=DIRECTION('',(1.,-1.60246890531964E-16,0.));
#19802=DIRECTION('',(0.,0.,1.));
#19803=DIRECTION('',(1.,-1.60246890531964E-16,0.));
#19804=DIRECTION('',(0.,0.,1.));
#19805=DIRECTION('center_axis',(-0.866025403784439,-0.5,0.));
#19806=DIRECTION('ref_axis',(0.5,-0.866025403784439,0.));
#19807=DIRECTION('',(0.5,-0.866025403784439,0.));
#19808=DIRECTION('',(0.,0.,1.));
#19809=DIRECTION('',(0.5,-0.866025403784439,0.));
#19810=DIRECTION('center_axis',(-0.866025403784439,0.5,0.));
#19811=DIRECTION('ref_axis',(-0.5,-0.866025403784439,0.));
#19812=DIRECTION('',(-0.5,-0.866025403784439,0.));
#19813=DIRECTION('',(0.,0.,1.));
#19814=DIRECTION('',(-0.5,-0.866025403784439,0.));
#19815=DIRECTION('center_axis',(1.60246890531964E-16,1.,0.));
#19816=DIRECTION('ref_axis',(-1.,1.60246890531964E-16,0.));
#19817=DIRECTION('',(-1.,1.60246890531964E-16,0.));
#19818=DIRECTION('',(0.,0.,1.));
#19819=DIRECTION('',(-1.,1.60246890531964E-16,0.));
#19820=DIRECTION('center_axis',(0.866025403784439,0.5,0.));
#19821=DIRECTION('ref_axis',(-0.5,0.866025403784439,0.));
#19822=DIRECTION('',(-0.5,0.866025403784439,0.));
#19823=DIRECTION('',(0.,0.,1.));
#19824=DIRECTION('',(-0.5,0.866025403784439,0.));
#19825=DIRECTION('center_axis',(0.866025403784439,-0.5,0.));
#19826=DIRECTION('ref_axis',(0.5,0.866025403784439,0.));
#19827=DIRECTION('',(0.5,0.866025403784439,0.));
#19828=DIRECTION('',(0.5,0.866025403784439,0.));
#19829=DIRECTION('center_axis',(0.,0.,1.));
#19830=DIRECTION('ref_axis',(1.,0.,0.));
#19831=DIRECTION('center_axis',(0.,0.,1.));
#19832=DIRECTION('ref_axis',(1.,0.,0.));
#19833=DIRECTION('center_axis',(0.,0.,1.));
#19834=DIRECTION('ref_axis',(1.,0.,0.));
#19835=DIRECTION('center_axis',(0.,0.,1.));
#19836=DIRECTION('ref_axis',(1.,0.,0.));
#19837=DIRECTION('',(0.,0.,-1.));
#19838=DIRECTION('center_axis',(0.,0.,1.));
#19839=DIRECTION('ref_axis',(1.,0.,0.));
#19840=DIRECTION('center_axis',(0.,0.,1.));
#19841=DIRECTION('ref_axis',(1.,0.,0.));
#19842=DIRECTION('center_axis',(0.,0.,1.));
#19843=DIRECTION('ref_axis',(1.,0.,0.));
#19844=DIRECTION('',(0.,0.,1.));
#19845=DIRECTION('',(1.,0.,0.));
#19846=DIRECTION('',(0.,0.,1.));
#19847=DIRECTION('',(1.,0.,0.));
#19848=DIRECTION('',(0.,0.,1.));
#19849=DIRECTION('',(1.,0.,0.));
#19850=DIRECTION('',(0.,0.,1.));
#19851=DIRECTION('',(1.,0.,0.));
#19852=DIRECTION('',(0.,0.,1.));
#19853=DIRECTION('',(1.,0.,0.));
#19854=DIRECTION('',(0.,0.,1.));
#19855=DIRECTION('',(1.,0.,0.));
#19856=DIRECTION('',(0.,0.,1.));
#19857=DIRECTION('',(1.,0.,0.));
#19858=DIRECTION('',(0.,0.,1.));
#19859=DIRECTION('',(1.,0.,0.));
#19860=DIRECTION('',(0.,0.,1.));
#19861=DIRECTION('',(1.,0.,0.));
#19862=DIRECTION('',(0.,0.,1.));
#19863=DIRECTION('',(1.,0.,0.));
#19864=DIRECTION('',(0.,0.,1.));
#19865=DIRECTION('',(1.,0.,0.));
#19866=DIRECTION('',(0.,0.,1.));
#19867=DIRECTION('',(1.,0.,0.));
#19868=DIRECTION('',(0.,0.,1.));
#19869=DIRECTION('',(0.866025403784438,-0.5,0.));
#19870=DIRECTION('',(0.,0.,1.));
#19871=DIRECTION('',(1.,0.,0.));
#19872=DIRECTION('',(0.,0.,1.));
#19873=DIRECTION('',(1.,0.,0.));
#19874=DIRECTION('',(0.,0.,1.));
#19875=DIRECTION('',(1.,0.,0.));
#19876=DIRECTION('',(-1.,0.,-1.22464679914735E-16));
#19877=DIRECTION('',(0.,1.,0.));
#19878=DIRECTION('',(0.,-1.22464679914735E-16,-1.));
#19879=DIRECTION('',(2.22044604925031E-16,-1.,1.22464679914735E-16));
#19880=DIRECTION('',(0.,-1.22464679914735E-16,-1.));
#19881=DIRECTION('',(1.,0.,0.));
#19882=DIRECTION('',(0.,0.,1.));
#19883=DIRECTION('',(1.,0.,0.));
#19884=DIRECTION('',(0.,0.,1.));
#19885=DIRECTION('',(1.,0.,0.));
#19886=DIRECTION('',(0.,0.,1.));
#19887=DIRECTION('',(1.,0.,0.));
#19888=DIRECTION('',(0.,0.,1.));
#19889=DIRECTION('',(1.,0.,0.));
#19890=DIRECTION('',(0.,0.,1.));
#19891=DIRECTION('',(1.,0.,0.));
#19892=DIRECTION('',(0.,0.,1.));
#19893=DIRECTION('',(1.,0.,0.));
#19894=DIRECTION('',(0.,0.,1.));
#19895=DIRECTION('',(1.,0.,0.));
#19896=DIRECTION('',(0.,0.,1.));
#19897=DIRECTION('',(1.,0.,0.));
#19898=DIRECTION('',(0.,0.,1.));
#19899=DIRECTION('',(1.,0.,0.));
#19900=DIRECTION('',(0.,0.,1.));
#19901=DIRECTION('',(1.,0.,0.));
#19902=DIRECTION('',(0.,0.,1.));
#19903=DIRECTION('',(1.,0.,0.));
#19904=DIRECTION('',(0.,0.,1.));
#19905=DIRECTION('',(1.,0.,0.));
#19906=DIRECTION('',(0.,0.,1.));
#19907=DIRECTION('',(1.,0.,0.));
#19908=DIRECTION('',(0.,0.,1.));
#19909=DIRECTION('',(1.,0.,0.));
#19910=DIRECTION('',(0.,0.,1.));
#19911=DIRECTION('',(1.,0.,0.));
#19912=DIRECTION('',(0.,0.,1.));
#19913=DIRECTION('',(1.,0.,0.));
#19914=DIRECTION('',(0.,0.,1.));
#19915=DIRECTION('',(1.,0.,0.));
#19916=DIRECTION('',(0.,0.,1.));
#19917=DIRECTION('',(1.,0.,0.));
#19918=DIRECTION('',(0.,0.,1.));
#19919=DIRECTION('',(1.,0.,0.));
#19920=DIRECTION('',(0.,0.,1.));
#19921=DIRECTION('',(1.,0.,0.));
#19922=DIRECTION('',(0.,0.,1.));
#19923=DIRECTION('',(1.,0.,0.));
#19924=DIRECTION('',(0.,0.,1.));
#19925=DIRECTION('',(1.,0.,0.));
#19926=DIRECTION('',(0.,0.,1.));
#19927=DIRECTION('',(1.,0.,0.));
#19928=DIRECTION('',(0.,0.,1.));
#19929=DIRECTION('',(1.,0.,0.));
#19930=DIRECTION('',(0.,0.,1.));
#19931=DIRECTION('',(1.,0.,0.));
#19932=DIRECTION('',(0.,0.,1.));
#19933=DIRECTION('',(1.,0.,0.));
#19934=DIRECTION('',(0.,0.,1.));
#19935=DIRECTION('',(1.,0.,0.));
#19936=DIRECTION('',(0.,-1.22464679914735E-16,-1.));
#19937=DIRECTION('',(2.22044604925031E-16,-1.,1.22464679914735E-16));
#19938=DIRECTION('',(0.,-1.22464679914735E-16,-1.));
#19939=DIRECTION('',(2.22044604925031E-16,-1.,1.22464679914735E-16));
#19940=DIRECTION('',(0.,-1.22464679914735E-16,-1.));
#19941=DIRECTION('',(2.22044604925031E-16,-1.,1.22464679914735E-16));
#19942=DIRECTION('',(0.,0.,1.));
#19943=DIRECTION('',(-2.22044604925031E-16,-1.,0.));
#19944=DIRECTION('',(0.,0.,1.));
#19945=DIRECTION('',(-2.22044604925031E-16,-1.,0.));
#19946=DIRECTION('',(0.,0.,1.));
#19947=DIRECTION('',(-2.22044604925031E-16,-1.,0.));
#19948=DIRECTION('',(0.,0.,1.));
#19949=DIRECTION('',(-2.22044604925031E-16,-1.,0.));
#19950=CARTESIAN_POINT('',(0.,0.,0.));
#19951=CARTESIAN_POINT('',(0.,0.,0.));
#19952=CARTESIAN_POINT('Origin',(-46.,-3.,140.));
#19953=CARTESIAN_POINT('',(-49.9099188538711,-3.,80.));
#19954=CARTESIAN_POINT('',(-49.9099188538711,-3.,140.));
#19955=CARTESIAN_POINT('',(-49.9099188538711,-3.,60.));
#19956=CARTESIAN_POINT('',(-54.,-3.,80.));
#19957=CARTESIAN_POINT('',(-54.,-3.,80.));
#19958=CARTESIAN_POINT('',(-54.,-3.,140.));
#19959=CARTESIAN_POINT('',(-54.,-3.,140.));
#19960=CARTESIAN_POINT('',(-54.,-3.,140.));
#19961=CARTESIAN_POINT('Origin',(-50.,0.,140.));
#19962=CARTESIAN_POINT('',(-50.,-6.12323399573677E-15,140.));
#19963=CARTESIAN_POINT('Origin',(0.,0.,140.));
#19964=CARTESIAN_POINT('',(-54.,3.,140.));
#19965=CARTESIAN_POINT('',(-54.,3.,140.));
#19966=CARTESIAN_POINT('',(-49.9099188538711,3.,140.));
#19967=CARTESIAN_POINT('',(-46.,3.,140.));
#19968=CARTESIAN_POINT('Origin',(0.,0.,140.));
#19969=CARTESIAN_POINT('Origin',(-54.,3.,140.));
#19970=CARTESIAN_POINT('',(-49.9099188538711,3.,80.));
#19971=CARTESIAN_POINT('',(-49.9099188538711,3.,60.));
#19972=CARTESIAN_POINT('',(-54.,3.,80.));
#19973=CARTESIAN_POINT('',(-54.,3.,140.));
#19974=CARTESIAN_POINT('',(-46.,3.,80.));
#19975=CARTESIAN_POINT('Origin',(-54.,-3.,140.));
#19976=CARTESIAN_POINT('',(-54.,3.,80.));
#19977=CARTESIAN_POINT('Origin',(-50.,0.,80.));
#19978=CARTESIAN_POINT('',(-50.,-6.12323399573677E-15,80.));
#19979=CARTESIAN_POINT('Origin',(0.,0.,80.));
#19980=CARTESIAN_POINT('Origin',(0.,0.,80.));
#19981=CARTESIAN_POINT('Origin',(80.,0.,146.));
#19982=CARTESIAN_POINT('',(69.725,6.19873979128017,146.));
#19983=CARTESIAN_POINT('',(69.725,-6.19873979128017,146.));
#19984=CARTESIAN_POINT('Origin',(0.,0.,146.));
#19985=CARTESIAN_POINT('Origin',(80.,0.,146.));
#19986=CARTESIAN_POINT('Origin',(80.,0.,148.));
#19987=CARTESIAN_POINT('',(69.725,6.19873979128013,150.));
#19988=CARTESIAN_POINT('',(69.725,6.19873979128017,148.));
#19989=CARTESIAN_POINT('',(69.725,-6.19873979128013,150.));
#19990=CARTESIAN_POINT('Origin',(80.,0.,150.));
#19991=CARTESIAN_POINT('',(69.725,-6.19873979128017,148.));
#19992=CARTESIAN_POINT('Origin',(0.,0.,60.));
#19993=CARTESIAN_POINT('',(68.3739716558867,-15.,150.));
#19994=CARTESIAN_POINT('Origin',(0.,0.,150.));
#19995=CARTESIAN_POINT('',(68.3739716558867,-15.,160.));
#19996=CARTESIAN_POINT('',(68.3739716558867,-15.,60.));
#19997=CARTESIAN_POINT('',(-70.,-8.57252759403147E-15,160.));
#19998=CARTESIAN_POINT('Origin',(0.,0.,160.));
#19999=CARTESIAN_POINT('',(-70.,-8.57252759403147E-15,110.));
#20000=CARTESIAN_POINT('',(-70.,-8.57252759403147E-15,60.));
#20001=CARTESIAN_POINT('Origin',(0.,0.,110.));
#20002=CARTESIAN_POINT('',(68.3739716558867,15.,160.));
#20003=CARTESIAN_POINT('Origin',(0.,0.,160.));
#20004=CARTESIAN_POINT('',(68.3739716558867,15.,150.));
#20005=CARTESIAN_POINT('',(68.3739716558867,15.,60.));
#20006=CARTESIAN_POINT('Origin',(0.,0.,150.));
#20007=CARTESIAN_POINT('Origin',(80.,0.,155.));
#20008=CARTESIAN_POINT('',(72.,9.79717439317883E-16,160.));
#20009=CARTESIAN_POINT('Origin',(80.,0.,160.));
#20010=CARTESIAN_POINT('',(72.,9.79717439317883E-16,150.));
#20011=CARTESIAN_POINT('',(72.,9.79717439317883E-16,155.));
#20012=CARTESIAN_POINT('Origin',(80.,0.,150.));
#20013=CARTESIAN_POINT('Origin',(80.,0.,100.));
#20014=CARTESIAN_POINT('',(72.,9.79717439317883E-16,110.));
#20015=CARTESIAN_POINT('Origin',(80.,0.,110.));
#20016=CARTESIAN_POINT('',(72.,9.79717439317883E-16,90.));
#20017=CARTESIAN_POINT('',(72.,9.79717439317883E-16,100.));
#20018=CARTESIAN_POINT('Origin',(80.,0.,90.));
#20019=CARTESIAN_POINT('Origin',(60.,-60.,100.));
#20020=CARTESIAN_POINT('',(54.5,-60.,110.));
#20021=CARTESIAN_POINT('Origin',(60.,-60.,110.));
#20022=CARTESIAN_POINT('',(54.5,-60.,90.));
#20023=CARTESIAN_POINT('',(54.5,-60.,100.));
#20024=CARTESIAN_POINT('Origin',(60.,-60.,90.));
#20025=CARTESIAN_POINT('Origin',(-60.,-60.,100.));
#20026=CARTESIAN_POINT('',(-65.5,-60.,110.));
#20027=CARTESIAN_POINT('Origin',(-60.,-60.,110.));
#20028=CARTESIAN_POINT('',(-65.5,-60.,90.));
#20029=CARTESIAN_POINT('',(-65.5,-60.,100.));
#20030=CARTESIAN_POINT('Origin',(-60.,-60.,90.));
#20031=CARTESIAN_POINT('Origin',(-60.,60.,100.));
#20032=CARTESIAN_POINT('',(-65.5,60.,110.));
#20033=CARTESIAN_POINT('Origin',(-60.,60.,110.));
#20034=CARTESIAN_POINT('',(-65.5,60.,90.));
#20035=CARTESIAN_POINT('',(-65.5,60.,100.));
#20036=CARTESIAN_POINT('Origin',(-60.,60.,90.));
#20037=CARTESIAN_POINT('Origin',(60.,60.,100.));
#20038=CARTESIAN_POINT('',(54.5,60.,110.));
#20039=CARTESIAN_POINT('Origin',(60.,60.,110.));
#20040=CARTESIAN_POINT('',(54.5,60.,90.));
#20041=CARTESIAN_POINT('',(54.5,60.,100.));
#20042=CARTESIAN_POINT('Origin',(60.,60.,90.));
#20043=CARTESIAN_POINT('Origin',(100.,15.,150.));
#20044=CARTESIAN_POINT('',(100.,15.,160.));
#20045=CARTESIAN_POINT('',(100.,15.,160.));
#20046=CARTESIAN_POINT('',(100.,15.,150.));
#20047=CARTESIAN_POINT('',(100.,15.,150.));
#20048=CARTESIAN_POINT('',(100.,15.,150.));
#20049=CARTESIAN_POINT('Origin',(100.,-15.,150.));
#20050=CARTESIAN_POINT('',(100.,-15.,150.));
#20051=CARTESIAN_POINT('',(100.,-15.,150.));
#20052=CARTESIAN_POINT('',(100.,-15.,160.));
#20053=CARTESIAN_POINT('',(100.,-15.,160.));
#20054=CARTESIAN_POINT('',(100.,-15.,150.));
#20055=CARTESIAN_POINT('Origin',(50.,-15.,150.));
#20056=CARTESIAN_POINT('',(50.,-15.,150.));
#20057=CARTESIAN_POINT('',(50.,-15.,160.));
#20058=CARTESIAN_POINT('Origin',(75.,0.,150.));
#20059=CARTESIAN_POINT('Origin',(0.,0.,110.));
#20060=CARTESIAN_POINT('',(-100.,-1.22464679914735E-14,110.));
#20061=CARTESIAN_POINT('Origin',(0.,0.,110.));
#20062=CARTESIAN_POINT('Origin',(0.,0.,90.));
#20063=CARTESIAN_POINT('',(-100.,-1.22464679914735E-14,90.));
#20064=CARTESIAN_POINT('Origin',(0.,0.,90.));
#20065=CARTESIAN_POINT('',(-70.,8.57252759403147E-15,90.));
#20066=CARTESIAN_POINT('Origin',(0.,0.,90.));
#20067=CARTESIAN_POINT('Origin',(0.,0.,90.));
#20068=CARTESIAN_POINT('',(-100.,-1.22464679914735E-14,90.));
#20069=CARTESIAN_POINT('Origin',(0.,0.,60.));
#20070=CARTESIAN_POINT('',(-70.,-8.57252759403147E-15,60.));
#20071=CARTESIAN_POINT('',(-70.,-8.57252759403147E-15,60.));
#20072=CARTESIAN_POINT('Origin',(0.,0.,60.));
#20073=CARTESIAN_POINT('Origin',(0.,0.,60.));
#20074=CARTESIAN_POINT('',(-50.,-6.12323399573677E-15,160.));
#20075=CARTESIAN_POINT('Origin',(0.,0.,160.));
#20076=CARTESIAN_POINT('',(-50.,-6.12323399573677E-15,60.));
#20077=CARTESIAN_POINT('',(-50.,-6.12323399573677E-15,60.));
#20078=CARTESIAN_POINT('',(-50.,-6.12323399573677E-15,60.));
#20079=CARTESIAN_POINT('Origin',(0.,0.,60.));
#20080=CARTESIAN_POINT('Origin',(0.,0.,160.));
#20081=CARTESIAN_POINT('Origin',(0.,0.,60.));
#20082=CARTESIAN_POINT('',(0.,0.,0.));
#20083=CARTESIAN_POINT('Origin',(80.,0.,48.));
#20084=CARTESIAN_POINT('',(74.8632856275073,0.000121616040080763,42.4259584946969));
#20085=CARTESIAN_POINT('',(74.86325,6.29070444552017E-16,42.));
#20086=CARTESIAN_POINT('',(74.86325,6.29070444552017E-16,48.));
#20087=CARTESIAN_POINT('',(79.7872015765661,5.13234034271734,42.));
#20088=CARTESIAN_POINT('Origin',(80.,0.,42.));
#20089=CARTESIAN_POINT('Ctrl Pts',(79.7872818445161,5.13260507264869,42.));
#20090=CARTESIAN_POINT('Ctrl Pts',(79.0562851507116,5.10168006756045,42.0396772434995));
#20091=CARTESIAN_POINT('Ctrl Pts',(78.3315536646317,4.91345033611241,42.079354486999));
#20092=CARTESIAN_POINT('Ctrl Pts',(77.6789039388635,4.58290131773057,42.1190317304985));
#20093=CARTESIAN_POINT('Ctrl Pts',(76.9301312492104,4.20366867917444,42.1645526817226));
#20094=CARTESIAN_POINT('Ctrl Pts',(76.2762364578729,3.6371077237785,42.2100736329468));
#20095=CARTESIAN_POINT('Ctrl Pts',(75.7942602890204,2.94995818481276,42.2555945841709));
#20096=CARTESIAN_POINT('Ctrl Pts',(75.3122841201679,2.26280864584703,42.3011155353951));
#20097=CARTESIAN_POINT('Ctrl Pts',(75.0022265738003,1.45507052331149,42.3466364866192));
#20098=CARTESIAN_POINT('Ctrl Pts',(74.9006161199858,0.621912016979159,42.3921574378433));
#20099=CARTESIAN_POINT('Ctrl Pts',(74.8754662301444,0.415694606583752,42.4034244567945));
#20100=CARTESIAN_POINT('Ctrl Pts',(74.8630863502092,0.207919877499314,42.4146914757457));
#20101=CARTESIAN_POINT('Ctrl Pts',(74.8632856275073,0.000121616040080763,
42.4259584946969));
#20102=CARTESIAN_POINT('Origin',(80.,0.,48.));
#20103=CARTESIAN_POINT('',(74.8628762025111,4.99008593407568E-5,44.1759584946969));
#20104=CARTESIAN_POINT('',(74.8636304222849,4.19133500426576E-5,43.6990415053031));
#20105=CARTESIAN_POINT('',(74.86325,6.29070444552017E-16,48.));
#20106=CARTESIAN_POINT('',(74.9489860411411,-0.934590043769125,42.));
#20107=CARTESIAN_POINT('Ctrl Pts',(74.8636304222849,4.19133500426576E-5,
43.6990415053031));
#20108=CARTESIAN_POINT('Ctrl Pts',(74.8635208617496,0.370740519310411,43.6789457515585));
#20109=CARTESIAN_POINT('Ctrl Pts',(74.9031296129329,0.741416057941528,43.6588499978138));
#20110=CARTESIAN_POINT('Ctrl Pts',(74.9827083545788,1.10330220113088,43.6387542440692));
#20111=CARTESIAN_POINT('Ctrl Pts',(75.1629703175275,1.92304759023842,43.593233292845));
#20112=CARTESIAN_POINT('Ctrl Pts',(75.5483239883248,2.69769334081098,43.5477123416209));
#20113=CARTESIAN_POINT('Ctrl Pts',(76.0933689928018,3.3359744761171,43.5021913903967));
#20114=CARTESIAN_POINT('Ctrl Pts',(76.6384139972788,3.97425561142324,43.4566704391726));
#20115=CARTESIAN_POINT('Ctrl Pts',(77.3431503354356,4.47617213146291,43.4111494879485));
#20116=CARTESIAN_POINT('Ctrl Pts',(78.1245493196722,4.78259088641757,43.3656285367243));
#20117=CARTESIAN_POINT('Ctrl Pts',(78.9059483039088,5.08900964137223,43.3201075855002));
#20118=CARTESIAN_POINT('Ctrl Pts',(79.7640099342254,5.19993063124186,43.274586634276));
#20119=CARTESIAN_POINT('Ctrl Pts',(80.5976420089561,5.10228536737467,43.2290656830519));
#20120=CARTESIAN_POINT('Ctrl Pts',(81.4312740836868,5.00464010350749,43.1835447318277));
#20121=CARTESIAN_POINT('Ctrl Pts',(82.2404766028315,4.69842858590349,43.1380237806036));
#20122=CARTESIAN_POINT('Ctrl Pts',(82.9299126180493,4.2197278344979,43.0925028293795));
#20123=CARTESIAN_POINT('Ctrl Pts',(83.619348633267,3.74102708309231,43.0469818781553));
#20124=CARTESIAN_POINT('Ctrl Pts',(84.1890181445578,3.08983709788513,43.0014609269312));
#20125=CARTESIAN_POINT('Ctrl Pts',(84.5718071021192,2.34287633816629,42.955939975707));
#20126=CARTESIAN_POINT('Ctrl Pts',(84.9545960596807,1.59591557844745,42.9104190244829));
#20127=CARTESIAN_POINT('Ctrl Pts',(85.1505044635128,0.753184044216937,42.8648980732587));
#20128=CARTESIAN_POINT('Ctrl Pts',(85.1364480089129,-0.0860286291164032,
42.8193771220346));
#20129=CARTESIAN_POINT('Ctrl Pts',(85.1223915543129,-0.925241302449768,
42.7738561708104));
#20130=CARTESIAN_POINT('Ctrl Pts',(84.8983702412809,-1.76093511488598,42.7283352195863));
#20131=CARTESIAN_POINT('Ctrl Pts',(84.4907843336716,-2.4946596112628,42.6828142683622));
#20132=CARTESIAN_POINT('Ctrl Pts',(84.0831984260624,-3.22838410763962,42.637293317138));
#20133=CARTESIAN_POINT('Ctrl Pts',(83.4920479238758,-3.86013928795704,42.5917723659139));
#20134=CARTESIAN_POINT('Ctrl Pts',(82.786964128127,-4.31548031249223,42.5462514146897));
#20135=CARTESIAN_POINT('Ctrl Pts',(82.0818803323782,-4.77082133702742,42.5007304634656));
#20136=CARTESIAN_POINT('Ctrl Pts',(81.2628632430673,-5.04974820578038,42.4552095122414));
#20137=CARTESIAN_POINT('Ctrl Pts',(80.4264389659417,-5.11943010927012,42.4096885610173));
#20138=CARTESIAN_POINT('Ctrl Pts',(79.5900146888162,-5.18911201275987,42.3641676097932));
#20139=CARTESIAN_POINT('Ctrl Pts',(78.7361832238761,-5.04954895098638,42.318646658569));
#20140=CARTESIAN_POINT('Ctrl Pts',(77.96547438976,-4.7171163339107,42.2731257073449));
#20141=CARTESIAN_POINT('Ctrl Pts',(77.1947655556439,-4.38468371683501,42.2276047561207));
#20142=CARTESIAN_POINT('Ctrl Pts',(76.5071793523518,-3.85938154445711,42.1820838048966));
#20143=CARTESIAN_POINT('Ctrl Pts',(75.9839213652191,-3.20324008292404,42.1365628536724));
#20144=CARTESIAN_POINT('Ctrl Pts',(75.4606633780864,-2.54709862139098,42.0910419024483));
#20145=CARTESIAN_POINT('Ctrl Pts',(75.1017336071131,-1.76011787070275,42.0455209512241));
#20146=CARTESIAN_POINT('Ctrl Pts',(74.9489860411411,-0.934590043769161,
42.));
#20147=CARTESIAN_POINT('Origin',(80.,0.,42.));
#20148=CARTESIAN_POINT('Ctrl Pts',(74.8632856275073,0.000121616040080763,
42.4259584946969));
#20149=CARTESIAN_POINT('Ctrl Pts',(74.86389146931,-0.631625575059074,42.4602124269698));
#20150=CARTESIAN_POINT('Ctrl Pts',(74.9807637485846,-1.26359027082345,42.4944663592428));
#20151=CARTESIAN_POINT('Ctrl Pts',(75.2085395310293,-1.85267328325476,42.5287202915158));
#20152=CARTESIAN_POINT('Ctrl Pts',(75.5112367571486,-2.63552118702721,42.5742412427399));
#20153=CARTESIAN_POINT('Ctrl Pts',(76.0097945706485,-3.34263810444295,42.6197621939641));
#20154=CARTESIAN_POINT('Ctrl Pts',(76.6454751600456,-3.89071404950825,42.6652831451882));
#20155=CARTESIAN_POINT('Ctrl Pts',(77.2811557494428,-4.43878999457355,42.7108040964123));
#20156=CARTESIAN_POINT('Ctrl Pts',(78.0539591147372,-4.82782496728842,42.7563250476365));
#20157=CARTESIAN_POINT('Ctrl Pts',(78.8728375123135,-5.01198527001719,42.8018459988606));
#20158=CARTESIAN_POINT('Ctrl Pts',(79.6917159098899,-5.19614557274597,42.8473669500848));
#20159=CARTESIAN_POINT('Ctrl Pts',(80.5566693397482,-5.1754312054887,42.8928879013089));
#20160=CARTESIAN_POINT('Ctrl Pts',(81.3657932499147,-4.95228241379094,42.9384088525331));
#20161=CARTESIAN_POINT('Ctrl Pts',(82.1749171600812,-4.72913362209319,42.9839298037572));
#20162=CARTESIAN_POINT('Ctrl Pts',(82.9282115505558,-4.30355040595498,43.0294507549814));
#20163=CARTESIAN_POINT('Ctrl Pts',(83.5369270500077,-3.72567296245263,43.0749717062055));
#20164=CARTESIAN_POINT('Ctrl Pts',(84.1456425494596,-3.14779551895029,43.1204926574296));
#20165=CARTESIAN_POINT('Ctrl Pts',(84.6097791578887,-2.41762384808381,43.1660136086538));
#20166=CARTESIAN_POINT('Ctrl Pts',(84.8746546014611,-1.62118309157148,43.2115345598779));
#20167=CARTESIAN_POINT('Ctrl Pts',(85.1395300450336,-0.824742335059147,
43.2570555111021));
#20168=CARTESIAN_POINT('Ctrl Pts',(85.2051443237493,0.0379675070990354,
43.3025764623262));
#20169=CARTESIAN_POINT('Ctrl Pts',(85.0637670949036,0.865306235619404,43.3480974135504));
#20170=CARTESIAN_POINT('Ctrl Pts',(84.9223898660578,1.69264496413977,43.3936183647745));
#20171=CARTESIAN_POINT('Ctrl Pts',(84.5740211296506,2.48461257902233,43.4391393159986));
#20172=CARTESIAN_POINT('Ctrl Pts',(84.0597039528812,3.14790341083024,43.4846602672228));
#20173=CARTESIAN_POINT('Ctrl Pts',(83.5453867761118,3.81119424263815,43.5301812184469));
#20174=CARTESIAN_POINT('Ctrl Pts',(82.8651211589803,4.34580829137141,43.5757021696711));
#20175=CARTESIAN_POINT('Ctrl Pts',(82.0990526094627,4.68875998754711,43.6212231208952));
#20176=CARTESIAN_POINT('Ctrl Pts',(81.332984059945,5.03171168372281,43.6667440721194));
#20177=CARTESIAN_POINT('Ctrl Pts',(80.4811125780413,5.18300102734094,43.7122650233435));
#20178=CARTESIAN_POINT('Ctrl Pts',(79.64380141847,5.12480386375012,43.7577859745677));
#20179=CARTESIAN_POINT('Ctrl Pts',(78.8064902588986,5.06660670015931,43.8033069257918));
#20180=CARTESIAN_POINT('Ctrl Pts',(77.9837394216597,4.79892302935956,43.8488278770159));
#20181=CARTESIAN_POINT('Ctrl Pts',(77.2724813128825,4.35329000715137,43.8943488282401));
#20182=CARTESIAN_POINT('Ctrl Pts',(76.5612232041052,3.90765698494317,43.9398697794642));
#20183=CARTESIAN_POINT('Ctrl Pts',(75.9614578237895,3.28407461132652,43.9853907306884));
#20184=CARTESIAN_POINT('Ctrl Pts',(75.5438465417775,2.556010256289,44.0309116819125));
#20185=CARTESIAN_POINT('Ctrl Pts',(75.1262352597655,1.82794590125149,44.0764326331367));
#20186=CARTESIAN_POINT('Ctrl Pts',(74.8907780760572,0.995399564793116,44.1219535843608));
#20187=CARTESIAN_POINT('Ctrl Pts',(74.8652153833832,0.156457709503931,44.1674745355849));
#20188=CARTESIAN_POINT('Ctrl Pts',(74.8636273026306,0.10433849694978,44.1703025219556));
#20189=CARTESIAN_POINT('Ctrl Pts',(74.862849311385,0.0521946008383264,44.1731305083262));
#20190=CARTESIAN_POINT('Ctrl Pts',(74.8628762025111,4.99008593407568E-5,
44.1759584946969));
#20191=CARTESIAN_POINT('Origin',(80.,0.,48.));
#20192=CARTESIAN_POINT('',(74.8629839453475,-8.98047708566482E-5,45.9259584946969));
#20193=CARTESIAN_POINT('',(74.8633066453123,0.000121786292464538,45.4490415053031));
#20194=CARTESIAN_POINT('',(74.86325,6.29070444552017E-16,48.));
#20195=CARTESIAN_POINT('Ctrl Pts',(74.8633066453123,0.000121786292464538,
45.4490415053031));
#20196=CARTESIAN_POINT('Ctrl Pts',(74.8631028564357,0.215109900456405,45.437384784139));
#20197=CARTESIAN_POINT('Ctrl Pts',(74.8763564073468,0.430073059765048,45.4257280629749));
#20198=CARTESIAN_POINT('Ctrl Pts',(74.9032715236375,0.643311848838259,45.4140713418108));
#20199=CARTESIAN_POINT('Ctrl Pts',(75.0083784124968,1.47603593821421,45.3685503905866));
#20200=CARTESIAN_POINT('Ctrl Pts',(75.3218241722691,2.28246338164187,45.3230294393625));
#20201=CARTESIAN_POINT('Ctrl Pts',(75.8066801846642,2.96758491418775,45.2775084881384));
#20202=CARTESIAN_POINT('Ctrl Pts',(76.2915361970593,3.65270644673361,45.2319875369142));
#20203=CARTESIAN_POINT('Ctrl Pts',(76.9478024620773,4.21652206839771,45.1864665856901));
#20204=CARTESIAN_POINT('Ctrl Pts',(77.6981609569454,4.59260583073588,45.1409456344659));
#20205=CARTESIAN_POINT('Ctrl Pts',(78.4485194518134,4.96868959307406,45.0954246832418));
#20206=CARTESIAN_POINT('Ctrl Pts',(79.2929701765315,5.1570414960863,45.0499037320176));
#20207=CARTESIAN_POINT('Ctrl Pts',(80.132024152519,5.13547085667211,45.0043827807935));
#20208=CARTESIAN_POINT('Ctrl Pts',(80.9710781285065,5.11390021725791,44.9588618295693));
#20209=CARTESIAN_POINT('Ctrl Pts',(81.8047353557635,4.88240703541727,44.9133408783452));
#20210=CARTESIAN_POINT('Ctrl Pts',(82.5347784918799,4.46826468483543,44.8678199271211));
#20211=CARTESIAN_POINT('Ctrl Pts',(83.2648216279964,4.0541223342536,44.8222989758969));
#20212=CARTESIAN_POINT('Ctrl Pts',(83.8912506729723,3.45733081493057,44.7767780246728));
#20213=CARTESIAN_POINT('Ctrl Pts',(84.3402628766027,2.74820113140603,44.7312570734486));
#20214=CARTESIAN_POINT('Ctrl Pts',(84.7892750802332,2.0390714478815,44.6857361222245));
#20215=CARTESIAN_POINT('Ctrl Pts',(85.0608704425183,1.21760360015545,44.6402151710004));
#20216=CARTESIAN_POINT('Ctrl Pts',(85.1230509507437,0.38057883852083,44.5946942197762));
#20217=CARTESIAN_POINT('Ctrl Pts',(85.1852314589692,-0.456445923113787,
44.5491732685521));
#20218=CARTESIAN_POINT('Ctrl Pts',(85.037997113135,-1.30902759865697,44.5036523173279));
#20219=CARTESIAN_POINT('Ctrl Pts',(84.6986943301815,-2.07671926105541,44.4581313661038));
#20220=CARTESIAN_POINT('Ctrl Pts',(84.359391547228,-2.84441092345386,44.4126104148796));
#20221=CARTESIAN_POINT('Ctrl Pts',(83.8280203271551,-3.52721257270756,44.3670894636555));
#20222=CARTESIAN_POINT('Ctrl Pts',(83.167184181402,-4.04467991999574,44.3215685124314));
#20223=CARTESIAN_POINT('Ctrl Pts',(82.506348035649,-4.56214726728393,44.2760475612072));
#20224=CARTESIAN_POINT('Ctrl Pts',(81.7160469642156,-4.91428031260659,44.2305266099831));
#20225=CARTESIAN_POINT('Ctrl Pts',(80.8893903014861,-5.05959249273419,44.1850056587589));
#20226=CARTESIAN_POINT('Ctrl Pts',(80.0627336387566,-5.2049046728618,44.1394847075348));
#20227=CARTESIAN_POINT('Ctrl Pts',(79.1997213847309,-5.14339598779434,44.0939637563106));
#20228=CARTESIAN_POINT('Ctrl Pts',(78.4020293485828,-4.88231308796566,44.0484428050865));
#20229=CARTESIAN_POINT('Ctrl Pts',(77.6043373124346,-4.62123018813698,44.0029218538623));
#20230=CARTESIAN_POINT('Ctrl Pts',(76.871965494164,-4.16057307354708,43.9574009026382));
#20231=CARTESIAN_POINT('Ctrl Pts',(76.2911982859515,-3.55461406363621,43.911879951414));
#20232=CARTESIAN_POINT('Ctrl Pts',(75.710431077739,-2.94865505372537,43.8663590001899));
#20233=CARTESIAN_POINT('Ctrl Pts',(75.2812684795846,-2.19739414849357,43.8208380489657));
#20234=CARTESIAN_POINT('Ctrl Pts',(75.0542723080574,-1.38934118205641,43.7753170977416));
#20235=CARTESIAN_POINT('Ctrl Pts',(74.9274862385012,-0.93801260273047,43.7498919002621));
#20236=CARTESIAN_POINT('Ctrl Pts',(74.8637690385459,-0.46896688232286,43.7244667027826));
#20237=CARTESIAN_POINT('Ctrl Pts',(74.8636304222849,4.19133500426576E-5,
43.6990415053031));
#20238=CARTESIAN_POINT('Ctrl Pts',(74.8628762025111,4.99008593407568E-5,
44.1759584946969));
#20239=CARTESIAN_POINT('Ctrl Pts',(74.8632821669507,-0.787157515205568,
44.2186514595504));
#20240=CARTESIAN_POINT('Ctrl Pts',(75.047126602999,-1.57454813845282,44.2613444244039));
#20241=CARTESIAN_POINT('Ctrl Pts',(75.3964937240302,-2.27996097356572,44.3040373892574));
#20242=CARTESIAN_POINT('Ctrl Pts',(75.7690029589908,-3.03210042722621,44.3495583404815));
#20243=CARTESIAN_POINT('Ctrl Pts',(76.3296896305517,-3.69104196042718,44.3950792917057));
#20244=CARTESIAN_POINT('Ctrl Pts',(77.0124964276053,-4.17915236366638,44.4406002429298));
#20245=CARTESIAN_POINT('Ctrl Pts',(77.695303224659,-4.66726276690558,44.4861211941539));
#20246=CARTESIAN_POINT('Ctrl Pts',(78.5002301472054,-4.98454204018302,44.5316421453781));
#20247=CARTESIAN_POINT('Ctrl Pts',(79.3324447141988,-5.09360991972006,44.5771630966022));
#20248=CARTESIAN_POINT('Ctrl Pts',(80.1646592811922,-5.20267779925709,44.6226840478264));
#20249=CARTESIAN_POINT('Ctrl Pts',(81.0241614926327,-5.10353428505372,44.6682049990505));
#20250=CARTESIAN_POINT('Ctrl Pts',(81.8096890787593,-4.80785997217622,44.7137259502747));
#20251=CARTESIAN_POINT('Ctrl Pts',(82.5952166648858,-4.51218565929872,44.7592469014988));
#20252=CARTESIAN_POINT('Ctrl Pts',(83.3067696256985,-4.01998054774709,44.804767852723));
#20253=CARTESIAN_POINT('Ctrl Pts',(83.8605163352739,-3.38923379230978,44.8502888039471));
#20254=CARTESIAN_POINT('Ctrl Pts',(84.4142630448494,-2.75848703687247,44.8958097551712));
#20255=CARTESIAN_POINT('Ctrl Pts',(84.8102035031877,-1.98919863754947,44.9413307063954));
#20256=CARTESIAN_POINT('Ctrl Pts',(85.0016899774868,-1.17200232207685,44.9868516576195));
#20257=CARTESIAN_POINT('Ctrl Pts',(85.1931764517859,-0.354806006604231,
45.0323726088437));
#20258=CARTESIAN_POINT('Ctrl Pts',(85.1802089420458,0.510298225017999,45.0778935600678));
#20259=CARTESIAN_POINT('Ctrl Pts',(84.9643152156786,1.32138810091097,45.123414511292));
#20260=CARTESIAN_POINT('Ctrl Pts',(84.7484214893113,2.13247797680394,45.1689354625161));
#20261=CARTESIAN_POINT('Ctrl Pts',(84.329601546317,2.88955349696764,45.2144564137403));
#20262=CARTESIAN_POINT('Ctrl Pts',(83.757198666428,3.50341979426373,45.2599773649644));
#20263=CARTESIAN_POINT('Ctrl Pts',(83.1847957865391,4.11728609155982,45.3054983161885));
#20264=CARTESIAN_POINT('Ctrl Pts',(82.4588099697556,4.5879431659883,45.3510192674127));
#20265=CARTESIAN_POINT('Ctrl Pts',(81.6647732492066,4.85994054516851,45.3965402186368));
#20266=CARTESIAN_POINT('Ctrl Pts',(80.8707365286577,5.13193792434872,45.442061169861));
#20267=CARTESIAN_POINT('Ctrl Pts',(80.0086489043433,5.20527560828067,45.4875821210851));
#20268=CARTESIAN_POINT('Ctrl Pts',(79.1800772464949,5.07131331630493,45.5331030723093));
#20269=CARTESIAN_POINT('Ctrl Pts',(78.3515055886465,4.93735102432919,45.5786240235334));
#20270=CARTESIAN_POINT('Ctrl Pts',(77.556449897264,4.59608875644576,45.6241449747576));
#20271=CARTESIAN_POINT('Ctrl Pts',(76.8885796740965,4.087732333385,45.6696659259817));
#20272=CARTESIAN_POINT('Ctrl Pts',(76.2207094509289,3.57937591032425,45.7151868772058));
#20273=CARTESIAN_POINT('Ctrl Pts',(75.6800246959761,2.90392533208616,45.76070782843));
#20274=CARTESIAN_POINT('Ctrl Pts',(75.3302261941625,2.14095882168743,45.8062287796541));
#20275=CARTESIAN_POINT('Ctrl Pts',(75.0235448835553,1.47203780531562,45.8461386846684));
#20276=CARTESIAN_POINT('Ctrl Pts',(74.8635917035264,0.73584610333616,45.8860485896826));
#20277=CARTESIAN_POINT('Ctrl Pts',(74.8629839453475,-8.98047708566482E-5,
45.9259584946969));
#20278=CARTESIAN_POINT('Origin',(80.,0.,48.));
#20279=CARTESIAN_POINT('',(74.8634284288361,-0.000111732590146046,47.6759584946969));
#20280=CARTESIAN_POINT('',(74.8628882136866,5.62082028603397E-5,47.1990415053031));
#20281=CARTESIAN_POINT('',(74.86325,6.29070444552017E-16,48.));
#20282=CARTESIAN_POINT('Ctrl Pts',(74.8628882136866,5.62082028603397E-5,
47.1990415053031));
#20283=CARTESIAN_POINT('Ctrl Pts',(74.8628543749168,0.0593869527591274,
47.1958238167195));
#20284=CARTESIAN_POINT('Ctrl Pts',(74.863861606955,0.118716546768157,47.192606128136));
#20285=CARTESIAN_POINT('Ctrl Pts',(74.8659174321507,0.178009783776934,47.1893884395524));
#20286=CARTESIAN_POINT('Ctrl Pts',(74.895001389788,1.016836935532,47.1438674883282));
#20287=CARTESIAN_POINT('Ctrl Pts',(75.133951140809,1.8483875848139,47.0983465371041));
#20288=CARTESIAN_POINT('Ctrl Pts',(75.554614815648,2.5746925756988,47.05282558588));
#20289=CARTESIAN_POINT('Ctrl Pts',(75.975278490487,3.30099756658369,47.0073046346558));
#20290=CARTESIAN_POINT('Ctrl Pts',(76.577656089144,3.92205689907159,46.9617836834317));
#20291=CARTESIAN_POINT('Ctrl Pts',(77.2907784831134,4.36470045582208,46.9162627322075));
#20292=CARTESIAN_POINT('Ctrl Pts',(78.0039008770828,4.80734401257257,46.8707417809834));
#20293=CARTESIAN_POINT('Ctrl Pts',(78.8277680663645,5.07157179358564,46.8252208297592));
#20294=CARTESIAN_POINT('Ctrl Pts',(79.6653161220242,5.12625379770042,46.7796998785351));
#20295=CARTESIAN_POINT('Ctrl Pts',(80.5028641776839,5.18093580181521,46.734178927311));
#20296=CARTESIAN_POINT('Ctrl Pts',(81.3540930997216,5.02607202903169,46.6886579760868));
#20297=CARTESIAN_POINT('Ctrl Pts',(82.1187153361258,4.67990775775341,46.6431370248627));
#20298=CARTESIAN_POINT('Ctrl Pts',(82.8833375725299,4.33374348647512,46.5976160736385));
#20299=CARTESIAN_POINT('Ctrl Pts',(83.5613531233007,3.79627871670206,46.5520951224144));
#20300=CARTESIAN_POINT('Ctrl Pts',(84.0728815731323,3.13083487074198,46.5065741711902));
#20301=CARTESIAN_POINT('Ctrl Pts',(84.584410022964,2.4653910247819,46.4610532199661));
#20302=CARTESIAN_POINT('Ctrl Pts',(84.9294513718567,1.67196810263481,46.4155322687419));
#20303=CARTESIAN_POINT('Ctrl Pts',(85.0673545665774,0.844043241310327,46.3700113175178));
#20304=CARTESIAN_POINT('Ctrl Pts',(85.2052577612982,0.0161183799858468,
46.3244903662937));
#20305=CARTESIAN_POINT('Ctrl Pts',(85.136022801847,-0.846308420516015,46.2789694150695));
#20306=CARTESIAN_POINT('Ctrl Pts',(84.8678066063186,-1.64163032991474,46.2334484638454));
#20307=CARTESIAN_POINT('Ctrl Pts',(84.5995904107902,-2.43695223931347,46.1879275126212));
#20308=CARTESIAN_POINT('Ctrl Pts',(84.1323929791847,-3.16516925760907,46.1424065613971));
#20309=CARTESIAN_POINT('Ctrl Pts',(83.5212571859964,-3.74048648262277,46.0968856101729));
#20310=CARTESIAN_POINT('Ctrl Pts',(82.9101213928081,-4.31580370763648,46.0513646589488));
#20311=CARTESIAN_POINT('Ctrl Pts',(82.1550472380371,-4.73822113936829,46.0058437077247));
#20312=CARTESIAN_POINT('Ctrl Pts',(81.3449937979184,-4.95797165988025,45.9603227565005));
#20313=CARTESIAN_POINT('Ctrl Pts',(80.5349403577998,-5.17772218039221,45.9148018052764));
#20314=CARTESIAN_POINT('Ctrl Pts',(79.6699076323335,-5.1948057896843,45.8692808540522));
#20315=CARTESIAN_POINT('Ctrl Pts',(78.8518094689004,-5.00720978199521,45.8237599028281));
#20316=CARTESIAN_POINT('Ctrl Pts',(78.0337113054673,-4.81961377430612,45.7782389516039));
#20317=CARTESIAN_POINT('Ctrl Pts',(77.2625477040674,-4.42733814963586,45.7327180003798));
#20318=CARTESIAN_POINT('Ctrl Pts',(76.6291733194038,-3.87659886833748,45.6871970491556));
#20319=CARTESIAN_POINT('Ctrl Pts',(75.9957989347401,-3.32585958703911,45.6416760979315));
#20320=CARTESIAN_POINT('Ctrl Pts',(75.5002137668128,-2.61665664911263,45.5961551467074));
#20321=CARTESIAN_POINT('Ctrl Pts',(75.2008051918223,-1.83254481248728,45.5506341954832));
#20322=CARTESIAN_POINT('Ctrl Pts',(74.9780672965728,-1.24922344256412,45.5167699654232));
#20323=CARTESIAN_POINT('Ctrl Pts',(74.8638986774373,-0.624445521762548,
45.4829057353631));
#20324=CARTESIAN_POINT('Ctrl Pts',(74.8633066453123,0.000121786292464538,
45.4490415053031));
#20325=CARTESIAN_POINT('Ctrl Pts',(74.8629839453475,-8.98047708566482E-5,
45.9259584946969));
#20326=CARTESIAN_POINT('Ctrl Pts',(74.8628984989094,-0.103557111606977,
45.9315695409068));
#20327=CARTESIAN_POINT('Ctrl Pts',(74.8659627285546,-0.207019362333967,
45.9371805871167));
#20328=CARTESIAN_POINT('Ctrl Pts',(74.8722116978087,-0.310288900473523,
45.9427916333266));
#20329=CARTESIAN_POINT('Ctrl Pts',(74.9229079519428,-1.14808766967639,45.9883125845507));
#20330=CARTESIAN_POINT('Ctrl Pts',(75.1832127088856,-1.97320276552273,46.0338335357748));
#20331=CARTESIAN_POINT('Ctrl Pts',(75.6224581586331,-2.68842323694194,46.079354486999));
#20332=CARTESIAN_POINT('Ctrl Pts',(76.0617036083807,-3.40364370836115,46.1248754382231));
#20333=CARTESIAN_POINT('Ctrl Pts',(76.6798897509331,-4.00896955535324,46.1703963894473));
#20334=CARTESIAN_POINT('Ctrl Pts',(77.4041849738781,-4.43308430147757,46.2159173406714));
#20335=CARTESIAN_POINT('Ctrl Pts',(78.1284801968231,-4.8571990476019,46.2614382918956));
#20336=CARTESIAN_POINT('Ctrl Pts',(78.9588845001607,-5.10010269285848,46.3069592431197));
#20337=CARTESIAN_POINT('Ctrl Pts',(79.7975637847368,-5.13317753955548,46.3524801943439));
#20338=CARTESIAN_POINT('Ctrl Pts',(80.6362430693128,-5.16625238625248,46.398001145568));
#20339=CARTESIAN_POINT('Ctrl Pts',(81.4831973351274,-4.98949843438988,46.4435220967922));
#20340=CARTESIAN_POINT('Ctrl Pts',(82.2386426488751,-4.62373995424531,46.4890430480163));
#20341=CARTESIAN_POINT('Ctrl Pts',(82.9940879626228,-4.25798147410075,46.5345639992405));
#20342=CARTESIAN_POINT('Ctrl Pts',(83.6580243243037,-3.70321846567422,46.5800849504646));
#20343=CARTESIAN_POINT('Ctrl Pts',(84.1522300585487,-3.02481034359698,46.6256059016887));
#20344=CARTESIAN_POINT('Ctrl Pts',(84.6464357927938,-2.34640222151975,46.6711268529128));
#20345=CARTESIAN_POINT('Ctrl Pts',(84.970910899603,-1.54434898579181,46.716647804137));
#20346=CARTESIAN_POINT('Ctrl Pts',(85.0874273379546,-0.713144553985232,
46.7621687553611));
#20347=CARTESIAN_POINT('Ctrl Pts',(85.2039437763063,0.118059877821356,46.8076897065853));
#20348=CARTESIAN_POINT('Ctrl Pts',(85.1125015462003,0.97841550570658,46.8532106578094));
#20349=CARTESIAN_POINT('Ctrl Pts',(84.8238739157559,1.76655951463203,46.8987316090336));
#20350=CARTESIAN_POINT('Ctrl Pts',(84.5352462853114,2.55470352355748,46.9442525602577));
#20351=CARTESIAN_POINT('Ctrl Pts',(84.0494332545284,3.27063591352315,46.9897735114819));
#20352=CARTESIAN_POINT('Ctrl Pts',(83.4236708950806,3.83000909607603,47.035294462706));
#20353=CARTESIAN_POINT('Ctrl Pts',(82.7979085356327,4.3893822786289,47.0808154139302));
#20354=CARTESIAN_POINT('Ctrl Pts',(82.0321968475201,4.79219625376898,47.1263363651543));
#20355=CARTESIAN_POINT('Ctrl Pts',(81.2167481681753,4.99099348517798,47.1718573163784));
#20356=CARTESIAN_POINT('Ctrl Pts',(80.4012994888305,5.18979071658698,47.2173782676026));
#20357=CARTESIAN_POINT('Ctrl Pts',(79.5361138182536,5.18457120426489,47.2628992188267));
#20358=CARTESIAN_POINT('Ctrl Pts',(78.7231230230567,4.9759498851575,47.3084201700509));
#20359=CARTESIAN_POINT('Ctrl Pts',(77.9101322278597,4.76732856605011,47.353941121275));
#20360=CARTESIAN_POINT('Ctrl Pts',(77.1493363080427,4.35530544015742,47.3994620724991));
#20361=CARTESIAN_POINT('Ctrl Pts',(76.5303684497011,3.7884230200728,47.4449830237233));
#20362=CARTESIAN_POINT('Ctrl Pts',(75.9114005913594,3.22154059998819,47.4905039749474));
#20363=CARTESIAN_POINT('Ctrl Pts',(75.4342607944931,2.49979888571167,47.5360249261716));
#20364=CARTESIAN_POINT('Ctrl Pts',(75.1551632935531,1.70822989135296,47.5815458773957));
#20365=CARTESIAN_POINT('Ctrl Pts',(74.9622094643284,1.16097931389284,47.6130167498295));
#20366=CARTESIAN_POINT('Ctrl Pts',(74.8639126621751,0.580353831793524,47.6444876222632));
#20367=CARTESIAN_POINT('Ctrl Pts',(74.8634284288361,-0.000111732590146046,
47.6759584946969));
#20368=CARTESIAN_POINT('Origin',(80.,0.,48.));
#20369=CARTESIAN_POINT('',(74.8636526568313,-4.35339233453846E-6,49.4259584946969));
#20370=CARTESIAN_POINT('',(74.8629661957176,-8.50189945436741E-5,48.9490415053031));
#20371=CARTESIAN_POINT('',(74.86325,6.29070444552017E-16,48.));
#20372=CARTESIAN_POINT('Ctrl Pts',(74.8629661957176,-8.50189945436741E-5,
48.9490415053031));
#20373=CARTESIAN_POINT('Ctrl Pts',(74.8635556721698,0.743029487008711,48.9087418980759));
#20374=CARTESIAN_POINT('Ctrl Pts',(75.0267457376609,1.48639459196899,48.8684422908488));
#20375=CARTESIAN_POINT('Ctrl Pts',(75.3392541588398,2.1605414832218,48.8281426836216));
#20376=CARTESIAN_POINT('Ctrl Pts',(75.6922521550092,2.92203296827837,48.7826217323974));
#20377=CARTESIAN_POINT('Ctrl Pts',(76.2357673683812,3.59520804109921,48.7371007811733));
#20378=CARTESIAN_POINT('Ctrl Pts',(76.9057655435175,4.10075656738261,48.6915798299491));
#20379=CARTESIAN_POINT('Ctrl Pts',(77.5757637186539,4.60630509366602,48.646058878725));
#20380=CARTESIAN_POINT('Ctrl Pts',(78.3722448555547,4.94422707341198,48.6005379275009));
#20381=CARTESIAN_POINT('Ctrl Pts',(79.2013715135795,5.0747102220021,48.5550169762767));
#20382=CARTESIAN_POINT('Ctrl Pts',(80.0304981716043,5.20519337059221,48.5094960250526));
#20383=CARTESIAN_POINT('Ctrl Pts',(80.8922703507531,5.12823768802648,48.4639750738284));
#20384=CARTESIAN_POINT('Ctrl Pts',(81.6851583449729,4.85290970954365,48.4184541226043));
#20385=CARTESIAN_POINT('Ctrl Pts',(82.4780463391927,4.57758173106082,48.3729331713801));
#20386=CARTESIAN_POINT('Ctrl Pts',(83.2020501484835,4.1038814566609,48.327412220156));
#20387=CARTESIAN_POINT('Ctrl Pts',(83.7718712499674,3.48761789338864,48.2818912689318));
#20388=CARTESIAN_POINT('Ctrl Pts',(84.3416923514512,2.87135433011637,48.2363703177077));
#20389=CARTESIAN_POINT('Ctrl Pts',(84.7573307451282,2.11252747797175,48.1908493664835));
#20390=CARTESIAN_POINT('Ctrl Pts',(84.9698179855606,1.30053853730398,48.1453284152594));
#20391=CARTESIAN_POINT('Ctrl Pts',(85.182305225993,0.488549596636203,48.0998074640352));
#20392=CARTESIAN_POINT('Ctrl Pts',(85.1916413131808,-0.376601432554719,
48.0542865128111));
#20393=CARTESIAN_POINT('Ctrl Pts',(84.9967263158304,-1.19298676493227,48.008765561587));
#20394=CARTESIAN_POINT('Ctrl Pts',(84.8018113184798,-2.00937209730982,47.9632446103628));
#20395=CARTESIAN_POINT('Ctrl Pts',(84.4026452365911,-2.77699173287399,47.9177236591387));
#20396=CARTESIAN_POINT('Ctrl Pts',(83.8462558298679,-3.40540854932594,47.8722027079145));
#20397=CARTESIAN_POINT('Ctrl Pts',(83.2898664231448,-4.03382536577789,47.8266817566904));
#20398=CARTESIAN_POINT('Ctrl Pts',(82.5762536915873,-4.52303936311763,47.7811608054663));
#20399=CARTESIAN_POINT('Ctrl Pts',(81.7894919330479,-4.8154137847304,47.7356398542421));
#20400=CARTESIAN_POINT('Ctrl Pts',(81.0027301745085,-5.10778820634318,47.690118903018));
#20401=CARTESIAN_POINT('Ctrl Pts',(80.1428193889873,-5.20332305222899,47.6445979517938));
#20402=CARTESIAN_POINT('Ctrl Pts',(79.3110699824109,-5.09076288266106,47.5990770005697));
#20403=CARTESIAN_POINT('Ctrl Pts',(78.4793205758345,-4.97820271309314,47.5535560493455));
#20404=CARTESIAN_POINT('Ctrl Pts',(77.6757325482029,-4.65754752807148,47.5080350981214));
#20405=CARTESIAN_POINT('Ctrl Pts',(76.9949806386261,-4.1665753244581,47.4625141468972));
#20406=CARTESIAN_POINT('Ctrl Pts',(76.3142287290494,-3.67560312084472,47.4169931956731));
#20407=CARTESIAN_POINT('Ctrl Pts',(75.7563129375275,-3.01431389863962,47.371472244449));
#20408=CARTESIAN_POINT('Ctrl Pts',(75.3869641238935,-2.26061746042296,47.3259512932248));
#20409=CARTESIAN_POINT('Ctrl Pts',(75.043723056891,-1.56019671964928,47.2836480305843));
#20410=CARTESIAN_POINT('Ctrl Pts',(74.8633330952622,-0.779970821893516,
47.2413447679437));
#20411=CARTESIAN_POINT('Ctrl Pts',(74.8628882136866,5.62082028603397E-5,
47.1990415053031));
#20412=CARTESIAN_POINT('Ctrl Pts',(74.8634284288361,-0.000111732590146046,
47.6759584946969));
#20413=CARTESIAN_POINT('Ctrl Pts',(74.8632122442806,-0.259258883083046,
47.6900085734873));
#20414=CARTESIAN_POINT('Ctrl Pts',(74.8824915705452,-0.518374159578633,
47.7040586522777));
#20415=CARTESIAN_POINT('Ctrl Pts',(74.9215471990678,-0.774473513137255,
47.7181087310682));
#20416=CARTESIAN_POINT('Ctrl Pts',(75.0480838105362,-1.60421164882776,47.7636296822923));
#20417=CARTESIAN_POINT('Ctrl Pts',(75.3822122384867,-2.40229164576784,47.8091506335165));
#20418=CARTESIAN_POINT('Ctrl Pts',(75.8845671356794,-3.07468769359052,47.8546715847406));
#20419=CARTESIAN_POINT('Ctrl Pts',(76.3869220328721,-3.74708374141319,47.9001925359648));
#20420=CARTESIAN_POINT('Ctrl Pts',(77.0575033993071,-4.29379584011847,47.9457134871889));
#20421=CARTESIAN_POINT('Ctrl Pts',(77.8173066782509,-4.65041309316053,47.991234438413));
#20422=CARTESIAN_POINT('Ctrl Pts',(78.5771099571947,-5.00703034620259,48.0367553896372));
#20423=CARTESIAN_POINT('Ctrl Pts',(79.4261351486474,-5.17355275358143,48.0822763408613));
#20424=CARTESIAN_POINT('Ctrl Pts',(80.2643543331593,-5.13036147463186,48.1277972920855));
#20425=CARTESIAN_POINT('Ctrl Pts',(81.1025735176711,-5.0871701956823,48.1733182433096));
#20426=CARTESIAN_POINT('Ctrl Pts',(81.9299866952422,-4.8342652304043,48.2188391945338));
#20427=CARTESIAN_POINT('Ctrl Pts',(82.6491121662587,-4.40144258220266,48.2643601457579));
#20428=CARTESIAN_POINT('Ctrl Pts',(83.3682376372753,-3.96861993400101,48.309881096982));
#20429=CARTESIAN_POINT('Ctrl Pts',(83.9790754017373,-3.35587960287571,48.3554020482062));
#20430=CARTESIAN_POINT('Ctrl Pts',(84.4096595965402,-2.63541160285976,48.4009229994303));
#20431=CARTESIAN_POINT('Ctrl Pts',(84.8402437913431,-1.91494360284381,48.4464439506545));
#20432=CARTESIAN_POINT('Ctrl Pts',(85.090574416487,-1.08674793393721,48.4919649018786));
#20433=CARTESIAN_POINT('Ctrl Pts',(85.1311587644999,-0.248398484985625,
48.5374858531028));
#20434=CARTESIAN_POINT('Ctrl Pts',(85.1717431125128,0.589950963965957,48.5830068043269));
#20435=CARTESIAN_POINT('Ctrl Pts',(85.0025811833949,1.43845419296252,48.628527755551));
#20436=CARTESIAN_POINT('Ctrl Pts',(84.6436027931163,2.19714477757134,48.6740487067752));
#20437=CARTESIAN_POINT('Ctrl Pts',(84.2846244028378,2.95583536218017,48.7195696579993));
#20438=CARTESIAN_POINT('Ctrl Pts',(83.7358295513987,3.62471330240126,48.7650906092235));
#20439=CARTESIAN_POINT('Ctrl Pts',(83.0618745148986,4.12497473069372,48.8106115604476));
#20440=CARTESIAN_POINT('Ctrl Pts',(82.3879194783985,4.62523615898618,48.8561325116718));
#20441=CARTESIAN_POINT('Ctrl Pts',(81.5888042568375,4.95688107535002,48.9016534628959));
#20442=CARTESIAN_POINT('Ctrl Pts',(80.7586766255913,5.08083672751136,48.9471744141201));
#20443=CARTESIAN_POINT('Ctrl Pts',(79.9285489943452,5.20479237967269,48.9926953653442));
#20444=CARTESIAN_POINT('Ctrl Pts',(79.067408953414,5.12105876763151,49.0382163165683));
#20445=CARTESIAN_POINT('Ctrl Pts',(78.2767117334743,4.83950096851957,49.0837372677925));
#20446=CARTESIAN_POINT('Ctrl Pts',(77.4860145135347,4.55794316940763,49.1292582190166));
#20447=CARTESIAN_POINT('Ctrl Pts',(76.7657601145866,4.07856118322493,49.1747791702408));
#20448=CARTESIAN_POINT('Ctrl Pts',(76.2008053226555,3.45783340800046,49.2203001214649));
#20449=CARTESIAN_POINT('Ctrl Pts',(75.6358505307244,2.83710563277598,49.2658210726891));
#20450=CARTESIAN_POINT('Ctrl Pts',(75.2261953458102,2.07503206850973,49.3113420239132));
#20451=CARTESIAN_POINT('Ctrl Pts',(75.0201033014939,1.26139642700268,49.3568629751374));
#20452=CARTESIAN_POINT('Ctrl Pts',(74.9158287019511,0.849728276621614,49.3798948149905));
#20453=CARTESIAN_POINT('Ctrl Pts',(74.8636656234315,0.424860397329693,49.4029266548437));
#20454=CARTESIAN_POINT('Ctrl Pts',(74.8636526568313,-4.35339233453846E-6,
49.4259584946969));
#20455=CARTESIAN_POINT('Origin',(80.,0.,48.));
#20456=CARTESIAN_POINT('',(74.8634535980369,0.000107814451578703,51.1759584946969));
#20457=CARTESIAN_POINT('',(74.863409785596,-0.000114188402419197,50.6990415053031));
#20458=CARTESIAN_POINT('',(74.86325,6.29070444552017E-16,48.));
#20459=CARTESIAN_POINT('Ctrl Pts',(74.863409785596,-0.000114188402419197,
50.6990415053031));
#20460=CARTESIAN_POINT('Ctrl Pts',(74.8639137889733,0.587533088950244,50.6671809306565));
#20461=CARTESIAN_POINT('Ctrl Pts',(74.9647094137452,1.17534890055812,50.6353203560098));
#20462=CARTESIAN_POINT('Ctrl Pts',(75.1623764068138,1.72855120469804,50.6034597813632));
#20463=CARTESIAN_POINT('Ctrl Pts',(75.4447940860268,2.51894169147106,50.557938830139));
#20464=CARTESIAN_POINT('Ctrl Pts',(75.9249592108754,3.23867422423114,50.5124178789149));
#20465=CARTESIAN_POINT('Ctrl Pts',(76.5463011178337,3.80295350062791,50.4668969276907));
#20466=CARTESIAN_POINT('Ctrl Pts',(77.1676430247919,4.36723277702467,50.4213759764666));
#20467=CARTESIAN_POINT('Ctrl Pts',(77.9301617138597,4.77605879705811,50.3758550252424));
#20468=CARTESIAN_POINT('Ctrl Pts',(78.744021030849,4.98126571522392,50.3303340740183));
#20469=CARTESIAN_POINT('Ctrl Pts',(79.5578803478383,5.18647263338972,50.2848131227942));
#20470=CARTESIAN_POINT('Ctrl Pts',(80.4230802927489,5.18806044968789,50.23929217157));
#20471=CARTESIAN_POINT('Ctrl Pts',(81.2376873172381,4.98584209551033,50.1937712203459));
#20472=CARTESIAN_POINT('Ctrl Pts',(82.0522943417272,4.78362374133277,50.1482502691217));
#20473=CARTESIAN_POINT('Ctrl Pts',(82.8163084457949,4.37759921667948,50.1027293178976));
#20474=CARTESIAN_POINT('Ctrl Pts',(83.4397172929055,3.81560430882212,50.0572083666734));
#20475=CARTESIAN_POINT('Ctrl Pts',(84.0631261400161,3.25360940096478,50.0116874154493));
#20476=CARTESIAN_POINT('Ctrl Pts',(84.5459297301697,2.53564410990337,49.9661664642252));
#20477=CARTESIAN_POINT('Ctrl Pts',(84.8312465489989,1.74629553037307,49.920645513001));
#20478=CARTESIAN_POINT('Ctrl Pts',(85.1165633678282,0.956946950842764,49.8751245617768));
#20479=CARTESIAN_POINT('Ctrl Pts',(85.204393415333,0.0962150828435583,49.8296036105527));
#20480=CARTESIAN_POINT('Ctrl Pts',(85.0843889927579,-0.734492931849786,
49.7840826593286));
#20481=CARTESIAN_POINT('Ctrl Pts',(84.9643845701827,-1.56520094654313,49.7385617081044));
#20482=CARTESIAN_POINT('Ctrl Pts',(84.6365456775277,-2.36588510793061,49.6930407568803));
#20483=CARTESIAN_POINT('Ctrl Pts',(84.1394966603092,-3.04221279596022,49.6475198056562));
#20484=CARTESIAN_POINT('Ctrl Pts',(83.6424476430907,-3.71854048398984,49.601998854432));
#20485=CARTESIAN_POINT('Ctrl Pts',(82.9761885013088,-4.27051169866158,49.5564779032079));
#20486=CARTESIAN_POINT('Ctrl Pts',(82.2192145687153,-4.63309594057973,49.5109569519837));
#20487=CARTESIAN_POINT('Ctrl Pts',(81.4622406361219,-4.99568018249788,49.4654360007596));
#20488=CARTESIAN_POINT('Ctrl Pts',(80.6145519127169,-5.16887745166244,49.4199150495354));
#20489=CARTESIAN_POINT('Ctrl Pts',(79.7760188619409,-5.13228250843703,49.3743940983113));
#20490=CARTESIAN_POINT('Ctrl Pts',(78.9374858111649,-5.09568756521162,49.3288731470871));
#20491=CARTESIAN_POINT('Ctrl Pts',(78.108108433018,-4.84930040959626,49.283352195863));
#20492=CARTESIAN_POINT('Ctrl Pts',(77.3855998394428,-4.42214914912349,49.2378312446389));
#20493=CARTESIAN_POINT('Ctrl Pts',(76.6630912458677,-3.99499788865072,49.1923102934147));
#20494=CARTESIAN_POINT('Ctrl Pts',(76.0474514368645,-3.38708252332054,49.1467893421906));
#20495=CARTESIAN_POINT('Ctrl Pts',(75.6112120285087,-2.67002461372696,49.1012683909664));
#20496=CARTESIAN_POINT('Ctrl Pts',(75.1749726201528,-1.95296670413337,49.0557474397423));
#20497=CARTESIAN_POINT('Ctrl Pts',(74.9181336124445,-1.12676625027638,49.0102264885181));
#20498=CARTESIAN_POINT('Ctrl Pts',(74.8709544980738,-0.288762074701733,
48.964705537294));
#20499=CARTESIAN_POINT('Ctrl Pts',(74.8655429594531,-0.192641322522879,
48.959484193297));
#20500=CARTESIAN_POINT('Ctrl Pts',(74.8628898212925,-0.0963652741121222,
48.9542628493001));
#20501=CARTESIAN_POINT('Ctrl Pts',(74.8629661957176,-8.50189945436741E-5,
48.9490415053031));
#20502=CARTESIAN_POINT('Ctrl Pts',(74.8636526568313,-4.35339233453846E-6,
49.4259584946969));
#20503=CARTESIAN_POINT('Ctrl Pts',(74.8636399957796,-0.414857476611885,
49.4484476060679));
#20504=CARTESIAN_POINT('Ctrl Pts',(74.9133486457029,-0.829707616969254,
49.4709367174388));
#20505=CARTESIAN_POINT('Ctrl Pts',(75.0128145331795,-1.23226344317328,49.4934258288098));
#20506=CARTESIAN_POINT('Ctrl Pts',(75.2141467128998,-2.04708995309434,49.5389467800339));
#20507=CARTESIAN_POINT('Ctrl Pts',(75.6193399760587,-2.81154525418862,49.5844677312581));
#20508=CARTESIAN_POINT('Ctrl Pts',(76.1806564704738,-3.43556503028439,49.6299886824822));
#20509=CARTESIAN_POINT('Ctrl Pts',(76.7419729648888,-4.05958480638017,49.6755096337063));
#20510=CARTESIAN_POINT('Ctrl Pts',(77.45941269056,-4.54316905747744,49.7210305849305));
#20511=CARTESIAN_POINT('Ctrl Pts',(78.2484504722489,-4.82934429562459,49.7665515361546));
#20512=CARTESIAN_POINT('Ctrl Pts',(79.0374882539378,-5.11551953377174,49.8120724873788));
#20513=CARTESIAN_POINT('Ctrl Pts',(79.8981240916443,-5.20428575896875,49.8575934386029));
#20514=CARTESIAN_POINT('Ctrl Pts',(80.7289621574045,-5.08518497666695,49.9031143898271));
#20515=CARTESIAN_POINT('Ctrl Pts',(81.5598002231647,-4.96608419436515,49.9486353410512));
#20516=CARTESIAN_POINT('Ctrl Pts',(82.3608405169786,-4.63911640456454,49.9941562922754));
#20517=CARTESIAN_POINT('Ctrl Pts',(83.0377084610454,-4.1428033237821,50.0396772434995));
#20518=CARTESIAN_POINT('Ctrl Pts',(83.7145764051122,-3.64649024299964,50.0851981947237));
#20519=CARTESIAN_POINT('Ctrl Pts',(84.267271999432,-2.98083187123535,50.1307191459478));
#20520=CARTESIAN_POINT('Ctrl Pts',(84.6306794018067,-2.22425276250945,50.1762400971719));
#20521=CARTESIAN_POINT('Ctrl Pts',(84.9940868041813,-1.46767365378356,50.2217610483961));
#20522=CARTESIAN_POINT('Ctrl Pts',(85.1682060146108,-0.620173808096055,
50.2672819996202));
#20523=CARTESIAN_POINT('Ctrl Pts',(85.1325231749308,0.218398563743828,50.3128029508444));
#20524=CARTESIAN_POINT('Ctrl Pts',(85.0968403352507,1.05697093558372,50.3583239020685));
#20525=CARTESIAN_POINT('Ctrl Pts',(84.8513554454613,1.88661583357599,50.4038448532927));
#20526=CARTESIAN_POINT('Ctrl Pts',(84.4249903126289,2.60958862792328,50.4493658045168));
#20527=CARTESIAN_POINT('Ctrl Pts',(83.9986251797964,3.33256142227058,50.494886755741));
#20528=CARTESIAN_POINT('Ctrl Pts',(83.3913798039212,3.94886211297289,50.5404077069651));
#20529=CARTESIAN_POINT('Ctrl Pts',(82.6747968107765,4.38588122216179,50.5859286581892));
#20530=CARTESIAN_POINT('Ctrl Pts',(81.9582138176319,4.82290033135069,50.6314496094134));
#20531=CARTESIAN_POINT('Ctrl Pts',(81.1322932072179,5.08063785902618,50.6769705606375));
#20532=CARTESIAN_POINT('Ctrl Pts',(80.2943408323192,5.12872845335609,50.7224915118616));
#20533=CARTESIAN_POINT('Ctrl Pts',(79.4563884574205,5.17681904768601,50.7680124630858));
#20534=CARTESIAN_POINT('Ctrl Pts',(78.606404318037,5.01526270867036,50.8135334143099));
#20535=CARTESIAN_POINT('Ctrl Pts',(77.8445293120887,4.66309319952182,50.8590543655341));
#20536=CARTESIAN_POINT('Ctrl Pts',(77.0826543061403,4.31092369037328,50.9045753167582));
#20537=CARTESIAN_POINT('Ctrl Pts',(76.408888433627,3.76814101109185,50.9500962679824));
#20538=CARTESIAN_POINT('Ctrl Pts',(75.9026114339255,3.09869311362241,50.9956172192065));
#20539=CARTESIAN_POINT('Ctrl Pts',(75.396334434224,2.42924521615298,51.0411381704307));
#20540=CARTESIAN_POINT('Ctrl Pts',(75.0575463073343,1.63313210049556,51.0866591216548));
#20541=CARTESIAN_POINT('Ctrl Pts',(74.9261613830222,0.804147848807305,51.1321800728789));
#20542=CARTESIAN_POINT('Ctrl Pts',(74.8840428677571,0.538397527435993,51.1467728801516));
#20543=CARTESIAN_POINT('Ctrl Pts',(74.8632386240357,0.269269127468966,51.1613656874243));
#20544=CARTESIAN_POINT('Ctrl Pts',(74.8634535980369,0.000107814451578703,
51.1759584946969));
#20545=CARTESIAN_POINT('Origin',(80.,0.,48.));
#20546=CARTESIAN_POINT('',(74.8630099039127,9.58920879684522E-5,52.9259584946969));
#20547=CARTESIAN_POINT('',(74.8636515713633,-1.05953972605244E-5,52.4490415053031));
#20548=CARTESIAN_POINT('',(74.86325,6.29070444552017E-16,48.));
#20549=CARTESIAN_POINT('',(83.8799476118145,3.36633437021263,54.));
#20550=CARTESIAN_POINT('Ctrl Pts',(74.8630099039127,9.58920879684522E-5,
52.9259584946969));
#20551=CARTESIAN_POINT('Ctrl Pts',(74.8636382796423,-0.725842401654488,
52.9653256712289));
#20552=CARTESIAN_POINT('Ctrl Pts',(75.0191418658014,-1.45204116294986,53.0046928477609));
#20553=CARTESIAN_POINT('Ctrl Pts',(75.3177903450041,-2.11362325386402,53.044060024293));
#20554=CARTESIAN_POINT('Ctrl Pts',(75.6631227780752,-2.878622137306,53.0895809755171));
#20555=CARTESIAN_POINT('Ctrl Pts',(76.1998499432974,-3.55722401379127,53.1351019267413));
#20556=CARTESIAN_POINT('Ctrl Pts',(76.8647368947113,-4.06947479034707,53.1806228779654));
#20557=CARTESIAN_POINT('Ctrl Pts',(77.5296238461253,-4.58172556690286,53.2261438291896));
#20558=CARTESIAN_POINT('Ctrl Pts',(78.3226705837311,-4.92762524352918,53.2716647804137));
#20559=CARTESIAN_POINT('Ctrl Pts',(79.1504451677981,-5.06643148578586,53.3171857316378));
#20560=CARTESIAN_POINT('Ctrl Pts',(79.9782197518651,-5.20523772804254,53.362706682862));
#20561=CARTESIAN_POINT('Ctrl Pts',(80.8407221823932,-5.13695053592958,53.4082276340861));
#20562=CARTESIAN_POINT('Ctrl Pts',(81.6363346794966,-4.86959432823606,53.4537485853103));
#20563=CARTESIAN_POINT('Ctrl Pts',(82.4319471766,-4.60223812054255,53.4992695365344));
#20564=CARTESIAN_POINT('Ctrl Pts',(83.1606697402787,-4.13581289726848,53.5447904877586));
#20565=CARTESIAN_POINT('Ctrl Pts',(83.7366512624658,-3.52531601118724,53.5903114389827));
#20566=CARTESIAN_POINT('Ctrl Pts',(84.312632784653,-2.914819125106,53.6358323902068));
#20567=CARTESIAN_POINT('Ctrl Pts',(84.7358732653486,-2.16025057621758,53.681353341431));
#20568=CARTESIAN_POINT('Ctrl Pts',(84.9564959299256,-1.35041792168183,53.7268742926551));
#20569=CARTESIAN_POINT('Ctrl Pts',(85.1771185945027,-0.540585267146073,
53.7723952438793));
#20570=CARTESIAN_POINT('Ctrl Pts',(85.1951234429612,0.324511493037019,53.8179161951034));
#20571=CARTESIAN_POINT('Ctrl Pts',(85.0083774710662,1.14270864307895,53.8634371463276));
#20572=CARTESIAN_POINT('Ctrl Pts',(84.821631499171,1.96090579312088,53.9089580975517));
#20573=CARTESIAN_POINT('Ctrl Pts',(84.4301347069223,2.73220333302164,53.9544790487759));
#20574=CARTESIAN_POINT('Ctrl Pts',(83.8799476118145,3.36633437021264,54.));
#20575=CARTESIAN_POINT('',(76.1197954215944,3.36643663068927,54.));
#20576=CARTESIAN_POINT('Origin',(80.,0.,54.));
#20577=CARTESIAN_POINT('Ctrl Pts',(76.1197954215944,3.36643663068927,54.));
#20578=CARTESIAN_POINT('Ctrl Pts',(76.5997425438788,3.91867143724511,53.9603227565005));
#20579=CARTESIAN_POINT('Ctrl Pts',(77.198769156323,4.36792997703869,53.920645513001));
#20580=CARTESIAN_POINT('Ctrl Pts',(77.8641232237026,4.67209812654765,53.8809682695015));
#20581=CARTESIAN_POINT('Ctrl Pts',(78.6274713642647,5.02106449307235,53.8354473182774));
#20582=CARTESIAN_POINT('Ctrl Pts',(79.478123276234,5.17905506715725,53.7899263670532));
#20583=CARTESIAN_POINT('Ctrl Pts',(80.315865632671,5.12744848588364,53.7444054158291));
#20584=CARTESIAN_POINT('Ctrl Pts',(81.1536079891079,5.07584190461002,53.6988844646049));
#20585=CARTESIAN_POINT('Ctrl Pts',(81.9784407900124,4.81463816797789,53.6533635133808));
#20586=CARTESIAN_POINT('Ctrl Pts',(82.693183411522,4.37461459180461,53.6078425621567));
#20587=CARTESIAN_POINT('Ctrl Pts',(83.4079260330316,3.93459101563133,53.5623216109325));
#20588=CARTESIAN_POINT('Ctrl Pts',(84.0125784751463,3.31574759991691,53.5168006597084));
#20589=CARTESIAN_POINT('Ctrl Pts',(84.4359049723902,2.59099170638668,53.4712797084842));
#20590=CARTESIAN_POINT('Ctrl Pts',(84.8592314696341,1.86623581285645,53.4257587572601));
#20591=CARTESIAN_POINT('Ctrl Pts',(85.1012320220073,1.03556744151041,53.3802378060359));
#20592=CARTESIAN_POINT('Ctrl Pts',(85.1333946855385,0.196852593275327,53.3347168548118));
#20593=CARTESIAN_POINT('Ctrl Pts',(85.1655573490699,-0.641862254959766,
53.2891959035876));
#20594=CARTESIAN_POINT('Ctrl Pts',(84.9878821237593,-1.48862358008391,53.2436749523635));
#20595=CARTESIAN_POINT('Ctrl Pts',(84.6213021217404,-2.24367055085715,53.1981540011394));
#20596=CARTESIAN_POINT('Ctrl Pts',(84.2547221197216,-2.9987175216304,53.1526330499152));
#20597=CARTESIAN_POINT('Ctrl Pts',(83.6992373409944,-3.66205013805274,53.1071120986911));
#20598=CARTESIAN_POINT('Ctrl Pts',(83.0202920939743,-4.15551768120208,53.0615911474669));
#20599=CARTESIAN_POINT('Ctrl Pts',(82.3413468469542,-4.6489852243514,53.0160701962428));
#20600=CARTESIAN_POINT('Ctrl Pts',(81.5389411316412,-4.97258769422772,52.9705492450186));
#20601=CARTESIAN_POINT('Ctrl Pts',(80.7076104593837,-5.08819994104047,52.9250282937945));
#20602=CARTESIAN_POINT('Ctrl Pts',(79.8762797871261,-5.20381218785322,52.8795073425703));
#20603=CARTESIAN_POINT('Ctrl Pts',(79.0160241579242,-5.1114342116024,52.8339863913462));
#20604=CARTESIAN_POINT('Ctrl Pts',(78.2281945743439,-4.82194948714952,52.7884654401221));
#20605=CARTESIAN_POINT('Ctrl Pts',(77.4403649907635,-4.53246476269664,52.7429444888979));
#20606=CARTESIAN_POINT('Ctrl Pts',(76.7249614528048,-4.04587329004171,52.6974235376738));
#20607=CARTESIAN_POINT('Ctrl Pts',(76.1662692568043,-3.41950287091639,52.6519025864496));
#20608=CARTESIAN_POINT('Ctrl Pts',(75.6075770608038,-2.79313245179107,52.6063816352255));
#20609=CARTESIAN_POINT('Ctrl Pts',(75.2055962067615,-2.02698308619534,52.5608606840013));
#20610=CARTESIAN_POINT('Ctrl Pts',(75.0076860699755,-1.21131866814437,52.5153397327772));
#20611=CARTESIAN_POINT('Ctrl Pts',(74.9116051012844,-0.815331738490969,
52.4932403236192));
#20612=CARTESIAN_POINT('Ctrl Pts',(74.8636212843626,-0.407674672990421,
52.4711409144611));
#20613=CARTESIAN_POINT('Ctrl Pts',(74.8636515713633,-1.05953972605244E-5,
52.4490415053031));
#20614=CARTESIAN_POINT('Origin',(80.,0.,57.8647410325605));
#20615=CARTESIAN_POINT('',(73.8872027408445,4.9881108922234E-5,43.1352589674395));
#20616=CARTESIAN_POINT('',(73.8867924003229,0.000144735339684834,42.9897410325605));
#20617=CARTESIAN_POINT('',(73.88675,2.47426426879123E-14,57.8647410325605));
#20618=CARTESIAN_POINT('',(85.6017891526601,-2.44781205398602,42.));
#20619=CARTESIAN_POINT('Ctrl Pts',(73.8867924003229,0.00014473533968537,
42.9897410325605));
#20620=CARTESIAN_POINT('Ctrl Pts',(73.8865552402621,0.247445601036081,42.9784740136094));
#20621=CARTESIAN_POINT('Ctrl Pts',(73.9608139639282,1.49374897980165,42.9216860434341));
#20622=CARTESIAN_POINT('Ctrl Pts',(74.7901455575896,3.65425999548639,42.8193771220346));
#20623=CARTESIAN_POINT('Ctrl Pts',(77.1247475918389,5.6770538401786,42.6828142683621));
#20624=CARTESIAN_POINT('Ctrl Pts',(80.1368351706977,6.36221026869802,42.5462514146897));
#20625=CARTESIAN_POINT('Ctrl Pts',(83.1167004331651,5.54813947205128,42.4096885610173));
#20626=CARTESIAN_POINT('Ctrl Pts',(85.3621237298141,3.42697795347734,42.2731257073449));
#20627=CARTESIAN_POINT('Ctrl Pts',(86.3441251020869,0.497881335996617,42.1365628536724));
#20628=CARTESIAN_POINT('Ctrl Pts',(86.0018547597101,-1.53226660829892,42.0455209512241));
#20629=CARTESIAN_POINT('Ctrl Pts',(85.6017891526601,-2.4478120539861,42.));
#20630=CARTESIAN_POINT('',(83.6329556492824,-4.91665117868322,42.));
#20631=CARTESIAN_POINT('Origin',(80.,0.,42.));
#20632=CARTESIAN_POINT('Ctrl Pts',(73.8872027408445,4.98811089222687E-5,
43.1352589674395));
#20633=CARTESIAN_POINT('Ctrl Pts',(73.8870723527698,0.441218568097294,43.1151632136948));
#20634=CARTESIAN_POINT('Ctrl Pts',(74.0409887873294,1.88163402125046,43.049546508726));
#20635=CARTESIAN_POINT('Ctrl Pts',(75.1606667541984,4.13243333827823,42.9384088525331));
#20636=CARTESIAN_POINT('Ctrl Pts',(77.6767884766317,5.92442701100857,42.8018459988606));
#20637=CARTESIAN_POINT('Ctrl Pts',(80.7403278321772,6.32044846892683,42.6652831451882));
#20638=CARTESIAN_POINT('Ctrl Pts',(83.6294253939595,5.22718080357853,42.5287202915158));
#20639=CARTESIAN_POINT('Ctrl Pts',(85.6633177227071,2.90223574469819,42.3921574378434));
#20640=CARTESIAN_POINT('Ctrl Pts',(86.3627699345494,-0.106570534545254,
42.2555945841709));
#20641=CARTESIAN_POINT('Ctrl Pts',(85.5971716734128,-2.96257437178865,42.1248754382231));
#20642=CARTESIAN_POINT('Ctrl Pts',(84.3329182412889,-4.39891812993667,42.0396772434995));
#20643=CARTESIAN_POINT('Ctrl Pts',(83.6330530644635,-4.91696557452334,42.));
#20644=CARTESIAN_POINT('Origin',(80.,0.,57.8647410325605));
#20645=CARTESIAN_POINT('',(73.8868174136284,0.000144937957391733,44.8852589674395));
#20646=CARTESIAN_POINT('',(73.8863051433301,5.93870499029922E-5,44.7397410325605));
#20647=CARTESIAN_POINT('',(73.88675,2.47426426879123E-14,57.8647410325605));
#20648=CARTESIAN_POINT('Ctrl Pts',(73.8863051433301,5.93870499033134E-5,
44.7397410325605));
#20649=CARTESIAN_POINT('Ctrl Pts',(73.8862731401809,0.0621168333236095,
44.7369130461899));
#20650=CARTESIAN_POINT('Ctrl Pts',(73.9021026716431,1.12307150188376,44.6885641085951));
#20651=CARTESIAN_POINT('Ctrl Pts',(74.4799467231356,3.16625379319216,44.5946942197762));
#20652=CARTESIAN_POINT('Ctrl Pts',(76.621290400294,5.39263133473806,44.4581313661038));
#20653=CARTESIAN_POINT('Ctrl Pts',(79.5587595524336,6.34834294257372,44.3215685124313));
#20654=CARTESIAN_POINT('Ctrl Pts',(82.6001982072725,5.80819426108823,44.1850056587589));
#20655=CARTESIAN_POINT('Ctrl Pts',(85.0289520597644,3.89946052862007,44.0484428050865));
#20656=CARTESIAN_POINT('Ctrl Pts',(86.272733737581,1.07189678402622,43.911879951414));
#20657=CARTESIAN_POINT('Ctrl Pts',(86.0384709317063,-2.00823809264104,43.7753170977416));
#20658=CARTESIAN_POINT('Ctrl Pts',(84.3813629617958,-4.61517164026814,43.6387542440692));
#20659=CARTESIAN_POINT('Ctrl Pts',(81.6918743166977,-6.13463234755794,43.5021913903967));
#20660=CARTESIAN_POINT('Ctrl Pts',(78.6037291538527,-6.20858889925048,43.3656285367243));
#20661=CARTESIAN_POINT('Ctrl Pts',(75.8445875723747,-4.81961646710041,43.2290656830519));
#20662=CARTESIAN_POINT('Ctrl Pts',(74.211443274136,-2.50328738630905,43.1037698483306));
#20663=CARTESIAN_POINT('Ctrl Pts',(73.8875134131035,-0.75169806720796,43.0239949648335));
#20664=CARTESIAN_POINT('Ctrl Pts',(73.8867924003229,0.00014473533968537,
42.9897410325605));
#20665=CARTESIAN_POINT('Ctrl Pts',(73.8868174136284,0.000144937957391837,
44.8852589674395));
#20666=CARTESIAN_POINT('Ctrl Pts',(73.8865748843346,0.256002452711397,44.8736022462753));
#20667=CARTESIAN_POINT('Ctrl Pts',(73.96394371651,1.51086982432855,44.8164245738871));
#20668=CARTESIAN_POINT('Ctrl Pts',(74.8055314959948,3.67609127100912,44.7137259502747));
#20669=CARTESIAN_POINT('Ctrl Pts',(77.1486004080237,5.68908344454576,44.5771630966022));
#20670=CARTESIAN_POINT('Ctrl Pts',(80.1635447169054,6.36155666463022,44.4406002429298));
#20671=CARTESIAN_POINT('Ctrl Pts',(83.1399529776901,5.53505604037131,44.3040373892574));
#20672=CARTESIAN_POINT('Ctrl Pts',(85.3764939963492,3.4043299457581,44.167474535585));
#20673=CARTESIAN_POINT('Ctrl Pts',(86.3461715250332,0.471441453942473,44.0309116819125));
#20674=CARTESIAN_POINT('Ctrl Pts',(85.8205004111942,-2.57253280683391,43.8943488282401));
#20675=CARTESIAN_POINT('Ctrl Pts',(83.9233445571365,-5.0103410604769,43.7577859745677));
#20676=CARTESIAN_POINT('Ctrl Pts',(81.1017308763422,-6.26756245882339,43.6212231208953));
#20677=CARTESIAN_POINT('Ctrl Pts',(78.020516297909,-6.04795786312262,43.4846602672228));
#20678=CARTESIAN_POINT('Ctrl Pts',(75.40572755909,-4.40327273783911,43.3480974135504));
#20679=CARTESIAN_POINT('Ctrl Pts',(74.0989624637806,-2.11574457800119,43.2316303136226));
#20680=CARTESIAN_POINT('Ctrl Pts',(73.88736770816,-0.558117835861341,43.160684164919));
#20681=CARTESIAN_POINT('Ctrl Pts',(73.8872027408445,4.98811089222687E-5,
43.1352589674395));
#20682=CARTESIAN_POINT('Origin',(80.,0.,57.8647410325605));
#20683=CARTESIAN_POINT('',(73.886319437839,6.68934239483887E-5,46.6352589674395));
#20684=CARTESIAN_POINT('',(73.8864333681599,-0.000106876724841452,46.4897410325605));
#20685=CARTESIAN_POINT('',(73.88675,2.47426426879123E-14,57.8647410325605));
#20686=CARTESIAN_POINT('Ctrl Pts',(73.88643336816,-0.000106876724841626,
46.4897410325606));
#20687=CARTESIAN_POINT('Ctrl Pts',(73.8871566616212,0.875730995516464,46.4498311275463));
#20688=CARTESIAN_POINT('Ctrl Pts',(74.2946407647659,2.7511948992005,46.364400271308));
#20689=CARTESIAN_POINT('Ctrl Pts',(76.1457328328429,5.06367217232759,46.2334484638453));
#20690=CARTESIAN_POINT('Ctrl Pts',(78.9843219438627,6.2820816096985,46.0968856101729));
#20691=CARTESIAN_POINT('Ctrl Pts',(82.0622353147722,6.02024391292702,45.9603227565005));
#20692=CARTESIAN_POINT('Ctrl Pts',(84.6542240982161,4.33985590869289,45.8237599028281));
#20693=CARTESIAN_POINT('Ctrl Pts',(86.149537876292,1.63686748781935,45.6871970491556));
#20694=CARTESIAN_POINT('Ctrl Pts',(86.1958358052853,-1.45181608290028,45.5506341954832));
#20695=CARTESIAN_POINT('Ctrl Pts',(84.7822087023876,-4.19840817351866,45.4140713418108));
#20696=CARTESIAN_POINT('Ctrl Pts',(82.2417495768579,-5.95572918282979,45.2775084881383));
#20697=CARTESIAN_POINT('Ctrl Pts',(79.1730669113078,-6.30970149306707,45.140945634466));
#20698=CARTESIAN_POINT('Ctrl Pts',(76.2992345216118,-5.17691859491353,45.0043827807935));
#20699=CARTESIAN_POINT('Ctrl Pts',(74.3388679796599,-2.87301696801453,44.8706479134917));
#20700=CARTESIAN_POINT('Ctrl Pts',(73.886788281912,-0.936796744990568,44.782433997414));
#20701=CARTESIAN_POINT('Ctrl Pts',(73.8863051433301,5.93870499033134E-5,
44.7397410325605));
#20702=CARTESIAN_POINT('Ctrl Pts',(73.886319437839,6.68934239489178E-5,
46.6352589674394));
#20703=CARTESIAN_POINT('Ctrl Pts',(73.8862791662938,0.0706764567001249,
46.6320412788559));
#20704=CARTESIAN_POINT('Ctrl Pts',(73.9044361060887,1.14018559218357,46.5833026390481));
#20705=CARTESIAN_POINT('Ctrl Pts',(74.4932859058703,3.18939648797121,46.4890430480163));
#20706=CARTESIAN_POINT('Ctrl Pts',(76.6439559920085,5.40676601013892,46.3524801943438));
#20707=CARTESIAN_POINT('Ctrl Pts',(79.5854108583403,6.35013904694908,46.2159173406715));
#20708=CARTESIAN_POINT('Ctrl Pts',(82.624555380254,5.79722857302948,46.079354486999));
#20709=CARTESIAN_POINT('Ctrl Pts',(85.0452758157915,3.87831690486471,45.9427916333266));
#20710=CARTESIAN_POINT('Ctrl Pts',(86.2771777145318,1.04555727349326,45.8062287796541));
#20711=CARTESIAN_POINT('Ctrl Pts',(86.0299879841389,-2.03356705891616,45.6696659259817));
#20712=CARTESIAN_POINT('Ctrl Pts',(84.3619519504042,-4.63352190610293,45.5331030723093));
#20713=CARTESIAN_POINT('Ctrl Pts',(81.6661090088627,-6.14167980625449,45.3965402186368));
#20714=CARTESIAN_POINT('Ctrl Pts',(78.5776807367317,-6.20267345467319,45.2599773649644));
#20715=CARTESIAN_POINT('Ctrl Pts',(75.8243936079491,-4.80213091560737,45.123414511292));
#20716=CARTESIAN_POINT('Ctrl Pts',(74.2060361265203,-2.48619421143874,44.9985083787837));
#20717=CARTESIAN_POINT('Ctrl Pts',(73.8875219915012,-0.743153080433105,
44.9191231974995));
#20718=CARTESIAN_POINT('Ctrl Pts',(73.8868174136284,0.000144937957391837,
44.8852589674395));
#20719=CARTESIAN_POINT('Origin',(80.,0.,57.8647410325605));
#20720=CARTESIAN_POINT('',(73.8864122443122,-0.000101181168932138,48.3852589674395));
#20721=CARTESIAN_POINT('',(73.8869623482907,-0.000132973038949946,48.2397410325606));
#20722=CARTESIAN_POINT('',(73.88675,2.47426426879123E-14,57.8647410325605));
#20723=CARTESIAN_POINT('Ctrl Pts',(73.8869623482907,-0.000132973038949845,
48.2397410325606));
#20724=CARTESIAN_POINT('Ctrl Pts',(73.887538634748,0.690679527368656,48.2082701601268));
#20725=CARTESIAN_POINT('Ctrl Pts',(74.1737315907217,2.38118134833958,48.131278336469));
#20726=CARTESIAN_POINT('Ctrl Pts',(75.701999226811,4.69290321850953,48.008765561587));
#20727=CARTESIAN_POINT('Ctrl Pts',(78.4182705988775,6.16395030530382,47.8722027079146));
#20728=CARTESIAN_POINT('Ctrl Pts',(81.507244931279,6.18258554180725,47.7356398542421));
#20729=CARTESIAN_POINT('Ctrl Pts',(84.2410670818731,4.74441790651735,47.5990770005697));
#20730=CARTESIAN_POINT('Ctrl Pts',(85.9755664309368,2.18832289529958,47.4625141468972));
#20731=CARTESIAN_POINT('Ctrl Pts',(86.3020428293569,-0.88340672488984,47.3259512932248));
#20732=CARTESIAN_POINT('Ctrl Pts',(85.1435686306702,-3.74697918411825,47.1893884395524));
#20733=CARTESIAN_POINT('Ctrl Pts',(82.7731151553917,-5.72765079239012,47.05282558588));
#20734=CARTESIAN_POINT('Ctrl Pts',(79.7492324481405,-6.35871582157629,46.9162627322075));
#20735=CARTESIAN_POINT('Ctrl Pts',(76.7844381088919,-5.49147639429357,46.7796998785351));
#20736=CARTESIAN_POINT('Ctrl Pts',(74.5773267431693,-3.33028017053867,46.6431370248627));
#20737=CARTESIAN_POINT('Ctrl Pts',(73.9195634847512,-1.24529947180603,46.5464840762045));
#20738=CARTESIAN_POINT('Ctrl Pts',(73.8863316782904,-0.123243395635752,
46.4953520787704));
#20739=CARTESIAN_POINT('Ctrl Pts',(73.88643336816,-0.000106876724841626,
46.4897410325606));
#20740=CARTESIAN_POINT('Ctrl Pts',(73.8864122443122,-0.000101181168932155,
48.3852589674395));
#20741=CARTESIAN_POINT('Ctrl Pts',(73.8871137806768,0.88427994577413,48.3449593602123));
#20742=CARTESIAN_POINT('Ctrl Pts',(74.3007018159247,2.76826051963491,48.259138801761));
#20743=CARTESIAN_POINT('Ctrl Pts',(76.1670218022879,5.07980592226054,48.1277972920855));
#20744=CARTESIAN_POINT('Ctrl Pts',(79.0107001846261,6.28628952143238,47.991234438413));
#20745=CARTESIAN_POINT('Ctrl Pts',(82.0874873209564,6.01153447605647,47.8546715847406));
#20746=CARTESIAN_POINT('Ctrl Pts',(84.6723997386214,4.32028132816605,47.7181087310682));
#20747=CARTESIAN_POINT('Ctrl Pts',(86.1563544240622,1.61104012280873,47.5815458773957));
#20748=CARTESIAN_POINT('Ctrl Pts',(86.1896870770046,-1.47781052937492,47.4449830237233));
#20749=CARTESIAN_POINT('Ctrl Pts',(84.7645435231389,-4.21844462901729,47.3084201700509));
#20750=CARTESIAN_POINT('Ctrl Pts',(82.2167303935176,-5.96508645657586,47.1718573163784));
#20751=CARTESIAN_POINT('Ctrl Pts',(79.1465889950142,-6.30617473025753,47.035294462706));
#20752=CARTESIAN_POINT('Ctrl Pts',(76.2775368648236,-5.1613388068622,46.8987316090336));
#20753=CARTESIAN_POINT('Ctrl Pts',(74.3325425970884,-2.85596626489593,46.7653864439447));
#20754=CARTESIAN_POINT('Ctrl Pts',(73.8868488917334,-0.928243855928552,
46.67756223008));
#20755=CARTESIAN_POINT('Ctrl Pts',(73.886319437839,6.68934239489178E-5,
46.6352589674394));
#20756=CARTESIAN_POINT('Origin',(80.,0.,57.8647410325605));
#20757=CARTESIAN_POINT('',(73.8869401609568,-0.000135895702726013,50.1352589674395));
#20758=CARTESIAN_POINT('',(73.8872292021947,-5.18097543697425E-6,49.9897410325606));
#20759=CARTESIAN_POINT('',(73.88675,2.47426426879123E-14,57.8647410325605));
#20760=CARTESIAN_POINT('Ctrl Pts',(73.8872292021947,-5.18097543696777E-6,
49.9897410325605));
#20761=CARTESIAN_POINT('Ctrl Pts',(73.8872446337552,0.505626675227688,49.9667091927074));
#20762=CARTESIAN_POINT('Ctrl Pts',(74.0720197357253,2.0106184806943,49.8981564016301));
#20763=CARTESIAN_POINT('Ctrl Pts',(75.2937534075295,4.28338584247207,49.7840826593286));
#20764=CARTESIAN_POINT('Ctrl Pts',(77.8652792970721,5.99492441863291,49.6475198056562));
#20765=CARTESIAN_POINT('Ctrl Pts',(80.939809508912,6.2938787207563,49.5109569519837));
#20766=CARTESIAN_POINT('Ctrl Pts',(83.792892369597,5.10980613499994,49.3743940983113));
#20767=CARTESIAN_POINT('Ctrl Pts',(85.7522558536446,2.72170973082036,49.2378312446388));
#20768=CARTESIAN_POINT('Ctrl Pts',(86.3562150670656,-0.307703243139823,
49.1012683909664));
#20769=CARTESIAN_POINT('Ctrl Pts',(85.4624590769004,-3.26461208994559,48.964705537294));
#20770=CARTESIAN_POINT('Ctrl Pts',(83.2815836418895,-5.45228026296463,48.8281426836216));
#20771=CARTESIAN_POINT('Ctrl Pts',(80.3274685256469,-6.35522742546172,48.6915798299491));
#20772=CARTESIAN_POINT('Ctrl Pts',(77.2961919879637,-5.76069210240215,48.5550169762767));
#20773=CARTESIAN_POINT('Ctrl Pts',(74.9020138373674,-3.80876467509304,48.4184541226043));
#20774=CARTESIAN_POINT('Ctrl Pts',(73.9839869412179,-1.61601829022539,48.3133621413656));
#20775=CARTESIAN_POINT('Ctrl Pts',(73.8867050668903,-0.308544189810323,
48.253791111351));
#20776=CARTESIAN_POINT('Ctrl Pts',(73.8869623482907,-0.000132973038949845,
48.2397410325606));
#20777=CARTESIAN_POINT('Ctrl Pts',(73.8869401609568,-0.000135895702726048,
50.1352589674395));
#20778=CARTESIAN_POINT('Ctrl Pts',(73.8875399757514,0.699223566656964,50.1033983927928));
#20779=CARTESIAN_POINT('Ctrl Pts',(74.1788859977704,2.39828340957575,50.026016866922));
#20780=CARTESIAN_POINT('Ctrl Pts',(75.7217357950776,4.71090282906051,49.9031143898271));
#20781=CARTESIAN_POINT('Ctrl Pts',(78.4441579740491,6.17053528166351,49.7665515361547));
#20782=CARTESIAN_POINT('Ctrl Pts',(81.5331832701364,6.17620426573987,49.6299886824822));
#20783=CARTESIAN_POINT('Ctrl Pts',(84.2609445326221,4.72657399835094,49.4934258288098));
#20784=CARTESIAN_POINT('Ctrl Pts',(85.9846992690839,2.16322091580975,49.3568629751373));
#20785=CARTESIAN_POINT('Ctrl Pts',(86.2982790838942,-0.909851995299122,
49.2203001214649));
#20786=CARTESIAN_POINT('Ctrl Pts',(85.1277951530875,-3.76853644535141,49.0837372677925));
#20787=CARTESIAN_POINT('Ctrl Pts',(82.7490486508255,-5.73924050614397,48.94717441412));
#20788=CARTESIAN_POINT('Ctrl Pts',(79.7225437079984,-6.35760710314802,48.8106115604476));
#20789=CARTESIAN_POINT('Ctrl Pts',(76.7614158020519,-5.47793049104956,48.6740487067752));
#20790=CARTESIAN_POINT('Ctrl Pts',(74.563395616688,-3.3074889041874,48.5374858531028));
#20791=CARTESIAN_POINT('Ctrl Pts',(73.9170067231604,-1.22818326457397,48.4412226066575));
#20792=CARTESIAN_POINT('Ctrl Pts',(73.886321351052,-0.114684384477866,48.3904803114364));
#20793=CARTESIAN_POINT('Ctrl Pts',(73.8864122443122,-0.000101181168932155,
48.3852589674395));
#20794=CARTESIAN_POINT('Origin',(80.,0.,57.8647410325605));
#20795=CARTESIAN_POINT('',(73.8872279103786,-1.26095903427159E-5,51.8852589674395));
#20796=CARTESIAN_POINT('',(73.8869923021753,0.000128310058932331,51.7397410325606));
#20797=CARTESIAN_POINT('',(73.88675,2.47426426879123E-14,57.8647410325605));
#20798=CARTESIAN_POINT('Ctrl Pts',(73.8869923021753,0.000128310058932178,
51.7397410325606));
#20799=CARTESIAN_POINT('Ctrl Pts',(73.8867364614564,0.320457389107717,51.7251482252879));
#20800=CARTESIAN_POINT('Ctrl Pts',(73.9887295387364,1.63986289423491,51.6650344667911));
#20801=CARTESIAN_POINT('Ctrl Pts',(74.9243661842076,3.83850135239988,51.5593997570702));
#20802=CARTESIAN_POINT('Ctrl Pts',(77.3299139839692,5.77639956476208,51.4228369033978));
#20803=CARTESIAN_POINT('Ctrl Pts',(80.3646142555919,6.35320452285083,51.2862740497253));
#20804=CARTESIAN_POINT('Ctrl Pts',(83.3134004559793,5.43300365203046,51.1497111960529));
#20805=CARTESIAN_POINT('Ctrl Pts',(85.481449977994,3.23262391926018,51.0131483423805));
#20806=CARTESIAN_POINT('Ctrl Pts',(86.3579052283988,0.270540886612342,50.8765854887081));
#20807=CARTESIAN_POINT('Ctrl Pts',(85.736247022437,-2.75528970567801,50.7400226350356));
#20808=CARTESIAN_POINT('Ctrl Pts',(83.7629567073689,-5.13189127740411,50.6034597813632));
#20809=CARTESIAN_POINT('Ctrl Pts',(80.903000756919,-6.2992651077435,50.4668969276907));
#20810=CARTESIAN_POINT('Ctrl Pts',(77.8302707029787,-5.98234285562748,50.3303340740183));
#20811=CARTESIAN_POINT('Ctrl Pts',(75.2687940477242,-4.25580092365468,50.1937712203459));
#20812=CARTESIAN_POINT('Ctrl Pts',(74.0661167021499,-1.98677733436168,50.0802402065266));
#20813=CARTESIAN_POINT('Ctrl Pts',(73.8872141342676,-0.493722191832877,
50.0122301439315));
#20814=CARTESIAN_POINT('Ctrl Pts',(73.8872292021947,-5.18097543696777E-6,
49.9897410325605));
#20815=CARTESIAN_POINT('Ctrl Pts',(73.8872279103786,-1.26095903429935E-5,
51.8852589674395));
#20816=CARTESIAN_POINT('Ctrl Pts',(73.8872661113861,0.514174273776074,51.8618374253733));
#20817=CARTESIAN_POINT('Ctrl Pts',(74.076305415408,2.02773695413552,51.7928949320831));
#20818=CARTESIAN_POINT('Ctrl Pts',(75.3117746142583,4.30310269326682,51.6784314875687));
#20819=CARTESIAN_POINT('Ctrl Pts',(77.8904620590793,6.00383208915477,51.5418686338962));
#20820=CARTESIAN_POINT('Ctrl Pts',(80.9662200126132,6.28987829428071,51.4053057802239));
#20821=CARTESIAN_POINT('Ctrl Pts',(83.8143075062239,5.09384023309799,51.2687429265514));
#20822=CARTESIAN_POINT('Ctrl Pts',(85.7636295740737,2.6975403991448,51.132180072879));
#20823=CARTESIAN_POINT('Ctrl Pts',(86.354867380944,-0.334380983822473,50.9956172192065));
#20824=CARTESIAN_POINT('Ctrl Pts',(85.4487075396391,-3.28751216265552,50.8590543655341));
#20825=CARTESIAN_POINT('Ctrl Pts',(83.258668528712,-5.46600672263342,50.7224915118617));
#20826=CARTESIAN_POINT('Ctrl Pts',(80.3007893255799,-6.35654590588445,50.5859286581892));
#20827=CARTESIAN_POINT('Ctrl Pts',(77.2720351219492,-5.74929192997566,50.4493658045168));
#20828=CARTESIAN_POINT('Ctrl Pts',(74.8860713886881,-3.78733207289439,50.3128029508444));
#20829=CARTESIAN_POINT('Ctrl Pts',(73.9806267980956,-1.59889694717195,50.2081006718186));
#20830=CARTESIAN_POINT('Ctrl Pts',(73.8866829874418,-0.299989671876453,
50.148919344017));
#20831=CARTESIAN_POINT('Ctrl Pts',(73.8869401609568,-0.000135895702726048,
50.1352589674395));
#20832=CARTESIAN_POINT('Origin',(80.,0.,57.8647410325605));
#20833=CARTESIAN_POINT('',(73.8870077577991,0.000138281717805,53.6352589674395));
#20834=CARTESIAN_POINT('',(73.8864642614677,0.000114121245111251,53.4897410325605));
#20835=CARTESIAN_POINT('',(73.88675,2.47426426879123E-14,57.8647410325605));
#20836=CARTESIAN_POINT('',(78.4211181181246,-5.90584097022478,54.));
#20837=CARTESIAN_POINT('Ctrl Pts',(78.4211181181246,-5.90584097022479,54.));
#20838=CARTESIAN_POINT('Ctrl Pts',(77.455879038986,-5.647791608345,53.9544790487759));
#20839=CARTESIAN_POINT('Ctrl Pts',(75.6552430725963,-4.64961437394933,53.8634371463276));
#20840=CARTESIAN_POINT('Ctrl Pts',(74.161524344143,-2.34018528006132,53.7418568021407));
#20841=CARTESIAN_POINT('Ctrl Pts',(73.8875141280071,-0.670206627459226,
53.665797409178));
#20842=CARTESIAN_POINT('Ctrl Pts',(73.8870077577991,0.000138281717805347,
53.6352589674395));
#20843=CARTESIAN_POINT('',(81.5790669755174,-5.90611323035058,54.));
#20844=CARTESIAN_POINT('Origin',(80.,0.,54.));
#20845=CARTESIAN_POINT('Ctrl Pts',(81.5790669755174,-5.90611323035057,54.));
#20846=CARTESIAN_POINT('Ctrl Pts',(80.7376823715278,-6.13029255477271,53.9603227565005));
#20847=CARTESIAN_POINT('Ctrl Pts',(78.8264544132615,-6.2231800657142,53.8751245617769));
#20848=CARTESIAN_POINT('Ctrl Pts',(76.1161979867926,-5.04105954615917,53.7444054158291));
#20849=CARTESIAN_POINT('Ctrl Pts',(74.2862708285712,-2.72742222003944,53.6139963368488));
#20850=CARTESIAN_POINT('Ctrl Pts',(73.8872120918914,-0.863825582696248,
53.5291082090926));
#20851=CARTESIAN_POINT('Ctrl Pts',(73.8864642614677,0.000114121245111225,
53.4897410325605));
#20852=CARTESIAN_POINT('Origin',(32.,-32.,48.));
#20853=CARTESIAN_POINT('',(33.6684805778295,-31.9993859124995,53.3285196366098));
#20854=CARTESIAN_POINT('',(33.6648118344815,-31.9985150168184,53.5214803633902));
#20855=CARTESIAN_POINT('',(33.666,-32.,48.));
#20856=CARTESIAN_POINT('',(31.3249228143251,-33.5230977622534,54.));
#20857=CARTESIAN_POINT('Ctrl Pts',(33.6648118344815,-31.9985150168184,53.5214803633902));
#20858=CARTESIAN_POINT('Ctrl Pts',(33.6661629666675,-31.8287715688263,53.5328138566339));
#20859=CARTESIAN_POINT('Ctrl Pts',(33.6422867594775,-31.659410867237,53.5441473498775));
#20860=CARTESIAN_POINT('Ctrl Pts',(33.5916050633703,-31.4985170507268,53.5554808431211));
#20861=CARTESIAN_POINT('Ctrl Pts',(33.4259531005074,-30.9726392967347,53.5925241061943));
#20862=CARTESIAN_POINT('Ctrl Pts',(32.973939640304,-30.537212789371,53.6295673692676));
#20863=CARTESIAN_POINT('Ctrl Pts',(32.442142359202,-30.3909996812704,53.6666106323408));
#20864=CARTESIAN_POINT('Ctrl Pts',(31.9103450780999,-30.2447865731697,53.703653895414));
#20865=CARTESIAN_POINT('Ctrl Pts',(31.2987639760992,-30.387786864332,53.7406971584873));
#20866=CARTESIAN_POINT('Ctrl Pts',(30.8877751462098,-30.7555547378681,53.7777404215606));
#20867=CARTESIAN_POINT('Ctrl Pts',(30.4767863163205,-31.1233226114042,53.8147836846338));
#20868=CARTESIAN_POINT('Ctrl Pts',(30.2663897585425,-31.7158580673142,53.851826947707));
#20869=CARTESIAN_POINT('Ctrl Pts',(30.351816552213,-32.2596861396068,53.8888702107803));
#20870=CARTESIAN_POINT('Ctrl Pts',(30.4372433458836,-32.8035142118994,53.9259134738535));
#20871=CARTESIAN_POINT('Ctrl Pts',(30.8184934910026,-33.2986349005747,53.9629567369268));
#20872=CARTESIAN_POINT('Ctrl Pts',(31.3249228143251,-33.5230977622534,54.));
#20873=CARTESIAN_POINT('',(33.666,-32.,54.));
#20874=CARTESIAN_POINT('Origin',(32.,-32.,54.));
#20875=CARTESIAN_POINT('',(33.666,-32.,55.));
#20876=CARTESIAN_POINT('',(33.666,-32.,48.));
#20877=CARTESIAN_POINT('Origin',(32.,-32.,55.));
#20878=CARTESIAN_POINT('',(33.6146716598692,-32.4224676707571,54.));
#20879=CARTESIAN_POINT('Origin',(32.,-32.,54.));
#20880=CARTESIAN_POINT('Ctrl Pts',(33.6146732908669,-32.4224680167337,54.));
#20881=CARTESIAN_POINT('Ctrl Pts',(33.4771404824827,-32.9453622991658,53.9636851831628));
#20882=CARTESIAN_POINT('Ctrl Pts',(33.0618476186246,-33.3962238432118,53.9273703663255));
#20883=CARTESIAN_POINT('Ctrl Pts',(32.5515251931148,-33.574862517777,53.8910555494883));
#20884=CARTESIAN_POINT('Ctrl Pts',(32.0309661071345,-33.7570845415485,53.854012286415));
#20885=CARTESIAN_POINT('Ctrl Pts',(31.4115267880172,-33.6560530141969,53.8169690233418));
#20886=CARTESIAN_POINT('Ctrl Pts',(30.9761676664273,-33.3177477807437,53.7799257602686));
#20887=CARTESIAN_POINT('Ctrl Pts',(30.5408085448373,-32.9794425472904,53.7428824971953));
#20888=CARTESIAN_POINT('Ctrl Pts',(30.2895296207747,-32.4038636077355,53.7058392341221));
#20889=CARTESIAN_POINT('Ctrl Pts',(30.3375623733908,-31.8545189866324,53.6687959710489));
#20890=CARTESIAN_POINT('Ctrl Pts',(30.3855951260069,-31.3051743655294,53.6317527079756));
#20891=CARTESIAN_POINT('Ctrl Pts',(30.7329395553015,-30.7820640628781,53.5947094449023));
#20892=CARTESIAN_POINT('Ctrl Pts',(31.2205277178506,-30.5244968291776,53.5576661818291));
#20893=CARTESIAN_POINT('Ctrl Pts',(31.7081158803996,-30.2669295954771,53.5206229187558));
#20894=CARTESIAN_POINT('Ctrl Pts',(32.335947776203,-30.2749054307274,53.4835796556826));
#20895=CARTESIAN_POINT('Ctrl Pts',(32.8167940806439,-30.5448068015671,53.4465363926094));
#20896=CARTESIAN_POINT('Ctrl Pts',(33.2976403850846,-30.8147081724067,53.4094931295362));
#20897=CARTESIAN_POINT('Ctrl Pts',(33.6315010981628,-31.3465350788358,53.3724498664629));
#20898=CARTESIAN_POINT('Ctrl Pts',(33.6655714697797,-31.8969101642465,53.3354066033897));
#20899=CARTESIAN_POINT('Ctrl Pts',(33.6676828885014,-31.9310181649572,53.3331109477964));
#20900=CARTESIAN_POINT('Ctrl Pts',(33.6686429432612,-31.9651974011345,53.3308152922031));
#20901=CARTESIAN_POINT('Ctrl Pts',(33.6684805778295,-31.9993859124995,53.3285196366098));
#20902=CARTESIAN_POINT('Origin',(32.,-32.,48.));
#20903=CARTESIAN_POINT('',(33.6641301080328,-31.9988695643883,52.6285196366098));
#20904=CARTESIAN_POINT('',(33.6637769838569,-32.0008964513587,52.8214803633902));
#20905=CARTESIAN_POINT('',(33.666,-32.,48.));
#20906=CARTESIAN_POINT('Ctrl Pts',(33.6637769838569,-32.0008964513587,52.8214803633902));
#20907=CARTESIAN_POINT('Ctrl Pts',(33.6621335736406,-31.664768877266,52.8438876115277));
#20908=CARTESIAN_POINT('Ctrl Pts',(33.563356481064,-31.3277533767314,52.8662948596652));
#20909=CARTESIAN_POINT('Ctrl Pts',(33.374088211561,-31.0530981103508,52.8887021078028));
#20910=CARTESIAN_POINT('Ctrl Pts',(33.0611932832952,-30.599042921398,52.925745370876));
#20911=CARTESIAN_POINT('Ctrl Pts',(32.50098494745,-30.3154189560176,52.9627886339492));
#20912=CARTESIAN_POINT('Ctrl Pts',(31.9498071641372,-30.3320029614108,52.9998318970225));
#20913=CARTESIAN_POINT('Ctrl Pts',(31.3986293808243,-30.348586966804,53.0368751600957));
#20914=CARTESIAN_POINT('Ctrl Pts',(30.8564821500439,-30.6653789429709,53.073918423169));
#20915=CARTESIAN_POINT('Ctrl Pts',(30.5714576898881,-31.1374325180527,53.1109616862422));
#20916=CARTESIAN_POINT('Ctrl Pts',(30.2864332297323,-31.6094860931344,53.1480049493154));
#20917=CARTESIAN_POINT('Ctrl Pts',(30.2585315402012,-32.2368012671311,53.1850482123886));
#20918=CARTESIAN_POINT('Ctrl Pts',(30.5005032885542,-32.7322905055208,53.2220914754619));
#20919=CARTESIAN_POINT('Ctrl Pts',(30.7424750369073,-33.2277797439105,53.2591347385351));
#20920=CARTESIAN_POINT('Ctrl Pts',(31.2543202231446,-33.5914430466933,53.2961780016084));
#20921=CARTESIAN_POINT('Ctrl Pts',(31.8018549075792,-33.656932440832,53.3332212646817));
#20922=CARTESIAN_POINT('Ctrl Pts',(32.3493895920138,-33.7224218349707,53.3702645277549));
#20923=CARTESIAN_POINT('Ctrl Pts',(32.9326137746457,-33.4897373204654,53.4073077908281));
#20924=CARTESIAN_POINT('Ctrl Pts',(33.2845806332005,-33.0652305629025,53.4443510539014));
#20925=CARTESIAN_POINT('Ctrl Pts',(33.5288622156088,-32.7706028729368,53.470060823731));
#20926=CARTESIAN_POINT('Ctrl Pts',(33.6617468220652,-32.3835741406163,53.4957705935606));
#20927=CARTESIAN_POINT('Ctrl Pts',(33.6648118344815,-31.9985150168184,53.5214803633902));
#20928=CARTESIAN_POINT('Ctrl Pts',(33.6684805778295,-31.9993859124995,53.3285196366098));
#20929=CARTESIAN_POINT('Ctrl Pts',(33.6660229747349,-32.5168716262576,53.2937720291298));
#20930=CARTESIAN_POINT('Ctrl Pts',(33.406412239859,-33.0364823406136,53.2590244216499));
#20931=CARTESIAN_POINT('Ctrl Pts',(32.9900196909147,-33.3433519640963,53.2242768141699));
#20932=CARTESIAN_POINT('Ctrl Pts',(32.5461175102774,-33.6704954141429,53.1872335510967));
#20933=CARTESIAN_POINT('Ctrl Pts',(31.9240331188471,-33.7558590498438,53.1501902880235));
#20934=CARTESIAN_POINT('Ctrl Pts',(31.408420821415,-33.5603767883024,53.1131470249502));
#20935=CARTESIAN_POINT('Ctrl Pts',(30.8928085239829,-33.364894526761,53.076103761877));
#20936=CARTESIAN_POINT('Ctrl Pts',(30.483668320549,-32.8885663679775,53.0390604988037));
#20937=CARTESIAN_POINT('Ctrl Pts',(30.3682246614595,-32.3493595890129,53.0020172357305));
#20938=CARTESIAN_POINT('Ctrl Pts',(30.2527810023701,-31.8101528100483,52.9649739726572));
#20939=CARTESIAN_POINT('Ctrl Pts',(30.4310338876251,-31.2080674109028,52.927930709584));
#20940=CARTESIAN_POINT('Ctrl Pts',(30.8214136864304,-30.8186133475755,52.8908874465107));
#20941=CARTESIAN_POINT('Ctrl Pts',(31.2117934852357,-30.4291592842482,52.8538441834375));
#20942=CARTESIAN_POINT('Ctrl Pts',(31.8143001975914,-30.2523365567391,52.8168009203643));
#20943=CARTESIAN_POINT('Ctrl Pts',(32.3532310680952,-30.3690588208124,52.779757657291));
#20944=CARTESIAN_POINT('Ctrl Pts',(32.892161938599,-30.4857810848857,52.7427143942178));
#20945=CARTESIAN_POINT('Ctrl Pts',(33.3675169672511,-30.8960483405412,52.7056711311445));
#20946=CARTESIAN_POINT('Ctrl Pts',(33.5617757404346,-31.4121242462018,52.6686278680713));
#20947=CARTESIAN_POINT('Ctrl Pts',(33.6318863371789,-31.5983829624405,52.6552584575841));
#20948=CARTESIAN_POINT('Ctrl Pts',(33.6653817597626,-31.7984241538003,52.641889047097));
#20949=CARTESIAN_POINT('Ctrl Pts',(33.6641301080328,-31.9988695643883,52.6285196366098));
#20950=CARTESIAN_POINT('Origin',(32.,-32.,48.));
#20951=CARTESIAN_POINT('',(33.6643835906196,-32.0012498155686,51.9285196366098));
#20952=CARTESIAN_POINT('',(33.6681251706529,-32.0009136526364,52.1214803633902));
#20953=CARTESIAN_POINT('',(33.666,-32.,48.));
#20954=CARTESIAN_POINT('Ctrl Pts',(33.6681251706529,-32.0009136526364,52.1214803633902));
#20955=CARTESIAN_POINT('Ctrl Pts',(33.6648306539093,-31.5020153412742,52.1549613664216));
#20956=CARTESIAN_POINT('Ctrl Pts',(33.4261511460292,-31.0003826202633,52.188442369453));
#20957=CARTESIAN_POINT('Ctrl Pts',(33.0352551049814,-30.6911883151967,52.2219233724844));
#20958=CARTESIAN_POINT('Ctrl Pts',(32.6027691107821,-30.3490968320775,52.2589666355576));
#20959=CARTESIAN_POINT('Ctrl Pts',(31.9839528618204,-30.2425717379885,52.2960098986308));
#20960=CARTESIAN_POINT('Ctrl Pts',(31.461973246163,-30.4203582047467,52.3330531617041));
#20961=CARTESIAN_POINT('Ctrl Pts',(30.9399936305057,-30.598144671505,52.3700964247773));
#20962=CARTESIAN_POINT('Ctrl Pts',(30.5148506481528,-31.0602426991104,52.4071396878506));
#20963=CARTESIAN_POINT('Ctrl Pts',(30.3810875652485,-31.5951990002834,52.4441829509239));
#20964=CARTESIAN_POINT('Ctrl Pts',(30.2473244823442,-32.1301553014564,52.4812262139971));
#20965=CARTESIAN_POINT('Ctrl Pts',(30.4049412988885,-32.7379698761969,52.5182694770703));
#20966=CARTESIAN_POINT('Ctrl Pts',(30.7818131318635,-33.1405095471833,52.5553127401435));
#20967=CARTESIAN_POINT('Ctrl Pts',(31.1586849648385,-33.5430492181697,52.5923560032168));
#20968=CARTESIAN_POINT('Ctrl Pts',(31.7548118142443,-33.740313985402,52.62939926629));
#20969=CARTESIAN_POINT('Ctrl Pts',(32.2974098252054,-33.6420375976381,52.6664425293633));
#20970=CARTESIAN_POINT('Ctrl Pts',(32.8400078361665,-33.5437612098741,52.7034857924365));
#20971=CARTESIAN_POINT('Ctrl Pts',(33.329077008683,-33.1499436671139,52.7405290555098));
#20972=CARTESIAN_POINT('Ctrl Pts',(33.540820834598,-32.6407916894713,52.777572318583));
#20973=CARTESIAN_POINT('Ctrl Pts',(33.6244820874556,-32.439622695946,52.7922083335187));
#20974=CARTESIAN_POINT('Ctrl Pts',(33.6648504301063,-32.2204489892046,52.8068443484545));
#20975=CARTESIAN_POINT('Ctrl Pts',(33.6637769838569,-32.0008964513587,52.8214803633902));
#20976=CARTESIAN_POINT('Ctrl Pts',(33.6641301080328,-31.9988695643883,52.6285196366098));
#20977=CARTESIAN_POINT('Ctrl Pts',(33.6619137486376,-32.3538078098979,52.6048457840237));
#20978=CARTESIAN_POINT('Ctrl Pts',(33.5507462927464,-32.7100135039337,52.5811719314377));
#20979=CARTESIAN_POINT('Ctrl Pts',(33.3409999223511,-32.9932070489303,52.5574980788516));
#20980=CARTESIAN_POINT('Ctrl Pts',(33.0128028133694,-33.4363293903327,52.5204548157783));
#20981=CARTESIAN_POINT('Ctrl Pts',(32.443246077691,-33.7006895174718,52.4834115527051));
#20982=CARTESIAN_POINT('Ctrl Pts',(31.8929556540234,-33.6653176007117,52.4463682896318));
#20983=CARTESIAN_POINT('Ctrl Pts',(31.3426652303558,-33.6299456839516,52.4093250265586));
#20984=CARTESIAN_POINT('Ctrl Pts',(30.8116411186989,-33.2948417232924,52.3722817634854));
#20985=CARTESIAN_POINT('Ctrl Pts',(30.5428771415083,-32.8133475089059,52.3352385004122));
#20986=CARTESIAN_POINT('Ctrl Pts',(30.2741131643176,-32.3318532945195,52.2981952373389));
#20987=CARTESIAN_POINT('Ctrl Pts',(30.2676093215931,-31.7039688264058,52.2611519742656));
#20988=CARTESIAN_POINT('Ctrl Pts',(30.5263417019884,-31.2170106150328,52.2241087111924));
#20989=CARTESIAN_POINT('Ctrl Pts',(30.7850740823836,-30.7300524036599,52.1870654481191));
#20990=CARTESIAN_POINT('Ctrl Pts',(31.3090426858984,-30.3840204490277,52.1500221850459));
#20991=CARTESIAN_POINT('Ctrl Pts',(31.8584823380995,-30.3372571061758,52.1129789219727));
#20992=CARTESIAN_POINT('Ctrl Pts',(32.4079219903006,-30.2904937633239,52.0759356588994));
#20993=CARTESIAN_POINT('Ctrl Pts',(32.982832691188,-30.5429990322524,52.0388923958262));
#20994=CARTESIAN_POINT('Ctrl Pts',(33.3201384125524,-30.9792278665667,52.0018491327529));
#20995=CARTESIAN_POINT('Ctrl Pts',(33.5427111247615,-31.2670754441422,51.9774059673719));
#20996=CARTESIAN_POINT('Ctrl Pts',(33.6618287241732,-31.6349177348701,51.9529628019908));
#20997=CARTESIAN_POINT('Ctrl Pts',(33.6643835906196,-32.0012498155686,51.9285196366098));
#20998=CARTESIAN_POINT('Origin',(32.,-32.,48.));
#20999=CARTESIAN_POINT('',(33.6686262364557,-32.0004179151258,51.2285196366098));
#21000=CARTESIAN_POINT('',(33.6665286247185,-31.9985210141682,51.4214803633902));
#21001=CARTESIAN_POINT('',(33.666,-32.,48.));
#21002=CARTESIAN_POINT('Ctrl Pts',(33.6665286247185,-31.9985210141682,51.4214803633902));
#21003=CARTESIAN_POINT('Ctrl Pts',(33.6675618774755,-31.8863136434922,51.4289918582422));
#21004=CARTESIAN_POINT('Ctrl Pts',(33.6571969459659,-31.774296080394,51.4365033530943));
#21005=CARTESIAN_POINT('Ctrl Pts',(33.634733907746,-31.6647595174629,51.4440148479463));
#21006=CARTESIAN_POINT('Ctrl Pts',(33.5239564592356,-31.1245752003957,51.4810581110195));
#21007=CARTESIAN_POINT('Ctrl Pts',(33.1189515966928,-30.6447291065599,51.5181013740928));
#21008=CARTESIAN_POINT('Ctrl Pts',(32.6050473497745,-30.4447962077593,51.555144637166));
#21009=CARTESIAN_POINT('Ctrl Pts',(32.0911431028562,-30.2448633089587,51.5921879002393));
#21010=CARTESIAN_POINT('Ctrl Pts',(31.4683394715624,-30.3248436051933,51.6292311633125));
#21011=CARTESIAN_POINT('Ctrl Pts',(31.0216280193636,-30.6481385443608,51.6662744263857));
#21012=CARTESIAN_POINT('Ctrl Pts',(30.5749165671649,-30.9714334835282,51.703317689459));
#21013=CARTESIAN_POINT('Ctrl Pts',(30.3042972940611,-31.5380430656285,51.7403609525322));
#21014=CARTESIAN_POINT('Ctrl Pts',(30.3336041144233,-32.0886898226008,51.7774042156055));
#21015=CARTESIAN_POINT('Ctrl Pts',(30.3629109347855,-32.6393365795731,51.8144474786787));
#21016=CARTESIAN_POINT('Ctrl Pts',(30.6921438486138,-33.1740205114175,51.8514907417519));
#21017=CARTESIAN_POINT('Ctrl Pts',(31.1706476550385,-33.448073141423,51.8885340048252));
#21018=CARTESIAN_POINT('Ctrl Pts',(31.6491514614632,-33.7221257714285,51.9255772678984));
#21019=CARTESIAN_POINT('Ctrl Pts',(32.2769261604843,-33.735547099595,51.9626205309717));
#21020=CARTESIAN_POINT('Ctrl Pts',(32.7667054630863,-33.4821956161538,51.9996637940449));
#21021=CARTESIAN_POINT('Ctrl Pts',(33.2564847656884,-33.2288441327127,52.0367070571182));
#21022=CARTESIAN_POINT('Ctrl Pts',(33.6082686718714,-32.7087198376638,52.0737503201914));
#21023=CARTESIAN_POINT('Ctrl Pts',(33.6610827552445,-32.1598287540646,52.1107935832646));
#21024=CARTESIAN_POINT('Ctrl Pts',(33.6661616139421,-32.1070447223078,52.1143558433065));
#21025=CARTESIAN_POINT('Ctrl Pts',(33.6684756955563,-32.053994664512,52.1179181033483));
#21026=CARTESIAN_POINT('Ctrl Pts',(33.6681251706529,-32.0009136526364,52.1214803633902));
#21027=CARTESIAN_POINT('Ctrl Pts',(33.6643835906196,-32.0012498155686,51.9285196366098));
#21028=CARTESIAN_POINT('Ctrl Pts',(33.6657005872652,-32.1900886968112,51.9159195389176));
#21029=CARTESIAN_POINT('Ctrl Pts',(33.6360439148516,-32.3785262770164,51.9033194412254));
#21030=CARTESIAN_POINT('Ctrl Pts',(33.5736181236639,-32.5553982113817,51.8907193435332));
#21031=CARTESIAN_POINT('Ctrl Pts',(33.3900913715693,-33.0753873221826,51.85367608046));
#21032=CARTESIAN_POINT('Ctrl Pts',(32.9233371255385,-33.4954131440844,51.8166328173867));
#21033=CARTESIAN_POINT('Ctrl Pts',(32.3869395954384,-33.6232741373353,51.7795895543135));
#21034=CARTESIAN_POINT('Ctrl Pts',(31.8505420653383,-33.7511351305863,51.7425462912403));
#21035=CARTESIAN_POINT('Ctrl Pts',(31.244501251169,-33.5868312951865,51.705503028167));
#21036=CARTESIAN_POINT('Ctrl Pts',(30.8461381445101,-33.2055471758926,51.6684597650938));
#21037=CARTESIAN_POINT('Ctrl Pts',(30.4477750378511,-32.8242630565987,51.6314165020205));
#21038=CARTESIAN_POINT('Ctrl Pts',(30.2570896387025,-32.2259986534107,51.5943732389472));
#21039=CARTESIAN_POINT('Ctrl Pts',(30.3613385511927,-31.6845165129817,51.557329975874));
#21040=CARTESIAN_POINT('Ctrl Pts',(30.4655874636828,-31.1430343725527,51.5202867128007));
#21041=CARTESIAN_POINT('Ctrl Pts',(30.8647706878118,-30.6583344948828,51.4832434497275));
#21042=CARTESIAN_POINT('Ctrl Pts',(31.3762241449887,-30.4522129159655,51.4462001866543));
#21043=CARTESIAN_POINT('Ctrl Pts',(31.8876776021656,-30.2460913370482,51.4091569235811));
#21044=CARTESIAN_POINT('Ctrl Pts',(32.5114012923905,-30.3185480568836,51.3721136605078));
#21045=CARTESIAN_POINT('Ctrl Pts',(32.9619826368709,-30.6364272732807,51.3350703974346));
#21046=CARTESIAN_POINT('Ctrl Pts',(33.3939980793994,-30.9412084898682,51.2995534771596));
#21047=CARTESIAN_POINT('Ctrl Pts',(33.6668456440257,-31.4716039419519,51.2640365568847));
#21048=CARTESIAN_POINT('Ctrl Pts',(33.6686262364557,-32.0004179151258,51.2285196366098));
#21049=CARTESIAN_POINT('Origin',(32.,-32.,48.));
#21050=CARTESIAN_POINT('',(33.6656097964572,-31.9984850050081,50.5285196366098));
#21051=CARTESIAN_POINT('',(33.6632910498763,-32.0000156711391,50.7214803633902));
#21052=CARTESIAN_POINT('',(33.666,-32.,48.));
#21053=CARTESIAN_POINT('Ctrl Pts',(33.6632910498763,-32.0000156711391,50.7214803633902));
#21054=CARTESIAN_POINT('Ctrl Pts',(33.663267639484,-31.7210181193327,50.7400656131361));
#21055=CARTESIAN_POINT('Ctrl Pts',(33.5968497698977,-31.4420100931612,50.758650862882));
#21056=CARTESIAN_POINT('Ctrl Pts',(33.4640996060852,-31.1992794035667,50.7772361126279));
#21057=CARTESIAN_POINT('Ctrl Pts',(33.1995080989302,-30.7154797821718,50.8142793757012));
#21058=CARTESIAN_POINT('Ctrl Pts',(32.6714007751648,-30.3757977747389,50.8513226387744));
#21059=CARTESIAN_POINT('Ctrl Pts',(32.1214366826114,-30.3356700260391,50.8883659018477));
#21060=CARTESIAN_POINT('Ctrl Pts',(31.571472590058,-30.2955422773393,50.9254091649209));
#21061=CARTESIAN_POINT('Ctrl Pts',(30.9996517287167,-30.5549687873725,50.9624524279942));
#21062=CARTESIAN_POINT('Ctrl Pts',(30.6676362241477,-30.9952373917923,50.9994956910674));
#21063=CARTESIAN_POINT('Ctrl Pts',(30.3356207195788,-31.4355059962121,51.0365389541406));
#21064=CARTESIAN_POINT('Ctrl Pts',(30.2434105717823,-32.0566166950185,51.0735822172139));
#21065=CARTESIAN_POINT('Ctrl Pts',(30.4332006444406,-32.5743526003433,51.1106254802871));
#21066=CARTESIAN_POINT('Ctrl Pts',(30.6229907170988,-33.0920885056681,51.1476687433603));
#21067=CARTESIAN_POINT('Ctrl Pts',(31.0947810102119,-33.5064496175111,51.1847120064336));
#21068=CARTESIAN_POINT('Ctrl Pts',(31.6326828437495,-33.6278265377282,51.2217552695068));
#21069=CARTESIAN_POINT('Ctrl Pts',(32.1705846772872,-33.7492034579452,51.2587985325801));
#21070=CARTESIAN_POINT('Ctrl Pts',(32.7745980512495,-33.5775961865362,51.2958417956533));
#21071=CARTESIAN_POINT('Ctrl Pts',(33.1683297209918,-33.1915312806824,51.3328850587266));
#21072=CARTESIAN_POINT('Ctrl Pts',(33.4822219499024,-32.8837511778476,51.3624168269478));
#21073=CARTESIAN_POINT('Ctrl Pts',(33.6624663466319,-32.4396691649416,51.391948595169));
#21074=CARTESIAN_POINT('Ctrl Pts',(33.6665286247185,-31.9985210141682,51.4214803633902));
#21075=CARTESIAN_POINT('Ctrl Pts',(33.6686262364557,-32.0004179151258,51.2285196366098));
#21076=CARTESIAN_POINT('Ctrl Pts',(33.6687027575733,-32.023143742516,51.2269932938115));
#21077=CARTESIAN_POINT('Ctrl Pts',(33.6682786564179,-32.0458666491388,51.2254669510132));
#21078=CARTESIAN_POINT('Ctrl Pts',(33.6673450516818,-32.0685686027211,51.2239406082148));
#21079=CARTESIAN_POINT('Ctrl Pts',(33.6446871232761,-32.6195290028056,51.1868973451416));
#21080=CARTESIAN_POINT('Ctrl Pts',(33.3219322677286,-33.1581480900158,51.1498540820684));
#21081=CARTESIAN_POINT('Ctrl Pts',(32.8467713568352,-33.4379566905658,51.1128108189952));
#21082=CARTESIAN_POINT('Ctrl Pts',(32.3716104459418,-33.7177652911157,51.0757675559219));
#21083=CARTESIAN_POINT('Ctrl Pts',(31.7440434797025,-33.7387634050054,51.0387242928486));
#21084=CARTESIAN_POINT('Ctrl Pts',(31.251241699047,-33.491342409186,51.0016810297754));
#21085=CARTESIAN_POINT('Ctrl Pts',(30.7584399183916,-33.2439214133666,50.9646377667021));
#21086=CARTESIAN_POINT('Ctrl Pts',(30.4004033233201,-32.7280813078381,50.9275945036289));
#21087=CARTESIAN_POINT('Ctrl Pts',(30.340967518355,-32.179867727859,50.8905512405557));
#21088=CARTESIAN_POINT('Ctrl Pts',(30.2815317133899,-31.6316541478799,50.8535079774824));
#21089=CARTESIAN_POINT('Ctrl Pts',(30.5206966985314,-31.0510670934503,50.8164647144092));
#21090=CARTESIAN_POINT('Ctrl Pts',(30.9490218734015,-30.7037800525773,50.7794214513359));
#21091=CARTESIAN_POINT('Ctrl Pts',(31.3773470482717,-30.3564930117043,50.7423781882627));
#21092=CARTESIAN_POINT('Ctrl Pts',(31.9948324128706,-30.242505984388,50.7053349251895));
#21093=CARTESIAN_POINT('Ctrl Pts',(32.5189200125302,-30.4139788162581,50.6682916621163));
#21094=CARTESIAN_POINT('Ctrl Pts',(33.0430076121899,-30.5854516481282,50.631248399043));
#21095=CARTESIAN_POINT('Ctrl Pts',(33.4736974469104,-31.0423843391848,50.5942051359697));
#21096=CARTESIAN_POINT('Ctrl Pts',(33.6139081836433,-31.5756869676153,50.5571618728965));
#21097=CARTESIAN_POINT('Ctrl Pts',(33.6500456502904,-31.7131386806355,50.5476144608009));
#21098=CARTESIAN_POINT('Ctrl Pts',(33.6668870964128,-31.8556635155748,50.5380670487053));
#21099=CARTESIAN_POINT('Ctrl Pts',(33.6656097964572,-31.9984850050081,50.5285196366098));
#21100=CARTESIAN_POINT('Origin',(32.,-32.,48.));
#21101=CARTESIAN_POINT('',(33.6634354342081,-32.000507607353,49.8285196366098));
#21102=CARTESIAN_POINT('',(33.6665861374632,-32.0014707565485,50.0214803633902));
#21103=CARTESIAN_POINT('',(33.666,-32.,48.));
#21104=CARTESIAN_POINT('Ctrl Pts',(33.6665861374632,-32.0014707565485,50.0214803633902));
#21105=CARTESIAN_POINT('Ctrl Pts',(33.6625139716522,-31.5584612743337,50.05113936803));
#21106=CARTESIAN_POINT('Ctrl Pts',(33.4805422623644,-31.1124970258842,50.0807983726698));
#21107=CARTESIAN_POINT('Ctrl Pts',(33.1642404300765,-30.8044727727622,50.1104573773096));
#21108=CARTESIAN_POINT('Ctrl Pts',(32.7691883328704,-30.4197591392497,50.1475006403828));
#21109=CARTESIAN_POINT('Ctrl Pts',(32.164590541927,-30.2502223504349,50.1845439034561));
#21110=CARTESIAN_POINT('Ctrl Pts',(31.6271077280869,-30.3734415216048,50.2215871665293));
#21111=CARTESIAN_POINT('Ctrl Pts',(31.0896249142469,-30.4966606927747,50.2586304296025));
#21112=CARTESIAN_POINT('Ctrl Pts',(30.6192570775103,-30.9126358239292,50.2956736926758));
#21113=CARTESIAN_POINT('Ctrl Pts',(30.4312419895041,-31.4310189505827,50.332716955749));
#21114=CARTESIAN_POINT('Ctrl Pts',(30.2432269014979,-31.9494020772363,50.3697602188223));
#21115=CARTESIAN_POINT('Ctrl Pts',(30.3375645622221,-32.5701931993888,50.4068034818955));
#21116=CARTESIAN_POINT('Ctrl Pts',(30.6710865696546,-33.0093216656442,50.4438467449688));
#21117=CARTESIAN_POINT('Ctrl Pts',(31.0046085770871,-33.4484501318996,50.480890008042));
#21118=CARTESIAN_POINT('Ctrl Pts',(31.5773149312279,-33.7059159422579,50.5179332711152));
#21119=CARTESIAN_POINT('Ctrl Pts',(32.1271383097918,-33.663904137947,50.5549765341885));
#21120=CARTESIAN_POINT('Ctrl Pts',(32.6769616883557,-33.621892333636,50.5920197972617));
#21121=CARTESIAN_POINT('Ctrl Pts',(33.2039020913427,-33.2804029146558,50.629063060335));
#21122=CARTESIAN_POINT('Ctrl Pts',(33.4668344475638,-32.7956995874872,50.6661063234082));
#21123=CARTESIAN_POINT('Ctrl Pts',(33.5978490648701,-32.554180354827,50.6845643367355));
#21124=CARTESIAN_POINT('Ctrl Pts',(33.6633142999988,-32.2771031787025,50.7030223500629));
#21125=CARTESIAN_POINT('Ctrl Pts',(33.6632910498763,-32.0000156711391,50.7214803633902));
#21126=CARTESIAN_POINT('Ctrl Pts',(33.6656097964572,-31.9984850050081,50.5285196366098));
#21127=CARTESIAN_POINT('Ctrl Pts',(33.6619312656801,-32.4098004851152,50.5010237856321));
#21128=CARTESIAN_POINT('Ctrl Pts',(33.5079762138442,-32.8235764117193,50.4735279346545));
#21129=CARTESIAN_POINT('Ctrl Pts',(33.231865087192,-33.1257218047281,50.4460320836768));
#21130=CARTESIAN_POINT('Ctrl Pts',(32.8598796152629,-33.5327814476059,50.4089888206036));
#21131=CARTESIAN_POINT('Ctrl Pts',(32.2661770326593,-33.737228167557,50.3719455575303));
#21132=CARTESIAN_POINT('Ctrl Pts',(31.722432421963,-33.6455082540982,50.334902294457));
#21133=CARTESIAN_POINT('Ctrl Pts',(31.1786878112666,-33.5537883406393,50.2978590313838));
#21134=CARTESIAN_POINT('Ctrl Pts',(30.6849011724773,-33.1659017937705,50.2608157683106));
#21135=CARTESIAN_POINT('Ctrl Pts',(30.4670265940585,-32.6593433941116,50.2237725052373));
#21136=CARTESIAN_POINT('Ctrl Pts',(30.2491520156396,-32.1527849944527,50.1867292421641));
#21137=CARTESIAN_POINT('Ctrl Pts',(30.3071894975912,-31.5275547420038,50.1496859790908));
#21138=CARTESIAN_POINT('Ctrl Pts',(30.6145814028672,-31.0697546101155,50.1126427160176));
#21139=CARTESIAN_POINT('Ctrl Pts',(30.9219733081434,-30.6119544782272,50.0755994529443));
#21140=CARTESIAN_POINT('Ctrl Pts',(31.4787196367441,-30.3215844668996,50.0385561898711));
#21141=CARTESIAN_POINT('Ctrl Pts',(32.0300562875329,-30.3315163188504,50.0015129267979));
#21142=CARTESIAN_POINT('Ctrl Pts',(32.5813929383217,-30.3414481708013,49.9644696637246));
#21143=CARTESIAN_POINT('Ctrl Pts',(33.1273199112987,-30.6516818860305,49.9274264006514));
#21144=CARTESIAN_POINT('Ctrl Pts',(33.4180239837953,-31.1202561986215,49.8903831375781));
#21145=CARTESIAN_POINT('Ctrl Pts',(33.5798525249692,-31.3811011767704,49.8697619705887));
#21146=CARTESIAN_POINT('Ctrl Pts',(33.6625899605592,-31.6910143728597,49.8491408035992));
#21147=CARTESIAN_POINT('Ctrl Pts',(33.6634354342081,-32.000507607353,49.8285196366098));
#21148=CARTESIAN_POINT('Origin',(32.,-32.,48.));
#21149=CARTESIAN_POINT('',(33.6674693081957,-32.0012453487566,49.1285196366098));
#21150=CARTESIAN_POINT('',(33.6680839806342,-31.999059079215,49.3214803633902));
#21151=CARTESIAN_POINT('',(33.666,-32.,48.));
#21152=CARTESIAN_POINT('Ctrl Pts',(33.6680839806342,-31.999059079215,49.3214803633902));
#21153=CARTESIAN_POINT('Ctrl Pts',(33.6684556670003,-31.9440785511347,49.3251698598506));
#21154=CARTESIAN_POINT('Ctrl Pts',(33.6659729369783,-31.8891320008961,49.328859356311));
#21155=CARTESIAN_POINT('Ctrl Pts',(33.6605253939354,-31.8344809793795,49.3325488527715));
#21156=CARTESIAN_POINT('Ctrl Pts',(33.6058310007557,-31.2857740788653,49.3695921158447));
#21157=CARTESIAN_POINT('Ctrl Pts',(33.2522671158011,-30.7668581022072,49.4066353789179));
#21158=CARTESIAN_POINT('Ctrl Pts',(32.7616226557065,-30.5151861866193,49.4436786419912));
#21159=CARTESIAN_POINT('Ctrl Pts',(32.2709781956119,-30.2635142710314,49.4807219050645));
#21160=CARTESIAN_POINT('Ctrl Pts',(31.6432531603773,-30.2790864165136,49.5177651681377));
#21161=CARTESIAN_POINT('Ctrl Pts',(31.1656911224287,-30.5547768937298,49.5548084312109));
#21162=CARTESIAN_POINT('Ctrl Pts',(30.6881290844802,-30.830467370946,49.5918516942842));
#21163=CARTESIAN_POINT('Ctrl Pts',(30.3607300438178,-31.3662761798961,49.6288949573574));
#21164=CARTESIAN_POINT('Ctrl Pts',(30.3333100262012,-31.9170201149068,49.6659382204307));
#21165=CARTESIAN_POINT('Ctrl Pts',(30.3058900085846,-32.4677640499176,49.7029814835039));
#21166=CARTESIAN_POINT('Ctrl Pts',(30.5784490140139,-33.033443110989,49.7400247465772));
#21167=CARTESIAN_POINT('Ctrl Pts',(31.0262655194942,-33.3552056270417,49.7770680096504));
#21168=CARTESIAN_POINT('Ctrl Pts',(31.4740820249745,-33.6769681430945,49.8141112727237));
#21169=CARTESIAN_POINT('Ctrl Pts',(32.097156030506,-33.7548141141286,49.8511545357969));
#21170=CARTESIAN_POINT('Ctrl Pts',(32.6103722496354,-33.5531216459011,49.8881977988701));
#21171=CARTESIAN_POINT('Ctrl Pts',(33.1235884687648,-33.3514291776736,49.9252410619434));
#21172=CARTESIAN_POINT('Ctrl Pts',(33.5269469014922,-32.8701982701844,49.9622843250166));
#21173=CARTESIAN_POINT('Ctrl Pts',(33.6358729161216,-32.3296375773346,49.9993275880899));
#21174=CARTESIAN_POINT('Ctrl Pts',(33.6575863877605,-32.2218814153821,50.0067118465233));
#21175=CARTESIAN_POINT('Ctrl Pts',(33.6675999922806,-32.1117676645154,50.0140961049568));
#21176=CARTESIAN_POINT('Ctrl Pts',(33.6665861374632,-32.0014707565485,50.0214803633902));
#21177=CARTESIAN_POINT('Ctrl Pts',(33.6634354342081,-32.000507607353,49.8285196366098));
#21178=CARTESIAN_POINT('Ctrl Pts',(33.6641087447684,-32.2469789945802,49.812097540526));
#21179=CARTESIAN_POINT('Ctrl Pts',(33.6128456395138,-32.493184039427,49.7956754444422));
#21180=CARTESIAN_POINT('Ctrl Pts',(33.508231507918,-32.7141280649899,49.7792533483584));
#21181=CARTESIAN_POINT('Ctrl Pts',(33.2722537875278,-33.2125107088145,49.7422100852852));
#21182=CARTESIAN_POINT('Ctrl Pts',(32.7648171747314,-33.5823610865111,49.7051668222119));
#21183=CARTESIAN_POINT('Ctrl Pts',(32.2181219120838,-33.6544376706759,49.6681235591386));
#21184=CARTESIAN_POINT('Ctrl Pts',(31.6714266494361,-33.7265142548407,49.6310802960654));
#21185=CARTESIAN_POINT('Ctrl Pts',(31.0854727369374,-33.5008170454736,49.5940370329922));
#21186=CARTESIAN_POINT('Ctrl Pts',(30.7283895077441,-33.0806238617888,49.556993769919));
#21187=CARTESIAN_POINT('Ctrl Pts',(30.3713062785509,-32.6604306781041,49.5199505068457));
#21188=CARTESIAN_POINT('Ctrl Pts',(30.2430937326631,-32.0457415201017,49.4829072437725));
#21189=CARTESIAN_POINT('Ctrl Pts',(30.4024212358755,-31.5178348134704,49.4458639806992));
#21190=CARTESIAN_POINT('Ctrl Pts',(30.5617487390879,-30.9899281068391,49.408820717626));
#21191=CARTESIAN_POINT('Ctrl Pts',(31.0086162914005,-30.5488038515789,49.3717774545528));
#21192=CARTESIAN_POINT('Ctrl Pts',(31.5385397239134,-30.3963181150002,49.3347341914795));
#21193=CARTESIAN_POINT('Ctrl Pts',(32.0684631564263,-30.2438323784214,49.2976909284063));
#21194=CARTESIAN_POINT('Ctrl Pts',(32.6814424691395,-30.3799851605242,49.260647665333));
#21195=CARTESIAN_POINT('Ctrl Pts',(33.0969816522974,-30.7424736864759,49.2236044022598));
#21196=CARTESIAN_POINT('Ctrl Pts',(33.4525248970599,-31.0526257778542,49.1919094803764));
#21197=CARTESIAN_POINT('Ctrl Pts',(33.6635253872144,-31.5284746399745,49.1602145584931));
#21198=CARTESIAN_POINT('Ctrl Pts',(33.6674693081957,-32.0012453487566,49.1285196366098));
#21199=CARTESIAN_POINT('Origin',(32.,-32.,48.));
#21200=CARTESIAN_POINT('',(33.6673134814248,-31.9986999266192,48.4285196366098));
#21201=CARTESIAN_POINT('',(33.6637466903966,-31.9991286486337,48.6214803633902));
#21202=CARTESIAN_POINT('',(33.666,-32.,48.));
#21203=CARTESIAN_POINT('Ctrl Pts',(33.6637466903966,-31.9991286486337,48.6214803633902));
#21204=CARTESIAN_POINT('Ctrl Pts',(33.6647970901213,-31.7776577039004,48.6362436147445));
#21205=CARTESIAN_POINT('Ctrl Pts',(33.6236994106997,-31.5565607626247,48.6510068660988));
#21206=CARTESIAN_POINT('Ctrl Pts',(33.5386159953374,-31.353933479444,48.6657701174531));
#21207=CARTESIAN_POINT('Ctrl Pts',(33.3251286501182,-30.8455105327269,48.7028133805264));
#21208=CARTESIAN_POINT('Ctrl Pts',(32.8347136636581,-30.4533698020822,48.7398566435996));
#21209=CARTESIAN_POINT('Ctrl Pts',(32.2917822745966,-30.3569527595584,48.7768999066729));
#21210=CARTESIAN_POINT('Ctrl Pts',(31.7488508855352,-30.2605357170346,48.8139431697461));
#21211=CARTESIAN_POINT('Ctrl Pts',(31.1534030938725,-30.4598423626317,48.8509864328193));
#21212=CARTESIAN_POINT('Ctrl Pts',(30.7779125803921,-30.8636710560197,48.8880296958926));
#21213=CARTESIAN_POINT('Ctrl Pts',(30.4024220669116,-31.2674997494077,48.9250729589658));
#21214=CARTESIAN_POINT('Ctrl Pts',(30.2468888316136,-31.8758504905866,48.962116222039));
#21215=CARTESIAN_POINT('Ctrl Pts',(30.3824840396265,-32.4103452790375,48.9991594851123));
#21216=CARTESIAN_POINT('Ctrl Pts',(30.5180792476393,-32.9448400674884,49.0362027481855));
#21217=CARTESIAN_POINT('Ctrl Pts',(30.9448028989631,-33.4054789032113,49.0732460112588));
#21218=CARTESIAN_POINT('Ctrl Pts',(31.4673885645646,-33.5814759526894,49.110289274332));
#21219=CARTESIAN_POINT('Ctrl Pts',(31.9899742301661,-33.7574730021676,49.1473325374053));
#21220=CARTESIAN_POINT('Ctrl Pts',(32.6084219100455,-33.648828265401,49.1843758004785));
#21221=CARTESIAN_POINT('Ctrl Pts',(33.0397332992827,-33.3052569848326,49.2214190635518));
#21222=CARTESIAN_POINT('Ctrl Pts',(33.4280862201802,-32.9959052874864,49.2547728301646));
#21223=CARTESIAN_POINT('Ctrl Pts',(33.6647238634908,-32.4960937617278,49.2881265967774));
#21224=CARTESIAN_POINT('Ctrl Pts',(33.6680839806342,-31.999059079215,49.3214803633902));
#21225=CARTESIAN_POINT('Ctrl Pts',(33.6674693081957,-32.0012453487566,49.1285196366098));
#21226=CARTESIAN_POINT('Ctrl Pts',(33.6681348228517,-32.0810227675013,49.1231712954199));
#21227=CARTESIAN_POINT('Ctrl Pts',(33.6629044681521,-32.1607125368175,49.11782295423));
#21228=CARTESIAN_POINT('Ctrl Pts',(33.6514778687695,-32.2395037027839,49.11247461304));
#21229=CARTESIAN_POINT('Ctrl Pts',(33.5723358484811,-32.7852209233395,49.0754313499668));
#21230=CARTESIAN_POINT('Ctrl Pts',(33.1959527543017,-33.2878310946498,49.0383880868936));
#21231=CARTESIAN_POINT('Ctrl Pts',(32.6945594492755,-33.5173425276136,49.0013448238203));
#21232=CARTESIAN_POINT('Ctrl Pts',(32.1931661442492,-33.7468539605773,48.9643015607471));
#21233=CARTESIAN_POINT('Ctrl Pts',(31.5667626283762,-33.7032666551944,48.9272582976738));
#21234=CARTESIAN_POINT('Ctrl Pts',(31.1019877539881,-33.4065259260658,48.8902150346006));
#21235=CARTESIAN_POINT('Ctrl Pts',(30.6372128796001,-33.1097851969372,48.8531717715273));
#21236=CARTESIAN_POINT('Ctrl Pts',(30.3340666466971,-32.5598910440628,48.8161285084541));
#21237=CARTESIAN_POINT('Ctrl Pts',(30.3312671277136,-32.0084720501211,48.7790852453809));
#21238=CARTESIAN_POINT('Ctrl Pts',(30.32846760873,-31.4570530561794,48.7420419823076));
#21239=CARTESIAN_POINT('Ctrl Pts',(30.6260148036659,-30.9041092211704,48.7049987192344));
#21240=CARTESIAN_POINT('Ctrl Pts',(31.0877527295011,-30.6026646457811,48.6679554561611));
#21241=CARTESIAN_POINT('Ctrl Pts',(31.5494906553363,-30.3012200703919,48.6309121930879));
#21242=CARTESIAN_POINT('Ctrl Pts',(32.1754193120707,-30.2512747546223,48.5938689300147));
#21243=CARTESIAN_POINT('Ctrl Pts',(32.6791171403395,-30.4756834041513,48.5568256669414));
#21244=CARTESIAN_POINT('Ctrl Pts',(33.1828149686084,-30.7000920536804,48.5197824038682));
#21245=CARTESIAN_POINT('Ctrl Pts',(33.5642819684116,-31.1988546685082,48.4827391407949));
#21246=CARTESIAN_POINT('Ctrl Pts',(33.6489609090579,-31.7437401805171,48.4456958777217));
#21247=CARTESIAN_POINT('Ctrl Pts',(33.6620489020421,-31.8279577876803,48.4399704640177));
#21248=CARTESIAN_POINT('Ctrl Pts',(33.6680469690924,-31.9132772178947,48.4342450503137));
#21249=CARTESIAN_POINT('Ctrl Pts',(33.6673134814248,-31.9986999266192,48.4285196366098));
#21250=CARTESIAN_POINT('Origin',(32.,-32.,48.));
#21251=CARTESIAN_POINT('',(33.6633884171911,-31.9995809948869,47.7285196366098));
#21252=CARTESIAN_POINT('',(33.6649068066772,-32.0014151417835,47.9214803633902));
#21253=CARTESIAN_POINT('',(33.666,-32.,48.));
#21254=CARTESIAN_POINT('Ctrl Pts',(33.6649068066772,-32.0014151417835,47.9214803633902));
#21255=CARTESIAN_POINT('Ctrl Pts',(33.6617820842682,-31.6145003896715,47.9473173696384));
#21256=CARTESIAN_POINT('Ctrl Pts',(33.5274209283347,-31.2256285879447,47.9731543758866));
#21257=CARTESIAN_POINT('Ctrl Pts',(33.2809047305485,-30.9304093300005,47.9989913821348));
#21258=CARTESIAN_POINT('Ctrl Pts',(32.927467328448,-30.5071449420422,48.036034645208));
#21259=CARTESIAN_POINT('Ctrl Pts',(32.3434864205215,-30.2763907205152,48.0730779082812));
#21260=CARTESIAN_POINT('Ctrl Pts',(31.7961885037315,-30.3437385459776,48.1101211713545));
#21261=CARTESIAN_POINT('Ctrl Pts',(31.2488905869415,-30.41108637144,48.1471644344277));
#21262=CARTESIAN_POINT('Ctrl Pts',(30.7382756612879,-30.7765362438918,48.184207697501));
#21263=CARTESIAN_POINT('Ctrl Pts',(30.4979983480558,-31.2728602832685,48.2212509605742));
#21264=CARTESIAN_POINT('Ctrl Pts',(30.2577210348237,-31.7691843226452,48.2582942236475));
#21265=CARTESIAN_POINT('Ctrl Pts',(30.2877813340129,-32.3963825289467,48.2953374867207));
#21266=CARTESIAN_POINT('Ctrl Pts',(30.5744238157098,-32.8674524038101,48.3323807497939));
#21267=CARTESIAN_POINT('Ctrl Pts',(30.8610662974067,-33.3385222786736,48.3694240128672));
#21268=CARTESIAN_POINT('Ctrl Pts',(31.4042909616111,-33.6534638220991,48.4064672759405));
#21269=CARTESIAN_POINT('Ctrl Pts',(31.9555211474962,-33.6681614915144,48.4435105390137));
#21270=CARTESIAN_POINT('Ctrl Pts',(32.5067513333814,-33.6828591609297,48.4805538020869));
#21271=CARTESIAN_POINT('Ctrl Pts',(33.0659870409472,-33.3973129563348,48.5175970651601));
#21272=CARTESIAN_POINT('Ctrl Pts',(33.377325042741,-32.9421872726427,48.5546403282334));
#21273=CARTESIAN_POINT('Ctrl Pts',(33.5645821511335,-32.6684477387846,48.5769203399523));
#21274=CARTESIAN_POINT('Ctrl Pts',(33.662161476028,-32.3333622890182,48.5992003516713));
#21275=CARTESIAN_POINT('Ctrl Pts',(33.6637466903966,-31.9991286486337,48.6214803633902));
#21276=CARTESIAN_POINT('Ctrl Pts',(33.6673134814248,-31.9986999266192,48.4285196366098));
#21277=CARTESIAN_POINT('Ctrl Pts',(33.6633013248413,-32.4659597025715,48.3972017872405));
#21278=CARTESIAN_POINT('Ctrl Pts',(33.4578770968944,-32.9363096322133,48.3658839378713));
#21279=CARTESIAN_POINT('Ctrl Pts',(33.1096935360429,-33.2463231646516,48.334566088502));
#21280=CARTESIAN_POINT('Ctrl Pts',(32.6978563408921,-33.6130122275871,48.2975228254288));
#21281=CARTESIAN_POINT('Ctrl Pts',(32.0862910691011,-33.755381944268,48.2604795623554));
#21282=CARTESIAN_POINT('Ctrl Pts',(31.5548466729667,-33.6082847043089,48.2234362992822));
#21283=CARTESIAN_POINT('Ctrl Pts',(31.0234022768324,-33.4611874643497,48.1863930362089));
#21284=CARTESIAN_POINT('Ctrl Pts',(30.5720787563548,-33.0246232677504,48.1493497731358));
#21285=CARTESIAN_POINT('Ctrl Pts',(30.4073993073046,-32.498361523704,48.1123065100625));
#21286=CARTESIAN_POINT('Ctrl Pts',(30.2427198582543,-31.9720997796577,48.0752632469893));
#21287=CARTESIAN_POINT('Ctrl Pts',(30.3646844806315,-31.3561404881642,48.038219983916));
#21288=CARTESIAN_POINT('Ctrl Pts',(30.7174828245619,-30.9323432811109,48.0011767208428));
#21289=CARTESIAN_POINT('Ctrl Pts',(31.0702811684923,-30.5085460740576,47.9641334577695));
#21290=CARTESIAN_POINT('Ctrl Pts',(31.653913233976,-30.2769109514445,47.9270901946963));
#21291=CARTESIAN_POINT('Ctrl Pts',(32.2013121524606,-30.3434328893901,47.8900469316231));
#21292=CARTESIAN_POINT('Ctrl Pts',(32.7487110709453,-30.4099548273358,47.8530036685498));
#21293=CARTESIAN_POINT('Ctrl Pts',(33.2598768424309,-30.7746338258402,47.8159604054765));
#21294=CARTESIAN_POINT('Ctrl Pts',(33.5009027815667,-31.2705947525773,47.7789171424033));
#21295=CARTESIAN_POINT('Ctrl Pts',(33.610208362449,-31.4955136861422,47.7621179738054));
#21296=CARTESIAN_POINT('Ctrl Pts',(33.6639560548541,-31.747432513297,47.7453188052076));
#21297=CARTESIAN_POINT('Ctrl Pts',(33.6633884171911,-31.9995809948869,47.7285196366098));
#21298=CARTESIAN_POINT('Origin',(32.,-32.,48.));
#21299=CARTESIAN_POINT('',(33.6657775986594,-32.0015218249574,47.0285196366098));
#21300=CARTESIAN_POINT('',(33.6687537257198,-32.0000368502801,47.2214803633902));
#21301=CARTESIAN_POINT('',(33.666,-32.,48.));
#21302=CARTESIAN_POINT('Ctrl Pts',(33.6687533332126,-32.0000368450276,47.2214803633902));
#21303=CARTESIAN_POINT('Ctrl Pts',(33.6685745432646,-31.4505822546247,47.2583911245323));
#21304=CARTESIAN_POINT('Ctrl Pts',(33.3706768056139,-30.9009615283162,47.2953018856743));
#21305=CARTESIAN_POINT('Ctrl Pts',(32.9101378018718,-30.6012897685026,47.3322126468164));
#21306=CARTESIAN_POINT('Ctrl Pts',(32.4479455591964,-30.300542249597,47.3692559098897));
#21307=CARTESIAN_POINT('Ctrl Pts',(31.8219422581151,-30.2515414474562,47.4062991729629));
#21308=CARTESIAN_POINT('Ctrl Pts',(31.318583614841,-30.4767098634442,47.4433424360361));
#21309=CARTESIAN_POINT('Ctrl Pts',(30.815224971567,-30.7018782794321,47.4803856991094));
#21310=CARTESIAN_POINT('Ctrl Pts',(30.4345109861002,-31.2012159135488,47.5174289621826));
#21311=CARTESIAN_POINT('Ctrl Pts',(30.3506543138547,-31.7462285719679,47.5544722252559));
#21312=CARTESIAN_POINT('Ctrl Pts',(30.2667976416092,-32.2912412303871,47.5915154883291));
#21313=CARTESIAN_POINT('Ctrl Pts',(30.479798282585,-32.8819289131088,47.6285587514023));
#21314=CARTESIAN_POINT('Ctrl Pts',(30.8921882984194,-33.2479961393901,47.6656020144756));
#21315=CARTESIAN_POINT('Ctrl Pts',(31.3045783142539,-33.6140633656714,47.7026452775488));
#21316=CARTESIAN_POINT('Ctrl Pts',(31.9163577049469,-33.7555101355125,47.7396885406221));
#21317=CARTESIAN_POINT('Ctrl Pts',(32.4475795385531,-33.6076111739971,47.7767318036953));
#21318=CARTESIAN_POINT('Ctrl Pts',(32.9788013721592,-33.4597122124816,47.8137750667686));
#21319=CARTESIAN_POINT('Ctrl Pts',(33.4294656486784,-33.0224675196098,47.8508183298418));
#21320=CARTESIAN_POINT('Ctrl Pts',(33.5933508388009,-32.4959578959791,47.887861592915));
#21321=CARTESIAN_POINT('Ctrl Pts',(33.6429290718713,-32.3366792154913,47.8990678497401));
#21322=CARTESIAN_POINT('Ctrl Pts',(33.6662620891541,-32.1692312594838,47.9102741065651));
#21323=CARTESIAN_POINT('Ctrl Pts',(33.6649068066772,-32.0014151417835,47.9214803633902));
#21324=CARTESIAN_POINT('Ctrl Pts',(33.6633884171911,-31.9995809948869,47.7285196366098));
#21325=CARTESIAN_POINT('Ctrl Pts',(33.6627043767632,-32.3034363704314,47.7082755421344));
#21326=CARTESIAN_POINT('Ctrl Pts',(33.5831445764217,-32.6076252460772,47.688031447659));
#21327=CARTESIAN_POINT('Ctrl Pts',(33.4268834615959,-32.8653003881351,47.6677873531836));
#21328=CARTESIAN_POINT('Ctrl Pts',(33.1409520957033,-33.3368022419862,47.6307440901104));
#21329=CARTESIAN_POINT('Ctrl Pts',(32.598203257132,-33.6525630947185,47.5937008270371));
#21330=CARTESIAN_POINT('Ctrl Pts',(32.0469958714793,-33.6680924922637,47.5566575639639));
#21331=CARTESIAN_POINT('Ctrl Pts',(31.4957884858266,-33.6836218898089,47.5196143008906));
#21332=CARTESIAN_POINT('Ctrl Pts',(30.9361225530924,-33.398919832167,47.4825710378174));
#21333=CARTESIAN_POINT('Ctrl Pts',(30.6240981694338,-32.9442644371823,47.4455277747442));
#21334=CARTESIAN_POINT('Ctrl Pts',(30.3120737857752,-32.4896090421976,47.4084845116709));
#21335=CARTESIAN_POINT('Ctrl Pts',(30.2476909511922,-31.8650003098702,47.3714412485976));
#21336=CARTESIAN_POINT('Ctrl Pts',(30.4604109016885,-31.3562558093131,47.3343979855244));
#21337=CARTESIAN_POINT('Ctrl Pts',(30.6731308521849,-30.8475113087561,47.2973547224512));
#21338=CARTESIAN_POINT('Ctrl Pts',(31.1629535877605,-30.4546310399694,47.260311459378));
#21339=CARTESIAN_POINT('Ctrl Pts',(31.7057388805693,-30.3573948836455,47.2232681963047));
#21340=CARTESIAN_POINT('Ctrl Pts',(32.2485241733781,-30.2601587273215,47.1862249332315));
#21341=CARTESIAN_POINT('Ctrl Pts',(32.8442720234201,-30.4585666834602,47.1491816701582));
#21342=CARTESIAN_POINT('Ctrl Pts',(33.2203714448242,-30.8618283471548,47.112138407085));
#21343=CARTESIAN_POINT('Ctrl Pts',(33.503364613578,-31.165259539949,47.0842654835932));
#21344=CARTESIAN_POINT('Ctrl Pts',(33.6619995116097,-31.584672681627,47.0563925601015));
#21345=CARTESIAN_POINT('Ctrl Pts',(33.6657775986594,-32.0015218249574,47.0285196366098));
#21346=CARTESIAN_POINT('Origin',(32.,-32.,48.));
#21347=CARTESIAN_POINT('',(33.6685587644994,-31.9994832045425,46.3285196366098));
#21348=CARTESIAN_POINT('',(33.6650141741342,-31.9985615245759,46.5214803633902));
#21349=CARTESIAN_POINT('',(33.666,-32.,48.));
#21350=CARTESIAN_POINT('Ctrl Pts',(33.6650141741342,-31.9985615245759,46.5214803633902));
#21351=CARTESIAN_POINT('Ctrl Pts',(33.6663655706979,-31.8347406294782,46.5324216163529));
#21352=CARTESIAN_POINT('Ctrl Pts',(33.6441442554494,-31.6712783426402,46.5433628693156));
#21353=CARTESIAN_POINT('Ctrl Pts',(33.5968493993272,-31.5154247984472,46.5543041222783));
#21354=CARTESIAN_POINT('Ctrl Pts',(33.436725526557,-30.9877591043886,46.5913473853516));
#21355=CARTESIAN_POINT('Ctrl Pts',(32.9891928793346,-30.5473096280065,46.6283906484248));
#21356=CARTESIAN_POINT('Ctrl Pts',(32.4590399703841,-30.3956236614555,46.665433911498));
#21357=CARTESIAN_POINT('Ctrl Pts',(31.9288870614335,-30.2439376949046,46.7024771745713));
#21358=CARTESIAN_POINT('Ctrl Pts',(31.3161138907549,-30.3810152381847,46.7395204376445));
#21359=CARTESIAN_POINT('Ctrl Pts',(30.9011221386267,-30.7441303507629,46.7765637007178));
#21360=CARTESIAN_POINT('Ctrl Pts',(30.4861303864983,-31.1072454633411,46.813606963791));
#21361=CARTESIAN_POINT('Ctrl Pts',(30.2689200529203,-31.6963981452175,46.8506502268642));
#21362=CARTESIAN_POINT('Ctrl Pts',(30.3488854087639,-32.2419953237128,46.8876934899375));
#21363=CARTESIAN_POINT('Ctrl Pts',(30.4288507646075,-32.7875925022081,46.9247367530107));
#21364=CARTESIAN_POINT('Ctrl Pts',(30.8059918098727,-33.2896341773223,46.961780016084));
#21365=CARTESIAN_POINT('Ctrl Pts',(31.3077308472083,-33.5183888007308,46.9988232791572));
#21366=CARTESIAN_POINT('Ctrl Pts',(31.809469884544,-33.7471434241392,47.0358665422305));
#21367=CARTESIAN_POINT('Ctrl Pts',(32.43580691395,-33.702610995842,47.0729098053037));
#21368=CARTESIAN_POINT('Ctrl Pts',(32.9001335069413,-33.4051693135608,47.109953068377));
#21369=CARTESIAN_POINT('Ctrl Pts',(33.3644600999327,-33.1077276312796,47.1469963314502));
#21370=CARTESIAN_POINT('Ctrl Pts',(33.6667762565094,-32.5573766950145,47.1840395945234));
#21371=CARTESIAN_POINT('Ctrl Pts',(33.668743742663,-32.0059541090467,47.2210828575967));
#21372=CARTESIAN_POINT('Ctrl Pts',(33.6687507802643,-32.0039816975615,47.2212153595278));
#21373=CARTESIAN_POINT('Ctrl Pts',(33.6687539750312,-32.002009272365,47.221347861459));
#21374=CARTESIAN_POINT('Ctrl Pts',(33.6687533332126,-32.0000368450276,47.2214803633902));
#21375=CARTESIAN_POINT('Ctrl Pts',(33.6657775986594,-32.0015218249574,47.0285196366098));
#21376=CARTESIAN_POINT('Ctrl Pts',(33.6670206093262,-32.1386674028061,47.0193492970283));
#21377=CARTESIAN_POINT('Ctrl Pts',(33.6515012237676,-32.2755354419662,47.0101789574468));
#21378=CARTESIAN_POINT('Ctrl Pts',(33.6181332971531,-32.4079041643904,47.0010086178652));
#21379=CARTESIAN_POINT('Ctrl Pts',(33.4833447353118,-32.9426029466809,46.963965354792));
#21380=CARTESIAN_POINT('Ctrl Pts',(33.057316618863,-33.4038851400114,46.9269220917187));
#21381=CARTESIAN_POINT('Ctrl Pts',(32.5349971038525,-33.5806705139124,46.8898788286455));
#21382=CARTESIAN_POINT('Ctrl Pts',(32.0126775888419,-33.7574558878134,46.8528355655722));
#21383=CARTESIAN_POINT('Ctrl Pts',(31.3940666752695,-33.6497444422849,46.815792302499));
#21384=CARTESIAN_POINT('Ctrl Pts',(30.962237362908,-33.3068243507597,46.7787490394258));
#21385=CARTESIAN_POINT('Ctrl Pts',(30.5304080505466,-32.9639042592346,46.7417057763525));
#21386=CARTESIAN_POINT('Ctrl Pts',(30.285360339396,-32.3857755217127,46.7046625132793));
#21387=CARTESIAN_POINT('Ctrl Pts',(30.339226733363,-31.8369867137117,46.6676192502061));
#21388=CARTESIAN_POINT('Ctrl Pts',(30.39309312733,-31.2881979057106,46.6305759871328));
#21389=CARTESIAN_POINT('Ctrl Pts',(30.7458736264145,-30.7687490272304,46.5935327240596));
#21390=CARTESIAN_POINT('Ctrl Pts',(31.236137787108,-30.5163370684692,46.5564894609863));
#21391=CARTESIAN_POINT('Ctrl Pts',(31.7264019478016,-30.2639251097081,46.5194461979131));
#21392=CARTESIAN_POINT('Ctrl Pts',(32.3541497701043,-30.278550070666,46.4824029348399));
#21393=CARTESIAN_POINT('Ctrl Pts',(32.8321272543511,-30.5535196485092,46.4453596717666));
#21394=CARTESIAN_POINT('Ctrl Pts',(33.3101047385979,-30.8284892263525,46.4083164086934));
#21395=CARTESIAN_POINT('Ctrl Pts',(33.6383118847889,-31.363803421081,46.3712731456201));
#21396=CARTESIAN_POINT('Ctrl Pts',(33.6665628824563,-31.9145053598074,46.3342298825469));
#21397=CARTESIAN_POINT('Ctrl Pts',(33.6680145197335,-31.942802394565,46.3323264672345));
#21398=CARTESIAN_POINT('Ctrl Pts',(33.6686741912351,-31.97114005715,46.3304230519221));
#21399=CARTESIAN_POINT('Ctrl Pts',(33.6685587644994,-31.9994832045425,46.3285196366098));
#21400=CARTESIAN_POINT('Origin',(32.,-32.,48.));
#21401=CARTESIAN_POINT('',(33.6642558539866,-31.9988063630671,45.6285196366098));
#21402=CARTESIAN_POINT('',(33.6636859258726,-32.0008167215673,45.8214803633902));
#21403=CARTESIAN_POINT('',(33.666,-32.,48.));
#21404=CARTESIAN_POINT('Ctrl Pts',(33.6636859258726,-32.0008167215673,45.8214803633902));
#21405=CARTESIAN_POINT('Ctrl Pts',(33.6622209390427,-31.6705283459497,45.8434953712468));
#21406=CARTESIAN_POINT('Ctrl Pts',(33.5671083318336,-31.3394623203548,45.8655103791033));
#21407=CARTESIAN_POINT('Ctrl Pts',(33.3840133726138,-31.0676652347372,45.8875253869599));
#21408=CARTESIAN_POINT('Ctrl Pts',(33.0759310505021,-30.6103294476841,45.9245686500332));
#21409=CARTESIAN_POINT('Ctrl Pts',(32.5187472242561,-30.3207998372036,45.9616119131065));
#21410=CARTESIAN_POINT('Ctrl Pts',(31.9674261915623,-30.3315635831428,45.9986551761797));
#21411=CARTESIAN_POINT('Ctrl Pts',(31.4161051588685,-30.3423273290819,46.035698439253));
#21412=CARTESIAN_POINT('Ctrl Pts',(30.8706469197269,-30.6533844314407,46.0727417023262));
#21413=CARTESIAN_POINT('Ctrl Pts',(30.5806502067447,-31.1223968468165,46.1097849653994));
#21414=CARTESIAN_POINT('Ctrl Pts',(30.2906534937624,-31.5914092621924,46.1468282284726));
#21415=CARTESIAN_POINT('Ctrl Pts',(30.2561183069395,-32.2183769905854,46.1838714915459));
#21416=CARTESIAN_POINT('Ctrl Pts',(30.4928477605068,-32.7164029990739,46.2209147546191));
#21417=CARTESIAN_POINT('Ctrl Pts',(30.7295772140741,-33.2144290075624,46.2579580176924));
#21418=CARTESIAN_POINT('Ctrl Pts',(31.2375713080316,-33.5835132961463,46.2950012807656));
#21419=CARTESIAN_POINT('Ctrl Pts',(31.7843746994676,-33.6547648956458,46.3320445438389));
#21420=CARTESIAN_POINT('Ctrl Pts',(32.3311780909037,-33.7260164951454,46.3690878069121));
#21421=CARTESIAN_POINT('Ctrl Pts',(32.9167907798183,-33.4994354055607,46.4061310699853));
#21422=CARTESIAN_POINT('Ctrl Pts',(33.2732395751167,-33.0787039049007,46.4431743330586));
#21423=CARTESIAN_POINT('Ctrl Pts',(33.5244061648518,-32.7822414182582,46.4692763431691));
#21424=CARTESIAN_POINT('Ctrl Pts',(33.6617902136893,-32.3893809923948,46.4953783532797));
#21425=CARTESIAN_POINT('Ctrl Pts',(33.6650141741342,-31.9985615245759,46.5214803633902));
#21426=CARTESIAN_POINT('Ctrl Pts',(33.6685587644994,-31.9994832045425,46.3285196366098));
#21427=CARTESIAN_POINT('Ctrl Pts',(33.6664278170942,-32.5227394156102,46.2933797888489));
#21428=CARTESIAN_POINT('Ctrl Pts',(33.4001232888826,-33.0478649913129,46.258239941088));
#21429=CARTESIAN_POINT('Ctrl Pts',(32.9757782336594,-33.353734838659,46.2231000933271));
#21430=CARTESIAN_POINT('Ctrl Pts',(32.5284477380514,-33.67617269606,46.1860568302539));
#21431=CARTESIAN_POINT('Ctrl Pts',(31.9054918976918,-33.7549587281378,46.1490135671807));
#21432=CARTESIAN_POINT('Ctrl Pts',(31.3919719272917,-33.5540408738129,46.1119703041074));
#21433=CARTESIAN_POINT('Ctrl Pts',(30.8784519568916,-33.3531230194881,46.0749270410342));
#21434=CARTESIAN_POINT('Ctrl Pts',(30.4743678564511,-32.8725012787608,46.037883777961));
#21435=CARTESIAN_POINT('Ctrl Pts',(30.3646263192768,-32.3321055541248,46.0008405148877));
#21436=CARTESIAN_POINT('Ctrl Pts',(30.2548847821026,-31.7917098294888,45.9637972518145));
#21437=CARTESIAN_POINT('Ctrl Pts',(30.4394858081946,-31.1915401209442,45.9267539887412));
#21438=CARTESIAN_POINT('Ctrl Pts',(30.8339569689707,-30.8062308328363,45.889710725668));
#21439=CARTESIAN_POINT('Ctrl Pts',(31.2284281297467,-30.4209215447285,45.8526674625947));
#21440=CARTESIAN_POINT('Ctrl Pts',(31.8327694252067,-30.2504726770573,45.8156241995215));
#21441=CARTESIAN_POINT('Ctrl Pts',(32.3704375554525,-30.3728807074486,45.7785809364483));
#21442=CARTESIAN_POINT('Ctrl Pts',(32.9081056856982,-30.4952887378399,45.741537673375));
#21443=CARTESIAN_POINT('Ctrl Pts',(33.3791006507296,-30.9105536662937,45.7044944103018));
#21444=CARTESIAN_POINT('Ctrl Pts',(33.5678977084122,-31.4286525132299,45.6674511472285));
#21445=CARTESIAN_POINT('Ctrl Pts',(33.6340379819389,-31.6101553389139,45.6544739770223));
#21446=CARTESIAN_POINT('Ctrl Pts',(33.6655448403235,-31.8042787039313,45.641496806816));
#21447=CARTESIAN_POINT('Ctrl Pts',(33.6642558539866,-31.9988063630671,45.6285196366098));
#21448=CARTESIAN_POINT('Origin',(32.,-32.,48.));
#21449=CARTESIAN_POINT('',(33.6642508521176,-32.0011912824064,44.9285196366098));
#21450=CARTESIAN_POINT('',(33.6679951137542,-32.0009960538572,45.1214803633902));
#21451=CARTESIAN_POINT('',(33.666,-32.,48.));
#21452=CARTESIAN_POINT('Ctrl Pts',(33.6679951137542,-32.0009960538572,45.1214803633902));
#21453=CARTESIAN_POINT('Ctrl Pts',(33.6645083963353,-31.507841323258,45.1545691261407));
#21454=CARTESIAN_POINT('Ctrl Pts',(33.432088645058,-31.0118309857062,45.1876578888911));
#21455=CARTESIAN_POINT('Ctrl Pts',(33.0490210707781,-30.702195730029,45.2207466516416));
#21456=CARTESIAN_POINT('Ctrl Pts',(32.6201723696075,-30.3555553820867,45.2577899147148));
#21457=CARTESIAN_POINT('Ctrl Pts',(32.0025157192002,-30.2425002018306,45.2948331777881));
#21458=CARTESIAN_POINT('Ctrl Pts',(31.4786874536787,-30.4147636267296,45.3318764408613));
#21459=CARTESIAN_POINT('Ctrl Pts',(30.9548591881572,-30.5870270516286,45.3689197039346));
#21460=CARTESIAN_POINT('Ctrl Pts',(30.5248593075215,-31.0446090816829,45.4059629670078));
#21461=CARTESIAN_POINT('Ctrl Pts',(30.3854534255734,-31.5781226610747,45.443006230081));
#21462=CARTESIAN_POINT('Ctrl Pts',(30.2460475436252,-32.1116362404665,45.4800494931543));
#21463=CARTESIAN_POINT('Ctrl Pts',(30.3972356603645,-32.7210813691959,45.5170927562276));
#21464=CARTESIAN_POINT('Ctrl Pts',(30.7698349133548,-33.127579260935,45.5541360193008));
#21465=CARTESIAN_POINT('Ctrl Pts',(31.1424341663451,-33.534077152674,45.591179282374));
#21466=CARTESIAN_POINT('Ctrl Pts',(31.7364445555863,-33.7376278074227,45.6282225454472));
#21467=CARTESIAN_POINT('Ctrl Pts',(32.280050147849,-33.6450875492755,45.6652658085205));
#21468=CARTESIAN_POINT('Ctrl Pts',(32.8236557401117,-33.5525472911282,45.7023090715937));
#21469=CARTESIAN_POINT('Ctrl Pts',(33.3168565353959,-33.1639161200851,45.739352334667));
#21470=CARTESIAN_POINT('Ctrl Pts',(33.5339665240493,-32.6570295527506,45.7763955977403));
#21471=CARTESIAN_POINT('Ctrl Pts',(33.6220468941052,-32.4513883627525,45.7914238529569));
#21472=CARTESIAN_POINT('Ctrl Pts',(33.6646859798409,-32.2262837319,45.8064521081736));
#21473=CARTESIAN_POINT('Ctrl Pts',(33.6636859258726,-32.0008167215673,45.8214803633902));
#21474=CARTESIAN_POINT('Ctrl Pts',(33.6642558539866,-31.9988063630671,45.6285196366098));
#21475=CARTESIAN_POINT('Ctrl Pts',(33.6618654357062,-32.3595568684207,45.6044535437428));
#21476=CARTESIAN_POINT('Ctrl Pts',(33.5466851733263,-32.7216978020734,45.5803874508758));
#21477=CARTESIAN_POINT('Ctrl Pts',(33.3304348817757,-33.0073153428977,45.5563213580088));
#21478=CARTESIAN_POINT('Ctrl Pts',(32.9975758471228,-33.4469465602108,45.5192780949355));
#21479=CARTESIAN_POINT('Ctrl Pts',(32.4252586274834,-33.7052762294185,45.4822348318623));
#21480=CARTESIAN_POINT('Ctrl Pts',(31.8753724793036,-33.6640940946256,45.4451915687891));
#21481=CARTESIAN_POINT('Ctrl Pts',(31.3254863311237,-33.6229119598326,45.4081483057158));
#21482=CARTESIAN_POINT('Ctrl Pts',(30.7980312544034,-33.2822180210392,45.3711050426426));
#21483=CARTESIAN_POINT('Ctrl Pts',(30.5343678322437,-32.7979119773011,45.3340617795693));
#21484=CARTESIAN_POINT('Ctrl Pts',(30.270704410084,-32.313605933563,45.2970185164961));
#21485=CARTESIAN_POINT('Ctrl Pts',(30.270832642485,-31.6856877848803,45.2599752534229));
#21486=CARTESIAN_POINT('Ctrl Pts',(30.5346938509953,-31.2014894713457,45.2229319903496));
#21487=CARTESIAN_POINT('Ctrl Pts',(30.7985550595056,-30.7172911578112,45.1858887272764));
#21488=CARTESIAN_POINT('Ctrl Pts',(31.3261492441253,-30.3768126794248,45.1488454642031));
#21489=CARTESIAN_POINT('Ctrl Pts',(31.8760521667326,-30.3358551417286,45.1118022011299));
#21490=CARTESIAN_POINT('Ctrl Pts',(32.4259550893399,-30.2948976040324,45.0747589380566));
#21491=CARTESIAN_POINT('Ctrl Pts',(32.9981667499349,-30.5534610070264,45.0377156749834));
#21492=CARTESIAN_POINT('Ctrl Pts',(33.3308461953179,-30.9932281395021,45.0006724119102));
#21493=CARTESIAN_POINT('Ctrl Pts',(33.5468435929401,-31.2787539136153,44.97662148681));
#21494=CARTESIAN_POINT('Ctrl Pts',(33.6618671138013,-31.6406654174441,44.9525705617099));
#21495=CARTESIAN_POINT('Ctrl Pts',(33.6642508521176,-32.0011912824064,44.9285196366098));
#21496=CARTESIAN_POINT('Origin',(32.,-32.,48.));
#21497=CARTESIAN_POINT('',(33.6685557839381,-32.0005207187555,44.2285196366098));
#21498=CARTESIAN_POINT('',(33.666705446585,-31.9985486374404,44.4214803633902));
#21499=CARTESIAN_POINT('',(33.666,-32.,48.));
#21500=CARTESIAN_POINT('Ctrl Pts',(33.666705446585,-31.9985486374404,44.4214803633902));
#21501=CARTESIAN_POINT('Ctrl Pts',(33.6676776984237,-31.8922296343042,44.4285996179613));
#21502=CARTESIAN_POINT('Ctrl Pts',(33.6583758869896,-31.7860801019361,44.4357188725324));
#21503=CARTESIAN_POINT('Ctrl Pts',(33.638183541047,-31.6820443176578,44.4428381271035));
#21504=CARTESIAN_POINT('Ctrl Pts',(33.5331177121255,-31.1407200978874,44.4798813901768));
#21505=CARTESIAN_POINT('Ctrl Pts',(33.1332035875173,-30.6566230988116,44.51692465325));
#21506=CARTESIAN_POINT('Ctrl Pts',(32.6214397021988,-30.4512734823014,44.5539679163232));
#21507=CARTESIAN_POINT('Ctrl Pts',(32.1096758168802,-30.2459238657912,44.5910111793965));
#21508=CARTESIAN_POINT('Ctrl Pts',(31.4860621708514,-30.3193216318466,44.6280544424697));
#21509=CARTESIAN_POINT('Ctrl Pts',(31.035960987131,-30.6378803607033,44.665097705543));
#21510=CARTESIAN_POINT('Ctrl Pts',(30.5858598034106,-30.9564390895599,44.7021409686162));
#21511=CARTESIAN_POINT('Ctrl Pts',(30.3092710819986,-31.5201587812177,44.7391842316894));
#21512=CARTESIAN_POINT('Ctrl Pts',(30.3327603220732,-32.071084361417,44.7762274947627));
#21513=CARTESIAN_POINT('Ctrl Pts',(30.3562495621479,-32.6220099416162,44.8132707578359));
#21514=CARTESIAN_POINT('Ctrl Pts',(30.6798167637091,-33.160141410357,44.8503140209092));
#21515=CARTESIAN_POINT('Ctrl Pts',(31.1553993297926,-33.4392327254398,44.8873572839824));
#21516=CARTESIAN_POINT('Ctrl Pts',(31.6309818958761,-33.7183240405225,44.9244005470557));
#21517=CARTESIAN_POINT('Ctrl Pts',(32.258579826482,-33.7383752019473,44.9614438101289));
#21518=CARTESIAN_POINT('Ctrl Pts',(32.7510077115729,-33.490210906969,44.9984870732021));
#21519=CARTESIAN_POINT('Ctrl Pts',(33.2434355966639,-33.2420466119907,45.0355303362754));
#21520=CARTESIAN_POINT('Ctrl Pts',(33.60069343624,-32.7256668606095,45.0725735993487));
#21521=CARTESIAN_POINT('Ctrl Pts',(33.6593019800612,-32.1773642271046,45.1096168624219));
#21522=CARTESIAN_POINT('Ctrl Pts',(33.6655586509436,-32.1188309673081,45.1135713627447));
#21523=CARTESIAN_POINT('Ctrl Pts',(33.6684118179163,-32.0599339040282,45.1175258630675));
#21524=CARTESIAN_POINT('Ctrl Pts',(33.6679951137542,-32.0009960538572,45.1214803633902));
#21525=CARTESIAN_POINT('Ctrl Pts',(33.6642508521176,-32.0011912824064,44.9285196366098));
#21526=CARTESIAN_POINT('Ctrl Pts',(33.6655385503544,-32.1959477778902,44.9155272986366));
#21527=CARTESIAN_POINT('Ctrl Pts',(33.6339560104401,-32.3902999199697,44.9025349606635));
#21528=CARTESIAN_POINT('Ctrl Pts',(33.5676642183743,-32.5719878260169,44.8895426226904));
#21529=CARTESIAN_POINT('Ctrl Pts',(33.3786555658768,-33.0900095180987,44.8524993596172));
#21530=CARTESIAN_POINT('Ctrl Pts',(32.9074910307108,-33.505082040305,44.815456096544));
#21531=CARTESIAN_POINT('Ctrl Pts',(32.3697729493851,-33.6272704571109,44.7784128334707));
#21532=CARTESIAN_POINT('Ctrl Pts',(31.8320548680593,-33.7494588739168,44.7413695703975));
#21533=CARTESIAN_POINT('Ctrl Pts',(31.2277832405737,-33.5787631853222,44.7043263073242));
#21534=CARTESIAN_POINT('Ctrl Pts',(30.8334694871393,-33.1932928128699,44.667283044251));
#21535=CARTESIAN_POINT('Ctrl Pts',(30.4391557337048,-32.8078224404177,44.6302397811777));
#21536=CARTESIAN_POINT('Ctrl Pts',(30.2547998543215,-32.2075773841077,44.5931965181045));
#21537=CARTESIAN_POINT('Ctrl Pts',(30.364762099767,-31.6672265270128,44.5561532550313));
#21538=CARTESIAN_POINT('Ctrl Pts',(30.4747243452125,-31.1268756699178,44.519109991958));
#21539=CARTESIAN_POINT('Ctrl Pts',(30.8790047154868,-30.646419012038,44.4820667288848));
#21540=CARTESIAN_POINT('Ctrl Pts',(31.3926067052714,-30.4457109148541,44.4450234658115));
#21541=CARTESIAN_POINT('Ctrl Pts',(31.906208695056,-30.2450028176701,44.4079802027383));
#21542=CARTESIAN_POINT('Ctrl Pts',(32.5291323043508,-30.324043281182,44.370936939665));
#21543=CARTESIAN_POINT('Ctrl Pts',(32.9763310672053,-30.6466638178604,44.3338936765918));
#21544=CARTESIAN_POINT('Ctrl Pts',(33.4003680481787,-30.9525748572825,44.2987689965978));
#21545=CARTESIAN_POINT('Ctrl Pts',(33.6664114443341,-31.4774878746799,44.2636443166038));
#21546=CARTESIAN_POINT('Ctrl Pts',(33.6685557839381,-32.0005207187555,44.2285196366098));
#21547=CARTESIAN_POINT('Origin',(32.,-32.,48.));
#21548=CARTESIAN_POINT('',(33.6657843894837,-31.9984780271603,43.5285196366098));
#21549=CARTESIAN_POINT('',(33.6632944811816,-31.9999190856909,43.7214803633902));
#21550=CARTESIAN_POINT('',(33.666,-32.,48.));
#21551=CARTESIAN_POINT('Ctrl Pts',(33.6632944811816,-31.9999190856909,43.7214803633902));
#21552=CARTESIAN_POINT('Ctrl Pts',(33.6634128178791,-31.7268111612894,43.7396733728552));
#21553=CARTESIAN_POINT('Ctrl Pts',(33.5999067829313,-31.4537550667933,43.7578663823202));
#21554=CARTESIAN_POINT('Ctrl Pts',(33.4724751700925,-31.2147879244965,43.7760593917851));
#21555=CARTESIAN_POINT('Ctrl Pts',(33.2130083255708,-30.7282206671663,43.8131026548584));
#21556=CARTESIAN_POINT('Ctrl Pts',(32.6885181894386,-30.3829797242392,43.8501459179316));
#21557=CARTESIAN_POINT('Ctrl Pts',(32.1390086040352,-30.3370454792411,43.8871891810049));
#21558=CARTESIAN_POINT('Ctrl Pts',(31.5894990186317,-30.291111234243,43.9242324440781));
#21559=CARTESIAN_POINT('Ctrl Pts',(31.0149699839572,-30.5444836871738,43.9612757071514));
#21560=CARTESIAN_POINT('Ctrl Pts',(30.6783228710374,-30.9812209774104,43.9983189702246));
#21561=CARTESIAN_POINT('Ctrl Pts',(30.3416757581177,-31.417958267647,44.0353622332978));
#21562=CARTESIAN_POINT('Ctrl Pts',(30.2429105669527,-32.0380603951895,44.0724054963711));
#21563=CARTESIAN_POINT('Ctrl Pts',(30.4272217134811,-32.5577719888467,44.1094487594443));
#21564=CARTESIAN_POINT('Ctrl Pts',(30.6115328600096,-33.0774835825039,44.1464920225176));
#21565=CARTESIAN_POINT('Ctrl Pts',(31.0789203442315,-33.4968046422757,44.1835352855908));
#21566=CARTESIAN_POINT('Ctrl Pts',(31.6155101876733,-33.6238561248802,44.2205785486641));
#21567=CARTESIAN_POINT('Ctrl Pts',(32.1521000311151,-33.7509076074846,44.2576218117373));
#21568=CARTESIAN_POINT('Ctrl Pts',(32.7578922337768,-33.5856895129216,44.2946650748105));
#21569=CARTESIAN_POINT('Ctrl Pts',(33.1556795684902,-33.2038047454075,44.3317083378838));
#21570=CARTESIAN_POINT('Ctrl Pts',(33.4770171235125,-32.8953134818994,44.3616323463859));
#21571=CARTESIAN_POINT('Ctrl Pts',(33.6626188288084,-32.4454340131511,44.3915563548881));
#21572=CARTESIAN_POINT('Ctrl Pts',(33.666705446585,-31.9985486374404,44.4214803633902));
#21573=CARTESIAN_POINT('Ctrl Pts',(33.6685557839381,-32.0005207187555,44.2285196366098));
#21574=CARTESIAN_POINT('Ctrl Pts',(33.6686729122274,-32.0290898605868,44.2266010535306));
#21575=CARTESIAN_POINT('Ctrl Pts',(33.6680026787812,-32.0576533927864,44.2246824704513));
#21576=CARTESIAN_POINT('Ctrl Pts',(33.6665278243027,-32.0861753184357,44.2227638873721));
#21577=CARTESIAN_POINT('Ctrl Pts',(33.6380519021311,-32.6368656724877,44.1857206242988));
#21578=CARTESIAN_POINT('Ctrl Pts',(33.3096261413737,-33.1720457707468,44.1486773612256));
#21579=CARTESIAN_POINT('Ctrl Pts',(32.8315363893394,-33.4468201021218,44.1116340981523));
#21580=CARTESIAN_POINT('Ctrl Pts',(32.3534466373052,-33.7215944334968,44.0745908350791));
#21581=CARTESIAN_POINT('Ctrl Pts',(31.725692893994,-33.7359629979876,44.0375475720059));
#21582=CARTESIAN_POINT('Ctrl Pts',(31.2355318684904,-33.4833508184354,44.0005043089326));
#21583=CARTESIAN_POINT('Ctrl Pts',(30.7453708429867,-33.2307386388832,43.9634610458594));
#21584=CARTESIAN_POINT('Ctrl Pts',(30.3928025352905,-32.711145715288,43.9264177827861));
#21585=CARTESIAN_POINT('Ctrl Pts',(30.3391602912853,-32.1623349520288,43.8893745197129));
#21586=CARTESIAN_POINT('Ctrl Pts',(30.2855180472801,-31.6135241887696,43.8523312566396));
#21587=CARTESIAN_POINT('Ctrl Pts',(30.5308018669659,-31.0354955858464,43.8152879935664));
#21588=CARTESIAN_POINT('Ctrl Pts',(30.9627712044431,-30.6927518978913,43.7782447304932));
#21589=CARTESIAN_POINT('Ctrl Pts',(31.3947405419203,-30.3500082099362,43.7412014674199));
#21590=CARTESIAN_POINT('Ctrl Pts',(32.0133953971889,-30.2425494369492,43.7041582043467));
#21591=CARTESIAN_POINT('Ctrl Pts',(32.5356426630091,-30.4195481304534,43.6671149412734));
#21592=CARTESIAN_POINT('Ctrl Pts',(33.0578899288294,-30.5965468239577,43.6300716782002));
#21593=CARTESIAN_POINT('Ctrl Pts',(33.4837296052012,-31.0580029839533,43.593028415127));
#21594=CARTESIAN_POINT('Ctrl Pts',(33.618299765207,-31.5927567744109,43.5559851520537));
#21595=CARTESIAN_POINT('Ctrl Pts',(33.651558523582,-31.7249201537679,43.5468299802391));
#21596=CARTESIAN_POINT('Ctrl Pts',(33.667025905015,-31.861560712161,43.5376748084244));
#21597=CARTESIAN_POINT('Ctrl Pts',(33.6657843894837,-31.9984780271603,43.5285196366098));
#21598=CARTESIAN_POINT('Origin',(32.,-32.,48.));
#21599=CARTESIAN_POINT('',(33.6633867149896,-32.0004154269497,42.8285196366098));
#21600=CARTESIAN_POINT('',(33.6664085055627,-32.0014938638813,43.0214803633902));
#21601=CARTESIAN_POINT('',(33.666,-32.,48.));
#21602=CARTESIAN_POINT('Ctrl Pts',(33.6664085055627,-32.0014938638813,43.0214803633902));
#21603=CARTESIAN_POINT('Ctrl Pts',(33.6623727377844,-31.5642233612903,43.050747127749));
#21604=CARTESIAN_POINT('Ctrl Pts',(33.4856936746432,-31.1240664805265,43.0800138921079));
#21605=CARTESIAN_POINT('Ctrl Pts',(33.1768026773126,-30.816836196291,43.1092806564668));
#21606=CARTESIAN_POINT('Ctrl Pts',(32.7858359706835,-30.4279714723517,43.1463239195401));
#21607=CARTESIAN_POINT('Ctrl Pts',(32.183062556742,-30.2520583620278,43.1833671826133));
#21608=CARTESIAN_POINT('Ctrl Pts',(31.6443082797766,-30.3695937527617,43.2204104456865));
#21609=CARTESIAN_POINT('Ctrl Pts',(31.1055540028112,-30.4871291434957,43.2574537087597));
#21610=CARTESIAN_POINT('Ctrl Pts',(30.6308188628218,-30.8981130352873,43.294496971833));
#21611=CARTESIAN_POINT('Ctrl Pts',(30.4373390864957,-31.4144814267063,43.3315402349062));
#21612=CARTESIAN_POINT('Ctrl Pts',(30.2438593101695,-31.9308498181252,43.3685834979795));
#21613=CARTESIAN_POINT('Ctrl Pts',(30.3316348975066,-32.5526027091714,43.4056267610527));
#21614=CARTESIAN_POINT('Ctrl Pts',(30.6605002152946,-32.995229348729,43.442670024126));
#21615=CARTESIAN_POINT('Ctrl Pts',(30.9893655330827,-33.4378559882867,43.4797132871992));
#21616=CARTESIAN_POINT('Ctrl Pts',(31.5593205813218,-33.7013563763557,43.5167565502724));
#21617=CARTESIAN_POINT('Ctrl Pts',(32.1095570205873,-33.6651541638684,43.5537998133457));
#21618=CARTESIAN_POINT('Ctrl Pts',(32.6597934598528,-33.628951951381,43.5908430764189));
#21619=CARTESIAN_POINT('Ctrl Pts',(33.1903112901447,-33.2930471383373,43.6278863394922));
#21620=CARTESIAN_POINT('Ctrl Pts',(33.4583484288351,-32.8111479459487,43.6649296025654));
#21621=CARTESIAN_POINT('Ctrl Pts',(33.5947448372928,-32.5659232752123,43.6837798561737));
#21622=CARTESIAN_POINT('Ctrl Pts',(33.6631718694299,-32.2828933592601,43.7026301097819));
#21623=CARTESIAN_POINT('Ctrl Pts',(33.6632944811816,-31.9999190856909,43.7214803633902));
#21624=CARTESIAN_POINT('Ctrl Pts',(33.6657843894837,-31.9984780271603,43.5285196366098));
#21625=CARTESIAN_POINT('Ctrl Pts',(33.6620025381831,-32.4155496728804,43.5006315453512));
#21626=CARTESIAN_POINT('Ctrl Pts',(33.503177614974,-32.8351893633072,43.4727434540926));
#21627=CARTESIAN_POINT('Ctrl Pts',(33.2199064719879,-33.1386700027057,43.444855362834));
#21628=CARTESIAN_POINT('Ctrl Pts',(32.8436423751234,-33.5417780196234,43.4078120997608));
#21629=CARTESIAN_POINT('Ctrl Pts',(32.2478135377548,-33.7399426325393,43.3707688366875));
#21630=CARTESIAN_POINT('Ctrl Pts',(31.7050680049991,-33.6424847916052,43.3337255736143));
#21631=CARTESIAN_POINT('Ctrl Pts',(31.1623224722433,-33.545026950671,43.296682310541));
#21632=CARTESIAN_POINT('Ctrl Pts',(30.6726602441004,-33.1519466558869,43.2596390474678));
#21633=CARTESIAN_POINT('Ctrl Pts',(30.4601481013144,-32.6431153137696,43.2225957843945));
#21634=CARTESIAN_POINT('Ctrl Pts',(30.2476359585285,-32.1342839716523,43.1855525213213));
#21635=CARTESIAN_POINT('Ctrl Pts',(30.3122739010995,-31.5097015822019,43.1485092582481));
#21636=CARTESIAN_POINT('Ctrl Pts',(30.6244839565387,-31.0551736700466,43.1114659951748));
#21637=CARTESIAN_POINT('Ctrl Pts',(30.9366940119779,-30.6006457578913,43.0744227321016));
#21638=CARTESIAN_POINT('Ctrl Pts',(31.4964761802852,-30.3161723230313,43.0373794690283));
#21639=CARTESIAN_POINT('Ctrl Pts',(32.0476771774324,-30.331926847221,43.0003362059551));
#21640=CARTESIAN_POINT('Ctrl Pts',(32.5988781745796,-30.3476813714108,42.9632929428818));
#21641=CARTESIAN_POINT('Ctrl Pts',(33.1414980005666,-30.6636638546505,42.9262496798086));
#21642=CARTESIAN_POINT('Ctrl Pts',(33.4272367634802,-31.1352824646434,42.8892064167354));
#21643=CARTESIAN_POINT('Ctrl Pts',(33.583275622188,-31.3928283044107,42.8689774900268));
#21644=CARTESIAN_POINT('Ctrl Pts',(33.6627090958471,-31.696786928658,42.8487485633183));
#21645=CARTESIAN_POINT('Ctrl Pts',(33.6633867149896,-32.0004154269497,42.8285196366098));
#21646=CARTESIAN_POINT('Origin',(32.,-32.,48.));
#21647=CARTESIAN_POINT('',(33.6673070425528,-32.0013037875835,42.1285196366098));
#21648=CARTESIAN_POINT('',(33.6682077276635,-31.9991447210259,42.3214803633902));
#21649=CARTESIAN_POINT('',(33.666,-32.,48.));
#21650=CARTESIAN_POINT('Ctrl Pts',(33.6682077276635,-31.9991447210259,42.3214803633902));
#21651=CARTESIAN_POINT('Ctrl Pts',(33.6685152776142,-31.9500189184328,42.3247776195697));
#21652=CARTESIAN_POINT('Ctrl Pts',(33.6665333026985,-31.9009182818708,42.3280748757492));
#21653=CARTESIAN_POINT('Ctrl Pts',(33.662181037674,-31.8520286556063,42.3313721319287));
#21654=CARTESIAN_POINT('Ctrl Pts',(33.6132852014122,-31.3027746126452,42.3684153950019));
#21655=CARTESIAN_POINT('Ctrl Pts',(33.2652217397612,-30.7801533642977,42.4054586580752));
#21656=CARTESIAN_POINT('Ctrl Pts',(32.7772627875611,-30.5233133209011,42.4425019211484));
#21657=CARTESIAN_POINT('Ctrl Pts',(32.2893038353611,-30.2664732775045,42.4795451842217));
#21658=CARTESIAN_POINT('Ctrl Pts',(31.6614493926119,-30.2754144390588,42.5165884472949));
#21659=CARTESIAN_POINT('Ctrl Pts',(31.1810021559353,-30.5460454993071,42.5536317103682));
#21660=CARTESIAN_POINT('Ctrl Pts',(30.7005549192587,-30.8166765595554,42.5906749734414));
#21661=CARTESIAN_POINT('Ctrl Pts',(30.3675148886547,-31.3489975184977,42.6277182365146));
#21662=CARTESIAN_POINT('Ctrl Pts',(30.3342794227585,-31.8994211306946,42.6647614995879));
#21663=CARTESIAN_POINT('Ctrl Pts',(30.3010439568623,-32.4498447428914,42.7018047626611));
#21664=CARTESIAN_POINT('Ctrl Pts',(30.5676130556739,-33.018371008343,42.7388480257344));
#21665=CARTESIAN_POINT('Ctrl Pts',(31.0120061215156,-33.3448454215074,42.7758912888076));
#21666=CARTESIAN_POINT('Ctrl Pts',(31.4563991873573,-33.6713198346718,42.8129345518809));
#21667=CARTESIAN_POINT('Ctrl Pts',(32.078616220229,-33.7557423955491,42.8499778149541));
#21668=CARTESIAN_POINT('Ctrl Pts',(32.5939340915773,-33.5594817824733,42.8870210780274));
#21669=CARTESIAN_POINT('Ctrl Pts',(33.1092519629256,-33.3632211693975,42.9240643411006));
#21670=CARTESIAN_POINT('Ctrl Pts',(33.5176706727504,-32.8862773823686,42.9611076041738));
#21671=CARTESIAN_POINT('Ctrl Pts',(33.6323000280045,-32.3468973200768,42.998150867247));
#21672=CARTESIAN_POINT('Ctrl Pts',(33.656364188659,-32.2336651689923,43.0059273659614));
#21673=CARTESIAN_POINT('Ctrl Pts',(33.6674808531087,-32.1176814088911,43.0137038646758));
#21674=CARTESIAN_POINT('Ctrl Pts',(33.6664085055627,-32.0014938638813,43.0214803633902));
#21675=CARTESIAN_POINT('Ctrl Pts',(33.6633867149896,-32.0004154269497,42.8285196366098));
#21676=CARTESIAN_POINT('Ctrl Pts',(33.6639499537789,-32.2527922225036,42.8117053002451));
#21677=CARTESIAN_POINT('Ctrl Pts',(33.6101009496347,-32.5049409347766,42.7948909638803));
#21678=CARTESIAN_POINT('Ctrl Pts',(33.500604739542,-32.7300182319024,42.7780766275156));
#21679=CARTESIAN_POINT('Ctrl Pts',(33.2593762528503,-33.2258806524225,42.7410333644424));
#21680=CARTESIAN_POINT('Ctrl Pts',(32.7480615796269,-33.5903507567164,42.7039901013691));
#21681=CARTESIAN_POINT('Ctrl Pts',(32.2006355348935,-33.6566491529375,42.6669468382959));
#21682=CARTESIAN_POINT('Ctrl Pts',(31.6532094901602,-33.7229475491586,42.6299035752227));
#21683=CARTESIAN_POINT('Ctrl Pts',(31.069672073917,-33.4910742373069,42.5928603121494));
#21684=CARTESIAN_POINT('Ctrl Pts',(30.7170468575088,-33.0671328874538,42.5558170490762));
#21685=CARTESIAN_POINT('Ctrl Pts',(30.3644216411006,-32.6431915376008,42.5187737860029));
#21686=CARTESIAN_POINT('Ctrl Pts',(30.2427086245275,-32.0271821497465,42.4817305229297));
#21687=CARTESIAN_POINT('Ctrl Pts',(30.4076029969488,-31.5009878737835,42.4446872598565));
#21688=CARTESIAN_POINT('Ctrl Pts',(30.5724973693701,-30.9747935978205,42.4076439967832));
#21689=CARTESIAN_POINT('Ctrl Pts',(31.0239991307858,-30.5384144337488,42.3706007337099));
#21690=CARTESIAN_POINT('Ctrl Pts',(31.5555035773089,-30.3915339446307,42.3335574706367));
#21691=CARTESIAN_POINT('Ctrl Pts',(32.087008023832,-30.2446534555125,42.2965142075635));
#21692=CARTESIAN_POINT('Ctrl Pts',(32.6985151554626,-30.3872716413479,42.2594709444902));
#21693=CARTESIAN_POINT('Ctrl Pts',(33.1102025176852,-30.7541295221294,42.222427681417));
#21694=CARTESIAN_POINT('Ctrl Pts',(33.4580908339469,-31.0641355659471,42.1911249998146));
#21695=CARTESIAN_POINT('Ctrl Pts',(33.6632925897301,-31.5342658601802,42.1598223182122));
#21696=CARTESIAN_POINT('Ctrl Pts',(33.6673070425528,-32.0013037875835,42.1285196366098));
#21697=CARTESIAN_POINT('Origin',(32.,-32.,48.));
#21698=CARTESIAN_POINT('',(33.6674738845699,-31.9987897819954,41.4285196366098));
#21699=CARTESIAN_POINT('',(33.6638410100825,-31.9990545799874,41.6214803633902));
#21700=CARTESIAN_POINT('',(33.666,-32.,48.));
#21701=CARTESIAN_POINT('',(30.7309291201476,-30.9206413469515,41.));
#21702=CARTESIAN_POINT('Ctrl Pts',(33.6674738845699,-31.9987897819954,41.4285196366098));
#21703=CARTESIAN_POINT('Ctrl Pts',(33.6635381632177,-32.4716720161883,41.3968095469596));
#21704=CARTESIAN_POINT('Ctrl Pts',(33.452320926774,-32.9475347722184,41.3650994573094));
#21705=CARTESIAN_POINT('Ctrl Pts',(33.0964755924645,-33.2578208392569,41.3333893676592));
#21706=CARTESIAN_POINT('Ctrl Pts',(32.6807822759957,-33.6202924858546,41.296346104586));
#21707=CARTESIAN_POINT('Ctrl Pts',(32.0677212020934,-33.7568087318644,41.2593028415127));
#21708=CARTESIAN_POINT('Ctrl Pts',(31.5378645772582,-33.6037827123866,41.2222595784395));
#21709=CARTESIAN_POINT('Ctrl Pts',(31.008007952423,-33.4507566929088,41.1852163153662));
#21710=CARTESIAN_POINT('Ctrl Pts',(30.5613557766549,-33.0081884079434,41.148173052293));
#21711=CARTESIAN_POINT('Ctrl Pts',(30.402364501489,-32.4811509461478,41.1111297892197));
#21712=CARTESIAN_POINT('Ctrl Pts',(30.2433732263231,-31.9541134843521,41.0740865261465));
#21713=CARTESIAN_POINT('Ctrl Pts',(30.3720428517593,-31.3426068457262,41.0370432630732));
#21714=CARTESIAN_POINT('Ctrl Pts',(30.7309291201476,-30.9206413469515,41.));
#21715=CARTESIAN_POINT('',(33.2714670322121,-30.9187899875149,41.));
#21716=CARTESIAN_POINT('Origin',(32.,-32.,41.));
#21717=CARTESIAN_POINT('Ctrl Pts',(33.2714683511891,-30.9187889684226,41.));
#21718=CARTESIAN_POINT('Ctrl Pts',(32.9206802420719,-30.5073507297867,41.0363148168373));
#21719=CARTESIAN_POINT('Ctrl Pts',(32.3508928184604,-30.2813273881367,41.0726296336745));
#21720=CARTESIAN_POINT('Ctrl Pts',(31.8135997916615,-30.3418001164503,41.1089444505117));
#21721=CARTESIAN_POINT('Ctrl Pts',(31.2655290956605,-30.4034858794192,41.1459877135849));
#21722=CARTESIAN_POINT('Ctrl Pts',(30.751269494614,-30.7632767551392,41.1830309766582));
#21723=CARTESIAN_POINT('Ctrl Pts',(30.5058096205078,-31.2569744715082,41.2200742397314));
#21724=CARTESIAN_POINT('Ctrl Pts',(30.2603497464016,-31.7506721878771,41.2571175028047));
#21725=CARTESIAN_POINT('Ctrl Pts',(30.2836895992358,-32.3782767448949,41.2941607658779));
#21726=CARTESIAN_POINT('Ctrl Pts',(30.5653173100033,-32.852378515895,41.3312040289512));
#21727=CARTESIAN_POINT('Ctrl Pts',(30.8469450207708,-33.326480286895,41.3682472920244));
#21728=CARTESIAN_POINT('Ctrl Pts',(31.3868605894716,-33.6470792718774,41.4052905550977));
#21729=CARTESIAN_POINT('Ctrl Pts',(31.9379165745124,-33.6675827533924,41.4423338181709));
#21730=CARTESIAN_POINT('Ctrl Pts',(32.4889725595533,-33.6880862349073,41.4793770812441));
#21731=CARTESIAN_POINT('Ctrl Pts',(33.0511689609341,-33.4084942129547,41.5164203443174));
#21732=CARTESIAN_POINT('Ctrl Pts',(33.3672906927666,-32.9566900927607,41.5534636073906));
#21733=CARTESIAN_POINT('Ctrl Pts',(33.5607723402275,-32.6801643221405,41.5761358593905));
#21734=CARTESIAN_POINT('Ctrl Pts',(33.6620737637366,-32.3391274427084,41.5988081113903));
#21735=CARTESIAN_POINT('Ctrl Pts',(33.6638410100825,-31.9990545799874,41.6214803633902));
#21736=CARTESIAN_POINT('Origin',(32.,-32.,39.4540747194623));
#21737=CARTESIAN_POINT('',(34.0532845839741,-31.9981685058867,53.7459252805377));
#21738=CARTESIAN_POINT('',(34.0546388766263,-32.0018310485179,53.8040747194623));
#21739=CARTESIAN_POINT('',(34.05475,-31.9999999999998,39.4540747194623));
#21740=CARTESIAN_POINT('',(31.6163320011532,-29.9813874990081,54.));
#21741=CARTESIAN_POINT('Ctrl Pts',(34.0546388766263,-32.0018310485179,53.8040747194623));
#21742=CARTESIAN_POINT('Ctrl Pts',(34.0493720989589,-31.4803615643801,53.832339883235));
#21743=CARTESIAN_POINT('Ctrl Pts',(33.5817165233639,-30.267781276506,53.8976483100809));
#21744=CARTESIAN_POINT('Ctrl Pts',(32.2875197530249,-29.8538180613451,53.9629567369268));
#21745=CARTESIAN_POINT('Ctrl Pts',(31.6163320011532,-29.9813874990081,54.));
#21746=CARTESIAN_POINT('',(30.6584342820381,-30.4387365847154,54.));
#21747=CARTESIAN_POINT('Origin',(32.,-32.,54.));
#21748=CARTESIAN_POINT('Ctrl Pts',(34.0532845839741,-31.9981685058867,53.7459252805377));
#21749=CARTESIAN_POINT('Ctrl Pts',(34.0549509938535,-31.7888165552494,53.7572587737813));
#21750=CARTESIAN_POINT('Ctrl Pts',(33.9292547539713,-30.8972175167488,53.8056355300982));
#21751=CARTESIAN_POINT('Ctrl Pts',(32.6546770307308,-29.6694113223394,53.8903271032523));
#21752=CARTESIAN_POINT('Ctrl Pts',(31.1647629871531,-30.0047891265576,53.9636851831628));
#21753=CARTESIAN_POINT('Ctrl Pts',(30.6584328706692,-30.4387350900138,54.));
#21754=CARTESIAN_POINT('Origin',(32.,-32.,39.4540747194623));
#21755=CARTESIAN_POINT('',(34.0520082578512,-32.0011056323104,53.0459252805377));
#21756=CARTESIAN_POINT('',(34.0578094041387,-31.9992426192728,53.1040747194623));
#21757=CARTESIAN_POINT('',(34.05475,-31.9999999999998,39.4540747194623));
#21758=CARTESIAN_POINT('Ctrl Pts',(34.0578094041387,-31.9992426192728,53.1040747194623));
#21759=CARTESIAN_POINT('Ctrl Pts',(34.0580096564622,-31.9570764465673,53.1063703750556));
#21760=CARTESIAN_POINT('Ctrl Pts',(34.0377190194437,-31.2347025738574,53.1457092937222));
#21761=CARTESIAN_POINT('Ctrl Pts',(33.188671237128,-29.8822030499806,53.2220914754619));
#21762=CARTESIAN_POINT('Ctrl Pts',(30.8656743801615,-29.8526922201837,53.3332212646816));
#21763=CARTESIAN_POINT('Ctrl Pts',(29.5804895672685,-31.7882160395824,53.4443510539014));
#21764=CARTESIAN_POINT('Ctrl Pts',(30.5102291276843,-33.9178753902133,53.5554808431211));
#21765=CARTESIAN_POINT('Ctrl Pts',(32.8021731990342,-34.291695073573,53.6666106323408));
#21766=CARTESIAN_POINT('Ctrl Pts',(33.9655643323599,-33.007470946703,53.7494752577879));
#21767=CARTESIAN_POINT('Ctrl Pts',(34.0562745401495,-32.1637799036814,53.7952966201617));
#21768=CARTESIAN_POINT('Ctrl Pts',(34.0546388766263,-32.0018310485179,53.8040747194623));
#21769=CARTESIAN_POINT('Ctrl Pts',(34.0520082578512,-32.0011056323104,53.0459252805377));
#21770=CARTESIAN_POINT('Ctrl Pts',(34.0499813688103,-31.5865449283087,53.0683325286752));
#21771=CARTESIAN_POINT('Ctrl Pts',(33.726754614814,-30.48373431258,53.127783039886));
#21772=CARTESIAN_POINT('Ctrl Pts',(31.9269572285084,-29.572527465193,53.2242768141699));
#21773=CARTESIAN_POINT('Ctrl Pts',(29.9209962036954,-30.7446672845728,53.3354066033898));
#21774=CARTESIAN_POINT('Ctrl Pts',(29.8177591150446,-33.0657522553465,53.4465363926093));
#21775=CARTESIAN_POINT('Ctrl Pts',(31.7116016656226,-34.4113173899075,53.5576661818292));
#21776=CARTESIAN_POINT('Ctrl Pts',(33.6494719430299,-33.6381800302083,53.6574624778052));
#21777=CARTESIAN_POINT('Ctrl Pts',(34.0495043713317,-32.473078610703,53.7202155107081));
#21778=CARTESIAN_POINT('Ctrl Pts',(34.0532845839741,-31.9981685058867,53.7459252805377));
#21779=CARTESIAN_POINT('Origin',(32.,-32.,39.4540747194623));
#21780=CARTESIAN_POINT('',(34.0573710650655,-32.0011268473916,52.3459252805377));
#21781=CARTESIAN_POINT('',(34.0524437812007,-31.99860578477,52.4040747194623));
#21782=CARTESIAN_POINT('',(34.05475,-31.9999999999998,39.4540747194623));
#21783=CARTESIAN_POINT('Ctrl Pts',(34.0524437812007,-31.99860578477,52.4040747194623));
#21784=CARTESIAN_POINT('Ctrl Pts',(34.0539874975223,-31.751387773122,52.4174441299495));
#21785=CARTESIAN_POINT('Ctrl Pts',(33.8982127967441,-30.8210709022261,52.4678568035099));
#21786=CARTESIAN_POINT('Ctrl Pts',(32.5140660253384,-29.6264478034877,52.5553127401435));
#21787=CARTESIAN_POINT('Ctrl Pts',(30.284773107188,-30.2806972020757,52.6664425293633));
#21788=CARTESIAN_POINT('Ctrl Pts',(29.6252320820182,-32.5084312487041,52.777572318583));
#21789=CARTESIAN_POINT('Ctrl Pts',(31.1390631138414,-34.2708597317664,52.8887021078028));
#21790=CARTESIAN_POINT('Ctrl Pts',(33.3932461919552,-33.9615363252737,52.9975362414291));
#21791=CARTESIAN_POINT('Ctrl Pts',(34.0547783357362,-32.6374801765024,53.0693271119824));
#21792=CARTESIAN_POINT('Ctrl Pts',(34.0578094041387,-31.9992426192728,53.1040747194623));
#21793=CARTESIAN_POINT('Ctrl Pts',(34.0573710650655,-32.0011268473916,52.3459252805377));
#21794=CARTESIAN_POINT('Ctrl Pts',(34.05330779479,-31.3858139390653,52.3794062835691));
#21795=CARTESIAN_POINT('Ctrl Pts',(33.4332399063797,-30.0826172598142,52.4499305496737));
#21796=CARTESIAN_POINT('Ctrl Pts',(31.2169954713513,-29.7011055471504,52.5574980788516));
#21797=CARTESIAN_POINT('Ctrl Pts',(29.6439536772523,-31.4108821177788,52.6686278680713));
#21798=CARTESIAN_POINT('Ctrl Pts',(30.2271406288629,-33.6598142860527,52.779757657291));
#21799=CARTESIAN_POINT('Ctrl Pts',(32.432827862626,-34.3896998451232,52.8908874465108));
#21800=CARTESIAN_POINT('Ctrl Pts',(33.8775323335813,-33.2263675462608,52.979609987593));
#21801=CARTESIAN_POINT('Ctrl Pts',(34.0533321856309,-32.2718892920576,53.031289265602));
#21802=CARTESIAN_POINT('Ctrl Pts',(34.0520082578512,-32.0011056323104,53.0459252805377));
#21803=CARTESIAN_POINT('Origin',(32.,-32.,39.4540747194623));
#21804=CARTESIAN_POINT('',(34.0554019757745,-31.9981759026781,51.6459252805377));
#21805=CARTESIAN_POINT('',(34.0527564122603,-32.0015414517042,51.7040747194623));
#21806=CARTESIAN_POINT('',(34.05475,-31.9999999999998,39.4540747194623));
#21807=CARTESIAN_POINT('Ctrl Pts',(34.0527564122603,-32.0015414517042,51.7040747194623));
#21808=CARTESIAN_POINT('Ctrl Pts',(34.0496053847508,-31.5497282207227,51.7285178848434));
#21809=CARTESIAN_POINT('Ctrl Pts',(33.680048118902,-30.4085132206192,51.7900043132977));
#21810=CARTESIAN_POINT('Ctrl Pts',(31.7940455863876,-29.5801661817881,51.8885340048252));
#21811=CARTESIAN_POINT('Ctrl Pts',(29.8553460280345,-30.8604947990401,51.9996637940449));
#21812=CARTESIAN_POINT('Ctrl Pts',(29.8794104413083,-33.1836861751323,52.1107935832647));
#21813=CARTESIAN_POINT('Ctrl Pts',(31.844215591537,-34.4235808867133,52.2219233724843));
#21814=CARTESIAN_POINT('Ctrl Pts',(33.6980657303603,-33.5631151460834,52.3196837512169));
#21815=CARTESIAN_POINT('Ctrl Pts',(34.0497102491075,-32.4363665050346,52.3804008668763));
#21816=CARTESIAN_POINT('Ctrl Pts',(34.0524437812007,-31.99860578477,52.4040747194623));
#21817=CARTESIAN_POINT('Ctrl Pts',(34.0554019757745,-31.9981759026781,51.6459252805377));
#21818=CARTESIAN_POINT('Ctrl Pts',(34.0566763311782,-31.859785689655,51.6534367753897));
#21819=CARTESIAN_POINT('Ctrl Pts',(33.9808503317639,-31.0403066930034,51.6979915333149));
#21820=CARTESIAN_POINT('Ctrl Pts',(32.8805414477757,-29.736670690513,51.7795895543136));
#21821=CARTESIAN_POINT('Ctrl Pts',(30.5761493204034,-30.0326001869503,51.8907193435332));
#21822=CARTESIAN_POINT('Ctrl Pts',(29.5748498880924,-32.1290726458106,52.001849132753));
#21823=CARTESIAN_POINT('Ctrl Pts',(30.7930215501968,-34.1074192405717,52.1129789219727));
#21824=CARTESIAN_POINT('Ctrl Pts',(33.1158067773521,-34.1570785575888,52.2241087111924));
#21825=CARTESIAN_POINT('Ctrl Pts',(34.0252705293619,-32.8124059202895,52.3017574973807));
#21826=CARTESIAN_POINT('Ctrl Pts',(34.0578033826196,-32.0665939597273,52.3423630204958));
#21827=CARTESIAN_POINT('Ctrl Pts',(34.0573710650655,-32.0011268473916,52.3459252805377));
#21828=CARTESIAN_POINT('Origin',(32.,-32.,39.4540747194623));
#21829=CARTESIAN_POINT('',(34.0514089344138,-32.0000193278948,50.9459252805377));
#21830=CARTESIAN_POINT('',(34.0579890512349,-32.0005154328357,51.0040747194623));
#21831=CARTESIAN_POINT('',(34.05475,-31.9999999999998,39.4540747194623));
#21832=CARTESIAN_POINT('Ctrl Pts',(34.057989051235,-32.0005154328357,51.0040747194623));
#21833=CARTESIAN_POINT('Ctrl Pts',(34.0557929694248,-31.3483062423322,51.0395916397373));
#21834=CARTESIAN_POINT('Ctrl Pts',(33.3683017673568,-30.0118742773859,51.1121518230855));
#21835=CARTESIAN_POINT('Ctrl Pts',(31.0922024613207,-29.7474644236002,51.2217552695068));
#21836=CARTESIAN_POINT('Ctrl Pts',(29.6152125517546,-31.5408685177941,51.3328850587265));
#21837=CARTESIAN_POINT('Ctrl Pts',(30.3207542514557,-33.7544647647039,51.4440148479463));
#21838=CARTESIAN_POINT('Ctrl Pts',(32.563123452382,-34.3623938867708,51.555144637166));
#21839=CARTESIAN_POINT('Ctrl Pts',(33.9102708685271,-33.1501141796208,51.6418312610047));
#21840=CARTESIAN_POINT('Ctrl Pts',(34.0543807212984,-32.2344446277146,51.6914746217701));
#21841=CARTESIAN_POINT('Ctrl Pts',(34.0527564122603,-32.0015414517042,51.7040747194623));
#21842=CARTESIAN_POINT('Ctrl Pts',(34.0514089344138,-32.0000193278948,50.9459252805377));
#21843=CARTESIAN_POINT('Ctrl Pts',(34.0513800613624,-31.6559195562416,50.9645105302836));
#21844=CARTESIAN_POINT('Ctrl Pts',(33.8061927556769,-30.6259373145995,51.0201390431027));
#21845=CARTESIAN_POINT('Ctrl Pts',(32.1767300235671,-29.5778564663098,51.1128108189952));
#21846=CARTESIAN_POINT('Ctrl Pts',(30.0609756751137,-30.5377423393424,51.2239406082148));
#21847=CARTESIAN_POINT('Ctrl Pts',(29.7197953608552,-32.8358705657033,51.3350703974346));
#21848=CARTESIAN_POINT('Ctrl Pts',(31.465433604746,-34.3690191153306,51.4462001866543));
#21849=CARTESIAN_POINT('Ctrl Pts',(33.5492418405736,-33.7769847980368,51.5498184810221));
#21850=CARTESIAN_POINT('Ctrl Pts',(34.0503917921621,-32.5422630352122,51.6163935123165));
#21851=CARTESIAN_POINT('Ctrl Pts',(34.0554019757745,-31.9981759026781,51.6459252805377));
#21852=CARTESIAN_POINT('Origin',(32.,-32.,39.4540747194623));
#21853=CARTESIAN_POINT('',(34.055472908735,-32.0018139477898,50.2459252805377));
#21854=CARTESIAN_POINT('',(34.0542687450602,-31.9981314910207,50.3040747194623));
#21855=CARTESIAN_POINT('',(34.05475,-31.9999999999998,39.4540747194623));
#21856=CARTESIAN_POINT('Ctrl Pts',(34.0542687450602,-31.9981314910207,50.3040747194623));
#21857=CARTESIAN_POINT('Ctrl Pts',(34.0558440944503,-31.8219835585998,50.3136221315579));
#21858=CARTESIAN_POINT('Ctrl Pts',(33.9544817357664,-30.9641799391559,50.3602128067267));
#21859=CARTESIAN_POINT('Ctrl Pts',(32.7551980511737,-29.6918213247557,50.4438467449688));
#21860=CARTESIAN_POINT('Ctrl Pts',(30.470483670184,-30.1135767468053,50.5549765341884));
#21861=CARTESIAN_POINT('Ctrl Pts',(29.5855660473401,-32.2617662727765,50.6661063234083));
#21862=CARTESIAN_POINT('Ctrl Pts',(30.9103121945009,-34.1703901446276,50.7772361126279));
#21863=CARTESIAN_POINT('Ctrl Pts',(33.2323288041292,-34.0926964930404,50.8883659018477));
#21864=CARTESIAN_POINT('Ctrl Pts',(34.0448660118093,-32.7367198389241,50.9639787707924));
#21865=CARTESIAN_POINT('Ctrl Pts',(34.0580834280455,-32.0285441806329,51.002548376664));
#21866=CARTESIAN_POINT('Ctrl Pts',(34.057989051235,-32.0005154328357,51.0040747194623));
#21867=CARTESIAN_POINT('Ctrl Pts',(34.055472908735,-32.0018139477898,50.2459252805377));
#21868=CARTESIAN_POINT('Ctrl Pts',(34.0504505301634,-31.4554311545241,50.2755842851775));
#21869=CARTESIAN_POINT('Ctrl Pts',(33.5457056833664,-30.2184358152945,50.3422865528905));
#21870=CARTESIAN_POINT('Ctrl Pts',(31.4573199910465,-29.6328263251734,50.4460320836768));
#21871=CARTESIAN_POINT('Ctrl Pts',(29.7169448784392,-31.1719467946929,50.5571618728964));
#21872=CARTESIAN_POINT('Ctrl Pts',(30.0659970543811,-33.4688925778434,50.6682916621163));
#21873=CARTESIAN_POINT('Ctrl Pts',(32.1850277527679,-34.4215238032342,50.7794214513359));
#21874=CARTESIAN_POINT('Ctrl Pts',(33.8086577032695,-33.3693128790145,50.8719659908098));
#21875=CARTESIAN_POINT('Ctrl Pts',(34.0514376097974,-32.3417633592069,50.9274672672104));
#21876=CARTESIAN_POINT('Ctrl Pts',(34.0514089344138,-32.0000193278948,50.9459252805377));
#21877=CARTESIAN_POINT('Origin',(32.,-32.,39.4540747194623));
#21878=CARTESIAN_POINT('',(34.0573202636303,-31.9988395216185,49.5459252805377));
#21879=CARTESIAN_POINT('',(34.0515870098674,-32.0006260541466,49.6040747194623));
#21880=CARTESIAN_POINT('',(34.05475,-31.9999999999998,39.4540747194623));
#21881=CARTESIAN_POINT('Ctrl Pts',(34.0515870098674,-32.0006260541466,49.6040747194623));
#21882=CARTESIAN_POINT('Ctrl Pts',(34.0505442505756,-31.6189146354342,49.6246958864518));
#21883=CARTESIAN_POINT('Ctrl Pts',(33.7651923215172,-30.5500595553348,49.6823603165144));
#21884=CARTESIAN_POINT('Ctrl Pts',(32.0437417120601,-29.5718114661385,49.7770680096504));
#21885=CARTESIAN_POINT('Ctrl Pts',(29.9837635871641,-30.6461892226366,49.8881977988701));
#21886=CARTESIAN_POINT('Ctrl Pts',(29.7690231621222,-32.9595599211113,49.9993275880899));
#21887=CARTESIAN_POINT('Ctrl Pts',(31.5960485451694,-34.3947517857787,50.1104573773095));
#21888=CARTESIAN_POINT('Ctrl Pts',(33.6040409500067,-33.7032818934708,50.2120397544338));
#21889=CARTESIAN_POINT('Ctrl Pts',(34.0497318536352,-32.5054246979535,50.2765788684846));
#21890=CARTESIAN_POINT('Ctrl Pts',(34.0542687450602,-31.9981314910207,50.3040747194623));
#21891=CARTESIAN_POINT('Ctrl Pts',(34.0573202636303,-31.9988395216185,49.5459252805377));
#21892=CARTESIAN_POINT('Ctrl Pts',(34.0577786805335,-31.9310296536276,49.5496147769981));
#21893=CARTESIAN_POINT('Ctrl Pts',(34.0239729579483,-31.1828581577522,49.5903475365317));
#21894=CARTESIAN_POINT('Ctrl Pts',(33.1084096420059,-29.8391110939209,49.6681235591387));
#21895=CARTESIAN_POINT('Ctrl Pts',(30.785808172351,-29.8967284995564,49.7792533483584));
#21896=CARTESIAN_POINT('Ctrl Pts',(29.5744218959985,-31.8792371733684,49.8903831375781));
#21897=CARTESIAN_POINT('Ctrl Pts',(30.5828983961289,-33.9722666764952,50.0015129267979));
#21898=CARTESIAN_POINT('Ctrl Pts',(32.8882909162952,-34.2602991056352,50.1126427160176));
#21899=CARTESIAN_POINT('Ctrl Pts',(33.9824180683095,-32.9549395059557,50.1941135005975));
#21900=CARTESIAN_POINT('Ctrl Pts',(34.0567233398191,-32.1378479043595,50.2385410221042));
#21901=CARTESIAN_POINT('Ctrl Pts',(34.055472908735,-32.0018139477898,50.2459252805377));
#21902=CARTESIAN_POINT('Origin',(32.,-32.,39.4540747194623));
#21903=CARTESIAN_POINT('',(34.0519708956138,-31.9989253245976,48.8459252805377));
#21904=CARTESIAN_POINT('',(34.0565621614737,-32.0015359425915,48.9040747194623));
#21905=CARTESIAN_POINT('',(34.05475,-31.9999999999998,39.4540747194623));
#21906=CARTESIAN_POINT('Ctrl Pts',(34.0565621614737,-32.0015359425915,48.9040747194623));
#21907=CARTESIAN_POINT('Ctrl Pts',(34.0516979528083,-31.418447338828,48.9357696413457));
#21908=CARTESIAN_POINT('Ctrl Pts',(33.4873124744596,-30.1456437189272,49.0045078263022));
#21909=CARTESIAN_POINT('Ctrl Pts',(31.3284246265722,-29.6661192380166,49.1102892743321));
#21910=CARTESIAN_POINT('Ctrl Pts',(29.6750012716246,-31.2982922215028,49.2214190635517));
#21911=CARTESIAN_POINT('Ctrl Pts',(30.1493915393249,-33.5726605541655,49.3325488527715));
#21912=CARTESIAN_POINT('Ctrl Pts',(32.317438601222,-34.4077470024496,49.4436786419912));
#21913=CARTESIAN_POINT('Ctrl Pts',(33.8465759975202,-33.2932195337787,49.5341872642215));
#21914=CARTESIAN_POINT('Ctrl Pts',(34.0524174329609,-32.3046098974271,49.5876526233785));
#21915=CARTESIAN_POINT('Ctrl Pts',(34.0515870098674,-32.0006260541466,49.6040747194623));
#21916=CARTESIAN_POINT('Ctrl Pts',(34.0519708956138,-31.9989253245976,48.8459252805377));
#21917=CARTESIAN_POINT('Ctrl Pts',(34.0532663991156,-31.7257756104976,48.860688531892));
#21918=CARTESIAN_POINT('Ctrl Pts',(33.8753960113233,-30.7688700324249,48.9124950463195));
#21919=CARTESIAN_POINT('Ctrl Pts',(32.4246384795753,-29.6088297926389,49.0013448238203));
#21920=CARTESIAN_POINT('Ctrl Pts',(30.2214637798412,-30.34627036294,49.1124746130401));
#21921=CARTESIAN_POINT('Ctrl Pts',(29.6459861413742,-32.5971863631273,49.2236044022597));
#21922=CARTESIAN_POINT('Ctrl Pts',(31.2248764581043,-34.3015638799969,49.3347341914795));
#21923=CARTESIAN_POINT('Ctrl Pts',(33.4371809635416,-33.9129210756653,49.4421744842388));
#21924=CARTESIAN_POINT('Ctrl Pts',(34.0531760855389,-32.6118539357201,49.5125715139249));
#21925=CARTESIAN_POINT('Ctrl Pts',(34.0573202636303,-31.9988395216185,49.5459252805377));
#21926=CARTESIAN_POINT('Origin',(32.,-32.,39.4540747194623));
#21927=CARTESIAN_POINT('',(34.0534017172989,-32.0017453556898,48.1459252805377));
#21928=CARTESIAN_POINT('',(34.056369973564,-31.9983965631577,48.2040747194623));
#21929=CARTESIAN_POINT('',(34.05475,-31.9999999999998,39.4540747194623));
#21930=CARTESIAN_POINT('Ctrl Pts',(34.056369973564,-31.9983965631577,48.2040747194623));
#21931=CARTESIAN_POINT('Ctrl Pts',(34.0572746156918,-31.8930410344953,48.2098001331663));
#21932=CARTESIAN_POINT('Ctrl Pts',(34.0020141870959,-31.106989754687,48.2525688099435));
#21933=CARTESIAN_POINT('Ctrl Pts',(32.9883371782127,-29.7816216473485,48.3323807497939));
#21934=CARTESIAN_POINT('Ctrl Pts',(30.6723823629214,-29.966420814655,48.4435105390137));
#21935=CARTESIAN_POINT('Ctrl Pts',(29.5714488116707,-32.0123295991414,48.5546403282333));
#21936=CARTESIAN_POINT('Ctrl Pts',(30.693098971438,-34.0469544682025,48.6657701174531));
#21937=CARTESIAN_POINT('Ctrl Pts',(33.0108107797937,-34.2082288062616,48.7768999066728));
#21938=CARTESIAN_POINT('Ctrl Pts',(34.0062529590955,-32.8789465616399,48.8563347740093));
#21939=CARTESIAN_POINT('Ctrl Pts',(34.0573829695406,-32.09992889047,48.8987263782724));
#21940=CARTESIAN_POINT('Ctrl Pts',(34.0565621614737,-32.0015359425915,48.9040747194623));
#21941=CARTESIAN_POINT('Ctrl Pts',(34.0534017172989,-32.0017453556898,48.1459252805377));
#21942=CARTESIAN_POINT('Ctrl Pts',(34.0495478617348,-31.524546624056,48.1717622867859));
#21943=CARTESIAN_POINT('Ctrl Pts',(33.6462462789142,-30.3572999443065,48.2346425561073));
#21944=CARTESIAN_POINT('Ctrl Pts',(31.7033877262933,-29.5895987972966,48.334566088502));
#21945=CARTESIAN_POINT('Ctrl Pts',(29.8140971767976,-30.9417742932515,48.4456958777216));
#21946=CARTESIAN_POINT('Ctrl Pts',(29.9253211859677,-33.2624264800428,48.5568256669414));
#21947=CARTESIAN_POINT('Ctrl Pts',(31.9352687467854,-34.427719642744,48.6679554561611));
#21948=CARTESIAN_POINT('Ctrl Pts',(33.7295722549086,-33.5115468202576,48.7643219940266));
#21949=CARTESIAN_POINT('Ctrl Pts',(34.050015782034,-32.4111501580791,48.8236452688187));
#21950=CARTESIAN_POINT('Ctrl Pts',(34.0519708956138,-31.9989253245976,48.8459252805377));
#21951=CARTESIAN_POINT('Origin',(32.,-32.,39.4540747194623));
#21952=CARTESIAN_POINT('',(34.0581462892693,-32.0000454490473,47.4459252805377));
#21953=CARTESIAN_POINT('',(34.0515290217428,-31.9994832228354,47.5040747194623));
#21954=CARTESIAN_POINT('',(34.05475,-31.9999999999998,39.4540747194623));
#21955=CARTESIAN_POINT('Ctrl Pts',(34.0515290217428,-31.9994832228354,47.5040747194623));
#21956=CARTESIAN_POINT('Ctrl Pts',(34.0522291138724,-31.6884975730474,47.5208738880602));
#21957=CARTESIAN_POINT('Ctrl Pts',(33.8397673943927,-30.6926760820841,47.5747163197312));
#21958=CARTESIAN_POINT('Ctrl Pts',(32.2929749124037,-29.5891539671616,47.6656020144756));
#21959=CARTESIAN_POINT('Ctrl Pts',(30.1335187541459,-30.4462108726646,47.7767318036953));
#21960=CARTESIAN_POINT('Ctrl Pts',(29.6822459909475,-32.7252787373636,47.8878615929151));
#21961=CARTESIAN_POINT('Ctrl Pts',(31.3521565618384,-34.3405793669477,47.9989913821348));
#21962=CARTESIAN_POINT('Ctrl Pts',(33.4983863159947,-33.8409464804423,48.1043957576506));
#21963=CARTESIAN_POINT('Ctrl Pts',(34.0514216069734,-32.5746882946331,48.172756870093));
#21964=CARTESIAN_POINT('Ctrl Pts',(34.056369973564,-31.9983965631577,48.2040747194623));
#21965=CARTESIAN_POINT('Ctrl Pts',(34.0581458051732,-32.0000454425691,47.4459252805377));
#21966=CARTESIAN_POINT('Ctrl Pts',(34.057925295782,-31.3223792843277,47.4828360416798));
#21967=CARTESIAN_POINT('Ctrl Pts',(33.321785989982,-29.9642037469477,47.556790065895));
#21968=CARTESIAN_POINT('Ctrl Pts',(31.008316669847,-29.7831154807695,47.6677873531836));
#21969=CARTESIAN_POINT('Ctrl Pts',(29.59966349763,-31.6306797131245,47.7789171424033));
#21970=CARTESIAN_POINT('Ctrl Pts',(30.3877722618167,-33.8162418669164,47.8900469316231));
#21971=CARTESIAN_POINT('Ctrl Pts',(32.6513743681069,-34.3395991604291,48.0011767208428));
#21972=CARTESIAN_POINT('Ctrl Pts',(33.9311686773918,-33.0979137221593,48.0864695038144));
#21973=CARTESIAN_POINT('Ctrl Pts',(34.055073245912,-32.208720246353,48.1347190237126));
#21974=CARTESIAN_POINT('Ctrl Pts',(34.0534017172989,-32.0017453556898,48.1459252805377));
#21975=CARTESIAN_POINT('Origin',(32.,-32.,39.4540747194623));
#21976=CARTESIAN_POINT('',(34.0535341382367,-31.9982258659195,46.7459252805377));
#21977=CARTESIAN_POINT('',(34.0544757027884,-32.0018769326718,46.8040747194623));
#21978=CARTESIAN_POINT('',(34.05475,-31.9999999999998,39.4540747194623));
#21979=CARTESIAN_POINT('Ctrl Pts',(34.0544757027884,-32.0018769326718,46.8040747194623));
#21980=CARTESIAN_POINT('Ctrl Pts',(34.0498160242977,-31.4877588190714,46.831947642954));
#21981=CARTESIAN_POINT('Ctrl Pts',(33.5941431221402,-30.2830100163635,46.896863829519));
#21982=CARTESIAN_POINT('Ctrl Pts',(31.5717539918218,-29.6094732275437,46.9988232791572));
#21983=CARTESIAN_POINT('Ctrl Pts',(29.7593951696295,-31.0631420131788,47.1099530683769));
#21984=CARTESIAN_POINT('Ctrl Pts',(29.9976135898446,-33.3742130685507,47.2210828575967));
#21985=CARTESIAN_POINT('Ctrl Pts',(32.0683943376577,-34.4276192263053,47.3322126468163));
#21986=CARTESIAN_POINT('Ctrl Pts',(33.7730095140328,-33.4359068477222,47.4265432674384));
#21987=CARTESIAN_POINT('Ctrl Pts',(34.0506853650385,-32.3742412257766,47.4838306249869));
#21988=CARTESIAN_POINT('Ctrl Pts',(34.0515290217428,-31.9994832228354,47.5040747194623));
#21989=CARTESIAN_POINT('Ctrl Pts',(34.0535341382367,-31.9982258659195,46.7459252805377));
#21990=CARTESIAN_POINT('Ctrl Pts',(34.0552008741846,-31.7961784564346,46.7568665335004));
#21991=CARTESIAN_POINT('Ctrl Pts',(33.9350054837422,-30.9120087675869,46.8048510495363));
#21992=CARTESIAN_POINT('Ctrl Pts',(32.6680530383748,-29.6651085813628,46.8898788286456));
#21993=CARTESIAN_POINT('Ctrl Pts',(30.4007739163126,-30.172299605471,47.0010086178652));
#21994=CARTESIAN_POINT('Ctrl Pts',(29.5970891631565,-32.3521822100667,47.112138407085));
#21995=CARTESIAN_POINT('Ctrl Pts',(30.9925223493965,-34.2097514752664,47.2232681963047));
#21996=CARTESIAN_POINT('Ctrl Pts',(33.3099881558288,-34.0449801540592,47.3343979855244));
#21997=CARTESIAN_POINT('Ctrl Pts',(34.057041091318,-32.685008900317,47.4086170136021));
#21998=CARTESIAN_POINT('Ctrl Pts',(34.0581465967559,-32.0024781226841,47.4457927786065));
#21999=CARTESIAN_POINT('Ctrl Pts',(34.0581458051732,-32.0000454425691,47.4459252805377));
#22000=CARTESIAN_POINT('Origin',(32.,-32.,39.4540747194623));
#22001=CARTESIAN_POINT('',(34.0518959520928,-32.0010072981031,46.0459252805377));
#22002=CARTESIAN_POINT('',(34.0579058351471,-31.9993626137656,46.1040747194623));
#22003=CARTESIAN_POINT('',(34.05475,-31.9999999999998,39.4540747194623));
#22004=CARTESIAN_POINT('Ctrl Pts',(34.0579058351471,-31.9993626137656,46.1040747194623));
#22005=CARTESIAN_POINT('Ctrl Pts',(34.0580481959426,-31.96440578177,46.1059781347747));
#22006=CARTESIAN_POINT('Ctrl Pts',(34.0414007129417,-31.2492759708491,46.1449248131603));
#22007=CARTESIAN_POINT('Ctrl Pts',(33.2110168535402,-29.8948987972565,46.2209147546191));
#22008=CARTESIAN_POINT('Ctrl Pts',(30.8883310710498,-29.8407860027877,46.3320445438389));
#22009=CARTESIAN_POINT('Ctrl Pts',(29.5830326367871,-31.7627624428669,46.4431743330586));
#22010=CARTESIAN_POINT('Ctrl Pts',(30.4897165224173,-33.9018561225001,46.5543041222784));
#22011=CARTESIAN_POINT('Ctrl Pts',(32.7785954683888,-34.300391703592,46.665433911498));
#22012=CARTESIAN_POINT('Ctrl Pts',(33.9595497245257,-33.0217127890764,46.748690777226));
#22013=CARTESIAN_POINT('Ctrl Pts',(34.0560087617125,-32.1710245173564,46.7949043798808));
#22014=CARTESIAN_POINT('Ctrl Pts',(34.0544757027884,-32.0018769326718,46.8040747194623));
#22015=CARTESIAN_POINT('Ctrl Pts',(34.0518959520928,-32.0010072981031,46.0459252805377));
#22016=CARTESIAN_POINT('Ctrl Pts',(34.0500891203468,-31.5936483306361,46.0679402883943));
#22017=CARTESIAN_POINT('Ctrl Pts',(33.7353983817626,-30.4982792184681,46.1269985593241));
#22018=CARTESIAN_POINT('Ctrl Pts',(31.9525944730258,-29.5718802511161,46.2231000933272));
#22019=CARTESIAN_POINT('Ctrl Pts',(29.9343826179068,-30.7228008652907,46.3342298825469));
#22020=CARTESIAN_POINT('Ctrl Pts',(29.8066013901918,-33.0426002769034,46.4453596717666));
#22021=CARTESIAN_POINT('Ctrl Pts',(31.6861947837558,-34.4082232216233,46.5564894609863));
#22022=CARTESIAN_POINT('Ctrl Pts',(33.6396491312149,-33.6524065822643,46.6566779972434));
#22023=CARTESIAN_POINT('Ctrl Pts',(34.0495578881022,-32.4802404526548,46.7198232704271));
#22024=CARTESIAN_POINT('Ctrl Pts',(34.0535341382367,-31.9982258659195,46.7459252805377));
#22025=CARTESIAN_POINT('Origin',(32.,-32.,39.4540747194623));
#22026=CARTESIAN_POINT('',(34.0572106602559,-32.0012284763881,45.3459252805377));
#22027=CARTESIAN_POINT('',(34.0525988691351,-31.9985278358415,45.4040747194623));
#22028=CARTESIAN_POINT('',(34.05475,-31.9999999999998,39.4540747194623));
#22029=CARTESIAN_POINT('Ctrl Pts',(34.0525988691351,-31.9985278358415,45.4040747194623));
#22030=CARTESIAN_POINT('Ctrl Pts',(34.0541886318456,-31.758608443519,45.4170518896685));
#22031=CARTESIAN_POINT('Ctrl Pts',(33.9044076954203,-30.8357624066553,45.467072322948));
#22032=CARTESIAN_POINT('Ctrl Pts',(32.539107595012,-29.6320101574646,45.5541360193008));
#22033=CARTESIAN_POINT('Ctrl Pts',(30.3030266643161,-30.2626760833603,45.6652658085204));
#22034=CARTESIAN_POINT('Ctrl Pts',(29.6199973275285,-32.4833220172713,45.7763955977403));
#22035=CARTESIAN_POINT('Ctrl Pts',(31.1151206265327,-34.2616368823846,45.88752538696));
#22036=CARTESIAN_POINT('Ctrl Pts',(33.3805969835407,-33.9751191529232,45.9967517608673));
#22037=CARTESIAN_POINT('Ctrl Pts',(34.0552776453628,-32.6447171754051,46.0689348717015));
#22038=CARTESIAN_POINT('Ctrl Pts',(34.0579058351471,-31.9993626137656,46.1040747194623));
#22039=CARTESIAN_POINT('Ctrl Pts',(34.0572106602559,-32.0012284763882,45.3459252805377));
#22040=CARTESIAN_POINT('Ctrl Pts',(34.0529103405582,-31.3929993751285,45.3790140432881));
#22041=CARTESIAN_POINT('Ctrl Pts',(33.4453451554924,-30.0963857660314,45.4491460691118));
#22042=CARTESIAN_POINT('Ctrl Pts',(31.2413200309736,-29.6929634802401,45.5563213580089));
#22043=CARTESIAN_POINT('Ctrl Pts',(29.6503075674633,-31.3860307243948,45.6674511472285));
#22044=CARTESIAN_POINT('Ctrl Pts',(30.2097081368571,-33.6409959913638,45.7785809364483));
#22045=CARTESIAN_POINT('Ctrl Pts',(32.4075644044926,-34.3941395228971,45.8897107256679));
#22046=CARTESIAN_POINT('Ctrl Pts',(33.8709146012435,-33.2410523704688,45.9788255070311));
#22047=CARTESIAN_POINT('Ctrl Pts',(34.0531293619917,-32.2790855330859,46.030897025321));
#22048=CARTESIAN_POINT('Ctrl Pts',(34.0518959520928,-32.0010072981031,46.0459252805377));
#22049=CARTESIAN_POINT('Origin',(32.,-32.,39.4540747194623));
#22050=CARTESIAN_POINT('',(34.0556200578454,-31.9982099716569,44.6459252805377));
#22051=CARTESIAN_POINT('',(34.0525927001132,-32.0014692602189,44.7040747194623));
#22052=CARTESIAN_POINT('',(34.05475,-31.9999999999998,39.4540747194623));
#22053=CARTESIAN_POINT('Ctrl Pts',(34.0525927001132,-32.0014692602189,44.7040747194623));
#22054=CARTESIAN_POINT('Ctrl Pts',(34.0496527323428,-31.5568170867306,44.7281256445624));
#22055=CARTESIAN_POINT('Ctrl Pts',(33.689290920656,-30.4229699899486,44.7892198327358));
#22056=CARTESIAN_POINT('Ctrl Pts',(31.819615432301,-29.5781258700983,44.8873572839824));
#22057=CARTESIAN_POINT('Ctrl Pts',(29.8675011150493,-30.8379064585695,44.9984870732022));
#22058=CARTESIAN_POINT('Ctrl Pts',(29.867026651317,-33.1612224537781,45.1096168624218));
#22059=CARTESIAN_POINT('Ctrl Pts',(31.8186262651666,-34.4218002522221,45.2207466516416));
#22060=CARTESIAN_POINT('Ctrl Pts',(33.6889356864207,-33.5775893888604,45.3188992706551));
#22061=CARTESIAN_POINT('Ctrl Pts',(34.0496506626755,-32.4434570680596,45.3800086265953));
#22062=CARTESIAN_POINT('Ctrl Pts',(34.0525988691351,-31.9985278358415,45.4040747194623));
#22063=CARTESIAN_POINT('Ctrl Pts',(34.0556200578454,-31.9982099716569,44.6459252805377));
#22064=CARTESIAN_POINT('Ctrl Pts',(34.0568191781729,-31.8670821375068,44.6530445351088));
#22065=CARTESIAN_POINT('Ctrl Pts',(33.9856534619524,-31.054959944858,44.6972070527531));
#22066=CARTESIAN_POINT('Ctrl Pts',(32.9043976734169,-29.7460972409556,44.7784128334707));
#22067=CARTESIAN_POINT('Ctrl Pts',(30.5970084672143,-30.0176711781749,44.8895426226904));
#22068=CARTESIAN_POINT('Ctrl Pts',(29.573621897008,-32.1034509556668,45.0006724119102));
#22069=CARTESIAN_POINT('Ctrl Pts',(30.770830253685,-34.0945535404118,45.1118022011299));
#22070=CARTESIAN_POINT('Ctrl Pts',(33.0929614323987,-34.168743439459,45.2229319903496));
#22071=CARTESIAN_POINT('Ctrl Pts',(34.0212425079456,-32.8270078695086,45.3009730168189));
#22072=CARTESIAN_POINT('Ctrl Pts',(34.0577245995579,-32.0739190812136,45.3419707802149));
#22073=CARTESIAN_POINT('Ctrl Pts',(34.0572106602559,-32.0012284763882,45.3459252805377));
#22074=CARTESIAN_POINT('Origin',(32.,-32.,39.4540747194623));
#22075=CARTESIAN_POINT('',(34.0514131663913,-31.9999002048757,43.9459252805377));
#22076=CARTESIAN_POINT('',(34.0579021590917,-32.0006422250077,44.0040747194623));
#22077=CARTESIAN_POINT('',(34.05475,-31.9999999999998,39.4540747194623));
#22078=CARTESIAN_POINT('Ctrl Pts',(34.0579021590918,-32.0006422250077,44.0040747194623));
#22079=CARTESIAN_POINT('Ctrl Pts',(34.0552574521282,-31.3555631515598,44.0391993994563));
#22080=CARTESIAN_POINT('Ctrl Pts',(33.3810889993931,-30.0254049823542,44.1113673425236));
#22081=CARTESIAN_POINT('Ctrl Pts',(31.116044435755,-29.7380018890796,44.220578548664));
#22082=CARTESIAN_POINT('Ctrl Pts',(29.6201949324755,-31.5157059427025,44.3317083378838));
#22083=CARTESIAN_POINT('Ctrl Pts',(30.3023172190834,-33.7366306656069,44.4428381271035));
#22084=CARTESIAN_POINT('Ctrl Pts',(32.538140376183,-34.3682098363267,44.5539679163233));
#22085=CARTESIAN_POINT('Ctrl Pts',(33.9041699601015,-33.1648057121054,44.6410467804428));
#22086=CARTESIAN_POINT('Ctrl Pts',(34.0541808741541,-32.2416708863265,44.6910823814892));
#22087=CARTESIAN_POINT('Ctrl Pts',(34.0525927001132,-32.0014692602189,44.7040747194623));
#22088=CARTESIAN_POINT('Ctrl Pts',(34.0514131663913,-31.9999002048757,43.9459252805377));
#22089=CARTESIAN_POINT('Ctrl Pts',(34.0515591161687,-31.6630643659418,43.9641182900027));
#22090=CARTESIAN_POINT('Ctrl Pts',(33.8137553061809,-30.6405823346687,44.0193545625409));
#22091=CARTESIAN_POINT('Ctrl Pts',(32.2023029066813,-29.5798581998207,44.1116340981523));
#22092=CARTESIAN_POINT('Ctrl Pts',(30.0765282356173,-30.5173438798798,44.2227638873721));
#22093=CARTESIAN_POINT('Ctrl Pts',(29.7110940641655,-32.8117403622951,44.3338936765918));
#22094=CARTESIAN_POINT('Ctrl Pts',(31.4404417830221,-34.3632408681166,44.4450234658115));
#22095=CARTESIAN_POINT('Ctrl Pts',(33.5382982167491,-33.7910911423125,44.5490340004602));
#22096=CARTESIAN_POINT('Ctrl Pts',(34.0505798550385,-32.5493730723421,44.6160012720355));
#22097=CARTESIAN_POINT('Ctrl Pts',(34.0556200578454,-31.9982099716569,44.6459252805377));
#22098=CARTESIAN_POINT('Origin',(32.,-32.,39.4540747194623));
#22099=CARTESIAN_POINT('',(34.055253827614,-32.0018424470648,43.2459252805377));
#22100=CARTESIAN_POINT('',(34.0544840782063,-31.9981228849384,43.3040747194623));
#22101=CARTESIAN_POINT('',(34.05475,-31.9999999999998,39.4540747194623));
#22102=CARTESIAN_POINT('Ctrl Pts',(34.0544840782063,-31.9981228849384,43.3040747194623));
#22103=CARTESIAN_POINT('Ctrl Pts',(34.0560152931149,-31.8292568267182,43.313229891277));
#22104=CARTESIAN_POINT('Ctrl Pts',(33.9597518145395,-30.9788546094819,43.3594283261648));
#22105=CARTESIAN_POINT('Ctrl Pts',(32.7795349677293,-29.699926495664,43.442670024126));
#22106=CARTESIAN_POINT('Ctrl Pts',(30.490493436163,-30.0975271807692,43.5537998133457));
#22107=CARTESIAN_POINT('Ctrl Pts',(29.5829359418664,-32.2362503593823,43.6649296025654));
#22108=CARTESIAN_POINT('Ctrl Pts',(30.887449261624,-34.1587597707098,43.7760593917852));
#22109=CARTESIAN_POINT('Ctrl Pts',(33.2101569520236,-34.1055956508643,43.8871891810049));
#22110=CARTESIAN_POINT('Ctrl Pts',(34.0412597763805,-32.7512874803452,43.9631942902306));
#22111=CARTESIAN_POINT('Ctrl Pts',(34.058046618487,-32.0358777857388,44.0021561363831));
#22112=CARTESIAN_POINT('Ctrl Pts',(34.0579021590918,-32.0006422250077,44.0040747194623));
#22113=CARTESIAN_POINT('Ctrl Pts',(34.055253827614,-32.0018424470648,43.2459252805377));
#22114=CARTESIAN_POINT('Ctrl Pts',(34.0502763403136,-31.462537786081,43.2751920448965));
#22115=CARTESIAN_POINT('Ctrl Pts',(33.5565644616089,-30.2325636359862,43.3415020723286));
#22116=CARTESIAN_POINT('Ctrl Pts',(31.4823524106659,-29.6272265641889,43.444855362834));
#22117=CARTESIAN_POINT('Ctrl Pts',(29.725818144952,-31.1478792982686,43.5559851520537));
#22118=CARTESIAN_POINT('Ctrl Pts',(30.0505904524204,-33.4483836551904,43.6671149412735));
#22119=CARTESIAN_POINT('Ctrl Pts',(32.1594412363987,-34.4233429992207,43.7782447304931));
#22120=CARTESIAN_POINT('Ctrl Pts',(33.8010224036592,-33.3839528343674,43.8711815102479));
#22121=CARTESIAN_POINT('Ctrl Pts',(34.0512619440044,-32.3489046398197,43.9270750269294));
#22122=CARTESIAN_POINT('Ctrl Pts',(34.0514131663913,-31.9999002048757,43.9459252805377));
#22123=CARTESIAN_POINT('Origin',(32.,-32.,39.4540747194623));
#22124=CARTESIAN_POINT('',(34.0574728862044,-31.9989451473756,42.5459252805377));
#22125=CARTESIAN_POINT('',(34.0515269223438,-32.0005123640606,42.6040747194623));
#22126=CARTESIAN_POINT('',(34.05475,-31.9999999999998,39.4540747194623));
#22127=CARTESIAN_POINT('Ctrl Pts',(34.0515269223438,-32.0005123640606,42.6040747194623));
#22128=CARTESIAN_POINT('Ctrl Pts',(34.0506911852892,-31.6260341786675,42.6243036461709));
#22129=CARTESIAN_POINT('Ctrl Pts',(33.7733218188497,-30.564657819967,42.6815758359526));
#22130=CARTESIAN_POINT('Ctrl Pts',(32.0693858594061,-29.572408937857,42.7758912888076));
#22131=CARTESIAN_POINT('Ctrl Pts',(29.9981750364838,-30.6249691844573,42.8870210780273));
#22132=CARTESIAN_POINT('Ctrl Pts',(29.7590127090568,-32.9359427703937,42.9981508672471));
#22133=CARTESIAN_POINT('Ctrl Pts',(31.5707776489307,-34.3903516582226,43.1092806564667));
#22134=CARTESIAN_POINT('Ctrl Pts',(33.5937426045007,-33.717540873949,43.2112552738719));
#22135=CARTESIAN_POINT('Ctrl Pts',(34.0498197571019,-32.5125154203786,43.2761866282037));
#22136=CARTESIAN_POINT('Ctrl Pts',(34.0544840782063,-31.9981228849384,43.3040747194623));
#22137=CARTESIAN_POINT('Ctrl Pts',(34.0574728862044,-31.9989451473756,42.5459252805377));
#22138=CARTESIAN_POINT('Ctrl Pts',(34.057852200887,-31.9383561660562,42.5492225367172));
#22139=CARTESIAN_POINT('Ctrl Pts',(34.0279453325407,-31.1974556320969,42.5895630559699));
#22140=CARTESIAN_POINT('Ctrl Pts',(33.1311710515888,-29.8509388446871,42.6669468382959));
#22141=CARTESIAN_POINT('Ctrl Pts',(30.8080907702464,-29.8840214107802,42.7780766275156));
#22142=CARTESIAN_POINT('Ctrl Pts',(29.5758326618125,-31.8536249348858,42.8892064167354));
#22143=CARTESIAN_POINT('Ctrl Pts',(30.5621463276885,-33.9571891796694,43.0003362059551));
#22144=CARTESIAN_POINT('Ctrl Pts',(32.8643680232945,-34.2695551886057,43.1114659951748));
#22145=CARTESIAN_POINT('Ctrl Pts',(33.9775551442909,-32.9695959350558,43.1933290200357));
#22146=CARTESIAN_POINT('Ctrl Pts',(34.0565764003152,-32.1451415815839,43.2381487818233));
#22147=CARTESIAN_POINT('Ctrl Pts',(34.055253827614,-32.0018424470648,43.2459252805377));
#22148=CARTESIAN_POINT('Origin',(32.,-32.,39.4540747194623));
#22149=CARTESIAN_POINT('',(34.0520872241698,-31.9988339725263,41.8459252805377));
#22150=CARTESIAN_POINT('',(34.056362032224,-32.0016080177294,41.9040747194623));
#22151=CARTESIAN_POINT('',(34.05475,-31.9999999999998,39.4540747194623));
#22152=CARTESIAN_POINT('Ctrl Pts',(34.056362032224,-32.0016080177294,41.9040747194623));
#22153=CARTESIAN_POINT('Ctrl Pts',(34.0514108335821,-31.4255899016838,41.9353774010647));
#22154=CARTESIAN_POINT('Ctrl Pts',(33.4988294221162,-30.1595906875508,42.0037233457404));
#22155=CARTESIAN_POINT('Ctrl Pts',(31.3531125199586,-29.6591578453596,42.1091125534892));
#22156=CARTESIAN_POINT('Ctrl Pts',(29.6825424522475,-31.2737738490384,42.220242342709));
#22157=CARTESIAN_POINT('Ctrl Pts',(30.1328842664196,-33.553027071776,42.3313721319287));
#22158=CARTESIAN_POINT('Ctrl Pts',(32.2919902196474,-34.4109652846105,42.4425019211484));
#22159=CARTESIAN_POINT('Ctrl Pts',(33.8394914966062,-33.3078912260223,42.5334027836596));
#22160=CARTESIAN_POINT('Ctrl Pts',(34.052221589152,-32.3117796033549,42.5872603830976));
#22161=CARTESIAN_POINT('Ctrl Pts',(34.0515269223438,-32.0005123640606,42.6040747194623));
#22162=CARTESIAN_POINT('Ctrl Pts',(34.0520872241698,-31.9988339725263,41.8459252805377));
#22163=CARTESIAN_POINT('Ctrl Pts',(34.053468796887,-31.732976645908,41.860296291611));
#22164=CARTESIAN_POINT('Ctrl Pts',(33.8819549522473,-30.7835444255121,41.9117105657577));
#22165=CARTESIAN_POINT('Ctrl Pts',(32.4498627695247,-29.6134582253175,42.0001681029775));
#22166=CARTESIAN_POINT('Ctrl Pts',(30.2390335714705,-30.327572605785,42.1112978921973));
#22167=CARTESIAN_POINT('Ctrl Pts',(29.6398080047623,-32.5722924533201,42.222427681417));
#22168=CARTESIAN_POINT('Ctrl Pts',(31.200611501379,-34.2932473343971,42.3335574706367));
#22169=CARTESIAN_POINT('Ctrl Pts',(33.4249871850401,-33.9266610466994,42.441390003677));
#22170=CARTESIAN_POINT('Ctrl Pts',(34.0535907626447,-32.6190474597171,42.5121792736439));
#22171=CARTESIAN_POINT('Ctrl Pts',(34.0574728862044,-31.9989451473756,42.5459252805377));
#22172=CARTESIAN_POINT('Origin',(32.,-32.,39.4540747194623));
#22173=CARTESIAN_POINT('',(34.0526762468981,-32.0023611642388,41.1459252805377));
#22174=CARTESIAN_POINT('',(34.0565678057143,-31.9985073856871,41.2040747194623));
#22175=CARTESIAN_POINT('',(34.05475,-31.9999999999998,39.4540747194623));
#22176=CARTESIAN_POINT('',(32.5301702171886,-33.9851743256717,41.));
#22177=CARTESIAN_POINT('Ctrl Pts',(32.5301702171886,-33.9851743256717,41.));
#22178=CARTESIAN_POINT('Ctrl Pts',(33.1902397907527,-33.8088929660699,41.0370432630732));
#22179=CARTESIAN_POINT('Ctrl Pts',(33.9249254184578,-33.112877718512,41.0856850232525));
#22180=CARTESIAN_POINT('Ctrl Pts',(34.0542946290731,-32.2166573957683,41.1343267834317));
#22181=CARTESIAN_POINT('Ctrl Pts',(34.0526762468981,-32.0023611642388,41.1459252805377));
#22182=CARTESIAN_POINT('',(31.4686978381225,-33.9887332741258,41.));
#22183=CARTESIAN_POINT('Origin',(32.,-32.,41.));
#22184=CARTESIAN_POINT('Ctrl Pts',(31.4686972148566,-33.9887352337366,41.));
#22185=CARTESIAN_POINT('Ctrl Pts',(32.1131669671016,-34.1600186174424,41.0363148168372));
#22186=CARTESIAN_POINT('Ctrl Pts',(33.4928784097068,-33.8407638650999,41.1043397233247));
#22187=CARTESIAN_POINT('Ctrl Pts',(34.051713710007,-32.5817335385731,41.1723646298121));
#22188=CARTESIAN_POINT('Ctrl Pts',(34.0565678057143,-31.9985073856871,41.2040747194623));
#22189=CARTESIAN_POINT('Origin',(32.,32.,48.));
#22190=CARTESIAN_POINT('',(33.6684806121724,32.0006140895871,53.3285196366098));
#22191=CARTESIAN_POINT('',(33.6648118697033,32.0014849556936,53.5214803633902));
#22192=CARTESIAN_POINT('',(33.666,32.,48.));
#22193=CARTESIAN_POINT('',(31.3249228143251,30.4769022377466,54.));
#22194=CARTESIAN_POINT('Ctrl Pts',(33.6648118697033,32.0014849556936,53.5214803633902));
#22195=CARTESIAN_POINT('Ctrl Pts',(33.6661630022499,32.1712284034164,53.5328138566339));
#22196=CARTESIAN_POINT('Ctrl Pts',(33.6422867953324,32.3405891079999,53.5441473498775));
#22197=CARTESIAN_POINT('Ctrl Pts',(33.591605099642,32.5014829336479,53.5554808431211));
#22198=CARTESIAN_POINT('Ctrl Pts',(33.4259531381418,33.0273607175068,53.5925241061943));
#22199=CARTESIAN_POINT('Ctrl Pts',(32.9739396808446,33.4627873203686,53.6295673692676));
#22200=CARTESIAN_POINT('Ctrl Pts',(32.4421423739696,33.6090004012271,53.6666106323408));
#22201=CARTESIAN_POINT('Ctrl Pts',(31.9103450670946,33.7552134820855,53.7036538954141));
#22202=CARTESIAN_POINT('Ctrl Pts',(31.2987639106417,33.6122130409406,53.7406971584873));
#22203=CARTESIAN_POINT('Ctrl Pts',(30.8877751036362,33.2444452260279,53.7777404215606));
#22204=CARTESIAN_POINT('Ctrl Pts',(30.4767862966307,32.8766774111153,53.8147836846338));
#22205=CARTESIAN_POINT('Ctrl Pts',(30.2663898390726,32.2841422224349,53.851826947707));
#22206=CARTESIAN_POINT('Ctrl Pts',(30.3518166376656,31.7403141445124,53.8888702107803));
#22207=CARTESIAN_POINT('Ctrl Pts',(30.4372434362585,31.1964860665899,53.9259134738535));
#22208=CARTESIAN_POINT('Ctrl Pts',(30.8184934910026,30.7013650994253,53.9629567369268));
#22209=CARTESIAN_POINT('Ctrl Pts',(31.3249228143251,30.4769022377466,54.));
#22210=CARTESIAN_POINT('',(33.666,32.,54.));
#22211=CARTESIAN_POINT('Origin',(32.,32.,54.));
#22212=CARTESIAN_POINT('',(33.666,32.,55.));
#22213=CARTESIAN_POINT('',(33.666,32.,48.));
#22214=CARTESIAN_POINT('Origin',(32.,32.,55.));
#22215=CARTESIAN_POINT('',(33.6146716715671,31.5775323837617,54.));
#22216=CARTESIAN_POINT('Origin',(32.,32.,54.));
#22217=CARTESIAN_POINT('Ctrl Pts',(33.614673303851,31.5775320375437,54.));
#22218=CARTESIAN_POINT('Ctrl Pts',(33.477140483944,31.0546378042632,53.9636851831628));
#22219=CARTESIAN_POINT('Ctrl Pts',(33.061847656895,30.6037761189473,53.9273703663256));
#22220=CARTESIAN_POINT('Ctrl Pts',(32.5515252260834,30.4251374099372,53.8910555494883));
#22221=CARTESIAN_POINT('Ctrl Pts',(32.0309661346949,30.2429153510298,53.8540122864151));
#22222=CARTESIAN_POINT('Ctrl Pts',(31.411526766352,30.3439469543993,53.8169690233418));
#22223=CARTESIAN_POINT('Ctrl Pts',(30.9761676297192,30.6822522118738,53.7799257602686));
#22224=CARTESIAN_POINT('Ctrl Pts',(30.5408084930864,31.0205574693483,53.7428824971953));
#22225=CARTESIAN_POINT('Ctrl Pts',(30.2895295881637,31.5961363809279,53.7058392341221));
#22226=CARTESIAN_POINT('Ctrl Pts',(30.3375623462193,32.1454810048324,53.6687959710489));
#22227=CARTESIAN_POINT('Ctrl Pts',(30.3855951042748,32.6948256287369,53.6317527079756));
#22228=CARTESIAN_POINT('Ctrl Pts',(30.7329395253087,33.2179359649664,53.5947094449023));
#22229=CARTESIAN_POINT('Ctrl Pts',(31.2205276954254,33.4755032093286,53.5576661818291));
#22230=CARTESIAN_POINT('Ctrl Pts',(31.7081158655422,33.7330704536908,53.5206229187558));
#22231=CARTESIAN_POINT('Ctrl Pts',(32.3359477847419,33.7250946061857,53.4835796556826));
#22232=CARTESIAN_POINT('Ctrl Pts',(32.8167941016275,33.4551932266985,53.4465363926094));
#22233=CARTESIAN_POINT('Ctrl Pts',(33.297640418513,33.1852918472114,53.4094931295362));
#22234=CARTESIAN_POINT('Ctrl Pts',(33.6315011330843,32.6534649357421,53.3724498664629));
#22235=CARTESIAN_POINT('Ctrl Pts',(33.6655715042332,32.1030898398486,53.3354066033897));
#22236=CARTESIAN_POINT('Ctrl Pts',(33.667682922926,32.0689818384882,53.3331109477964));
#22237=CARTESIAN_POINT('Ctrl Pts',(33.6686429776493,32.0348026016404,53.3308152922031));
#22238=CARTESIAN_POINT('Ctrl Pts',(33.6684806121724,32.0006140895871,53.3285196366098));
#22239=CARTESIAN_POINT('Origin',(32.,32.,48.));
#22240=CARTESIAN_POINT('',(33.6641301442348,32.00113043568,52.6285196366098));
#22241=CARTESIAN_POINT('',(33.6637770221358,31.9991035482978,52.8214803633902));
#22242=CARTESIAN_POINT('',(33.666,32.,48.));
#22243=CARTESIAN_POINT('Ctrl Pts',(33.6637770221358,31.9991035482978,52.8214803633902));
#22244=CARTESIAN_POINT('Ctrl Pts',(33.6621336119821,32.3352311296541,52.8438876115277));
#22245=CARTESIAN_POINT('Ctrl Pts',(33.5633565172328,32.6722466375241,52.8662948596652));
#22246=CARTESIAN_POINT('Ctrl Pts',(33.3740882433209,32.9469019105991,52.8887021078027));
#22247=CARTESIAN_POINT('Ctrl Pts',(33.0611933077665,33.400957110619,52.9257453708759));
#22248=CARTESIAN_POINT('Ctrl Pts',(32.5009849585214,33.6845810853147,52.9627886339492));
#22249=CARTESIAN_POINT('Ctrl Pts',(31.9498071626783,33.6679970783992,52.9998318970225));
#22250=CARTESIAN_POINT('Ctrl Pts',(31.3986293668351,33.6514130714837,53.0368751600957));
#22251=CARTESIAN_POINT('Ctrl Pts',(30.856482124394,33.3346210829571,53.073918423169));
#22252=CARTESIAN_POINT('Ctrl Pts',(30.5714576575436,32.862567499063,53.1109616862422));
#22253=CARTESIAN_POINT('Ctrl Pts',(30.2864331906931,32.3905139151689,53.1480049493154));
#22254=CARTESIAN_POINT('Ctrl Pts',(30.2585314994335,31.7631987359073,53.1850482123887));
#22255=CARTESIAN_POINT('Ctrl Pts',(30.5005032533944,31.2677094825492,53.2220914754619));
#22256=CARTESIAN_POINT('Ctrl Pts',(30.7424750073553,30.7722202291911,53.2591347385351));
#22257=CARTESIAN_POINT('Ctrl Pts',(31.2543202065367,30.4085569017365,53.2961780016084));
#22258=CARTESIAN_POINT('Ctrl Pts',(31.8018549039325,30.3430675123084,53.3332212646817));
#22259=CARTESIAN_POINT('Ctrl Pts',(32.3493896013283,30.2775781228804,53.3702645277549));
#22260=CARTESIAN_POINT('Ctrl Pts',(32.9326137969385,30.510262671479,53.4073077908281));
#22261=CARTESIAN_POINT('Ctrl Pts',(33.284580661892,30.9347694282061,53.4443510539014));
#22262=CARTESIAN_POINT('Ctrl Pts',(33.5288622487411,31.2293971175917,53.470060823731));
#22263=CARTESIAN_POINT('Ctrl Pts',(33.6617468564691,31.6164258325067,53.4957705935606));
#22264=CARTESIAN_POINT('Ctrl Pts',(33.6648118697033,32.0014849556936,53.5214803633902));
#22265=CARTESIAN_POINT('Ctrl Pts',(33.6684806121724,32.0006140895871,53.3285196366098));
#22266=CARTESIAN_POINT('Ctrl Pts',(33.6660230083945,31.4831283654114,53.2937720291298));
#22267=CARTESIAN_POINT('Ctrl Pts',(33.4064122708611,30.963517636581,53.2590244216499));
#22268=CARTESIAN_POINT('Ctrl Pts',(32.9900197135209,30.6566480056464,53.2242768141699));
#22269=CARTESIAN_POINT('Ctrl Pts',(32.5461175239329,30.3295045476556,53.1872335510967));
#22270=CARTESIAN_POINT('Ctrl Pts',(31.9240331170303,30.2441409119919,53.1501902880235));
#22271=CARTESIAN_POINT('Ctrl Pts',(31.4084208079463,30.4396231782327,53.1131470249502));
#22272=CARTESIAN_POINT('Ctrl Pts',(30.8928084988622,30.6351054444736,53.076103761877));
#22273=CARTESIAN_POINT('Ctrl Pts',(30.4836682875968,31.1114336126191,53.0390604988037));
#22274=CARTESIAN_POINT('Ctrl Pts',(30.3682246262316,31.650640403094,53.0020172357305));
#22275=CARTESIAN_POINT('Ctrl Pts',(30.2527809648664,32.1898471935689,52.9649739726572));
#22276=CARTESIAN_POINT('Ctrl Pts',(30.4310338534015,32.7919326063733,52.927930709584));
#22277=CARTESIAN_POINT('Ctrl Pts',(30.8214136605767,33.1813866783119,52.8908874465107));
#22278=CARTESIAN_POINT('Ctrl Pts',(31.2117934677519,33.5708407502506,52.8538441834375));
#22279=CARTESIAN_POINT('Ctrl Pts',(31.8143001935672,33.7476634813236,52.8168009203643));
#22280=CARTESIAN_POINT('Ctrl Pts',(32.3532310758874,33.6309412146398,52.779757657291));
#22281=CARTESIAN_POINT('Ctrl Pts',(32.8921619582076,33.514218947956,52.7427143942178));
#22282=CARTESIAN_POINT('Ctrl Pts',(33.3675169970328,33.1039516835154,52.7056711311445));
#22283=CARTESIAN_POINT('Ctrl Pts',(33.5617757744068,32.5878757666476,52.6686278680713));
#22284=CARTESIAN_POINT('Ctrl Pts',(33.6318863726636,32.4016170463641,52.6552584575841));
#22285=CARTESIAN_POINT('Ctrl Pts',(33.6653817959804,32.2015758506439,52.641889047097));
#22286=CARTESIAN_POINT('Ctrl Pts',(33.6641301442348,32.00113043568,52.6285196366098));
#22287=CARTESIAN_POINT('Origin',(32.,32.,48.));
#22288=CARTESIAN_POINT('',(33.6643836268795,31.9987501844045,51.9285196366098));
#22289=CARTESIAN_POINT('',(33.6681252089806,31.9990863473496,52.1214803633902));
#22290=CARTESIAN_POINT('',(33.666,32.,48.));
#22291=CARTESIAN_POINT('Ctrl Pts',(33.6681252089806,31.9990863473496,52.1214803633902));
#22292=CARTESIAN_POINT('Ctrl Pts',(33.6648306921651,32.4979846701634,52.1549613664216));
#22293=CARTESIAN_POINT('Ctrl Pts',(33.4261511788098,32.999617402672,52.188442369453));
#22294=CARTESIAN_POINT('Ctrl Pts',(33.0352551287758,33.3088117148578,52.2219233724844));
#22295=CARTESIAN_POINT('Ctrl Pts',(32.6027691246341,33.6509032058539,52.2589666355576));
#22296=CARTESIAN_POINT('Ctrl Pts',(31.983952861432,33.7574283024602,52.2960098986309));
#22297=CARTESIAN_POINT('Ctrl Pts',(31.461973233789,33.5796418315865,52.3330531617041));
#22298=CARTESIAN_POINT('Ctrl Pts',(30.9399936061459,33.4018553607128,52.3700964247774));
#22299=CARTESIAN_POINT('Ctrl Pts',(30.5148506140619,32.9397573223592,52.4071396878506));
#22300=CARTESIAN_POINT('Ctrl Pts',(30.3810875280695,32.4048010089502,52.4441829509238));
#22301=CARTESIAN_POINT('Ctrl Pts',(30.2473244420771,31.8698446955412,52.481226213997));
#22302=CARTESIAN_POINT('Ctrl Pts',(30.4049412621763,31.2620301070768,52.5182694770704));
#22303=CARTESIAN_POINT('Ctrl Pts',(30.7818131038358,30.859490426737,52.5553127401436));
#22304=CARTESIAN_POINT('Ctrl Pts',(31.1586849454953,30.4569507463972,52.5923560032168));
#22305=CARTESIAN_POINT('Ctrl Pts',(31.7548118087151,30.2596859741819,52.62939926629));
#22306=CARTESIAN_POINT('Ctrl Pts',(32.297409832103,30.357962364395,52.6664425293633));
#22307=CARTESIAN_POINT('Ctrl Pts',(32.8400078554909,30.4562387546082,52.7034857924365));
#22308=CARTESIAN_POINT('Ctrl Pts',(33.3290770390468,30.8500563072498,52.7405290555098));
#22309=CARTESIAN_POINT('Ctrl Pts',(33.5408208698929,31.3592082962425,52.7775723185831));
#22310=CARTESIAN_POINT('Ctrl Pts',(33.6244821246988,31.5603772942523,52.7922083335188));
#22311=CARTESIAN_POINT('Ctrl Pts',(33.6648504683442,31.7795510057075,52.8068443484545));
#22312=CARTESIAN_POINT('Ctrl Pts',(33.6637770221358,31.9991035482978,52.8214803633902));
#22313=CARTESIAN_POINT('Ctrl Pts',(33.6641301442348,32.00113043568,52.6285196366098));
#22314=CARTESIAN_POINT('Ctrl Pts',(33.6619137848118,31.6461921824217,52.6048457840238));
#22315=CARTESIAN_POINT('Ctrl Pts',(33.5507463265447,31.2899864805881,52.5811719314377));
#22316=CARTESIAN_POINT('Ctrl Pts',(33.3409999515945,31.0067929294096,52.5574980788516));
#22317=CARTESIAN_POINT('Ctrl Pts',(33.0128028354855,30.5636705783342,52.5204548157784));
#22318=CARTESIAN_POINT('Ctrl Pts',(32.4432460873448,30.2993104454786,52.4834115527051));
#22319=CARTESIAN_POINT('Ctrl Pts',(31.8929556516761,30.3346823630194,52.4463682896318));
#22320=CARTESIAN_POINT('Ctrl Pts',(31.3426652160074,30.3700542805602,52.4093250265586));
#22321=CARTESIAN_POINT('Ctrl Pts',(30.8116410928108,30.7051582484975,52.3722817634854));
#22322=CARTESIAN_POINT('Ctrl Pts',(30.5428771097717,31.1866524733684,52.3352385004122));
#22323=CARTESIAN_POINT('Ctrl Pts',(30.2741131267324,31.6681466982393,52.2981952373389));
#22324=CARTESIAN_POINT('Ctrl Pts',(30.2676092838506,32.2960311800439,52.2611519742656));
#22325=CARTESIAN_POINT('Ctrl Pts',(30.5263416698789,32.7829894020285,52.2241087111924));
#22326=CARTESIAN_POINT('Ctrl Pts',(30.7850740559072,33.2699476240131,52.1870654481191));
#22327=CARTESIAN_POINT('Ctrl Pts',(31.3090426708456,33.6159795861778,52.1500221850459));
#22328=CARTESIAN_POINT('Ctrl Pts',(31.8584823350187,33.662742930047,52.1129789219727));
#22329=CARTESIAN_POINT('Ctrl Pts',(32.4079219991918,33.7095062739161,52.0759356588994));
#22330=CARTESIAN_POINT('Ctrl Pts',(32.9828327125997,33.4570009994898,52.0388923958262));
#22331=CARTESIAN_POINT('Ctrl Pts',(33.3201384413117,33.0207721556727,52.0018491327529));
#22332=CARTESIAN_POINT('Ctrl Pts',(33.542711158369,32.7329245718267,51.9774059673719));
#22333=CARTESIAN_POINT('Ctrl Pts',(33.6618287603767,32.3650822730844,51.9529628019908));
#22334=CARTESIAN_POINT('Ctrl Pts',(33.6643836268795,31.9987501844045,51.9285196366098));
#22335=CARTESIAN_POINT('Origin',(32.,32.,48.));
#22336=CARTESIAN_POINT('',(33.6686262728084,31.9995820848651,51.2285196366098));
#22337=CARTESIAN_POINT('',(33.6665286630119,32.001478985866,51.4214803633902));
#22338=CARTESIAN_POINT('',(33.666,32.,48.));
#22339=CARTESIAN_POINT('Ctrl Pts',(33.6665286630119,32.001478985866,51.4214803633902));
#22340=CARTESIAN_POINT('Ctrl Pts',(33.6675619157926,32.1136863591203,51.4289918582423));
#22341=CARTESIAN_POINT('Ctrl Pts',(33.6571969840449,32.2257039247924,51.4365033530943));
#22342=CARTESIAN_POINT('Ctrl Pts',(33.6347339453088,32.3352404902405,51.4440148479463));
#22343=CARTESIAN_POINT('Ctrl Pts',(33.5239564942531,32.8754248197198,51.4810581110195));
#22344=CARTESIAN_POINT('Ctrl Pts',(33.1189516224042,33.3552709245807,51.5181013740928));
#22345=CARTESIAN_POINT('Ctrl Pts',(32.6050473636773,33.5552038279757,51.555144637166));
#22346=CARTESIAN_POINT('Ctrl Pts',(32.0911431049504,33.7551367313708,51.5921879002392));
#22347=CARTESIAN_POINT('Ctrl Pts',(31.4683394593454,33.6751564332998,51.6292311633125));
#22348=CARTESIAN_POINT('Ctrl Pts',(31.0216279968823,33.351861486703,51.6662744263857));
#22349=CARTESIAN_POINT('Ctrl Pts',(30.5749165344193,33.0285665401062,51.703317689459));
#22350=CARTESIAN_POINT('Ctrl Pts',(30.3042972550983,32.4619569449836,51.7403609525322));
#22351=CARTESIAN_POINT('Ctrl Pts',(30.3336040761335,31.9113101753598,51.7774042156055));
#22352=CARTESIAN_POINT('Ctrl Pts',(30.3629108971687,31.3606634057361,51.8144474786787));
#22353=CARTESIAN_POINT('Ctrl Pts',(30.6921438185601,30.8259794616112,51.851490741752));
#22354=CARTESIAN_POINT('Ctrl Pts',(31.1706476359806,30.5519268253061,51.8885340048252));
#22355=CARTESIAN_POINT('Ctrl Pts',(31.6491514534012,30.277874189001,51.9255772678984));
#22356=CARTESIAN_POINT('Ctrl Pts',(32.2769261668508,30.2644528605156,51.9626205309717));
#22357=CARTESIAN_POINT('Ctrl Pts',(32.7667054807056,30.5178043497829,51.9996637940449));
#22358=CARTESIAN_POINT('Ctrl Pts',(33.2564847945603,30.7711558390502,52.0367070571182));
#22359=CARTESIAN_POINT('Ctrl Pts',(33.6082687088201,31.2912801460702,52.0737503201914));
#22360=CARTESIAN_POINT('Ctrl Pts',(33.6610827934094,31.8401712422731,52.1107935832647));
#22361=CARTESIAN_POINT('Ctrl Pts',(33.6661616522239,31.8929552752419,52.1143558433065));
#22362=CARTESIAN_POINT('Ctrl Pts',(33.6684757338916,31.9460053342557,52.1179181033484));
#22363=CARTESIAN_POINT('Ctrl Pts',(33.6681252089806,31.9990863473496,52.1214803633902));
#22364=CARTESIAN_POINT('Ctrl Pts',(33.6643836268795,31.9987501844045,51.9285196366098));
#22365=CARTESIAN_POINT('Ctrl Pts',(33.6657006235542,31.8099112990475,51.9159195389176));
#22366=CARTESIAN_POINT('Ctrl Pts',(33.6360439504949,31.6214737147367,51.9033194412254));
#22367=CARTESIAN_POINT('Ctrl Pts',(33.5736181579473,31.444601776518,51.8907193435332));
#22368=CARTESIAN_POINT('Ctrl Pts',(33.390091401855,30.9246126543882,51.85367608046));
#22369=CARTESIAN_POINT('Ctrl Pts',(32.9233371456542,30.5045868233367,51.8166328173867));
#22370=CARTESIAN_POINT('Ctrl Pts',(32.3869396038679,30.3767258273003,51.7795895543135));
#22371=CARTESIAN_POINT('Ctrl Pts',(31.8505420620816,30.248864831264,51.7425462912403));
#22372=CARTESIAN_POINT('Ctrl Pts',(31.2445012347098,30.4131686702428,51.7055030281671));
#22373=CARTESIAN_POINT('Ctrl Pts',(30.8461381193723,30.7944527978433,51.6684597650938));
#22374=CARTESIAN_POINT('Ctrl Pts',(30.4477750040348,31.1757369254437,51.6314165020206));
#22375=CARTESIAN_POINT('Ctrl Pts',(30.2570896007315,31.7740013416658,51.5943732389473));
#22376=CARTESIAN_POINT('Ctrl Pts',(30.3613385154927,32.3154834938915,51.557329975874));
#22377=CARTESIAN_POINT('Ctrl Pts',(30.465587430254,32.8569656461173,51.5202867128007));
#22378=CARTESIAN_POINT('Ctrl Pts',(30.8647706630797,33.3416655343467,51.4832434497275));
#22379=CARTESIAN_POINT('Ctrl Pts',(31.3762241313992,33.5477871177545,51.4462001866543));
#22380=CARTESIAN_POINT('Ctrl Pts',(31.8876775997186,33.7539087011623,51.4091569235811));
#22381=CARTESIAN_POINT('Ctrl Pts',(32.5114013035318,33.6814519797484,51.3721136605078));
#22382=CARTESIAN_POINT('Ctrl Pts',(32.9619826578286,33.3635727564261,51.3350703974346));
#22383=CARTESIAN_POINT('Ctrl Pts',(33.3939981097689,33.0587915331986,51.2995534771596));
#22384=CARTESIAN_POINT('Ctrl Pts',(33.6668456803395,32.5283960695597,51.2640365568847));
#22385=CARTESIAN_POINT('Ctrl Pts',(33.6686262728084,31.9995820848651,51.2285196366098));
#22386=CARTESIAN_POINT('Origin',(32.,32.,48.));
#22387=CARTESIAN_POINT('',(33.6656098327441,32.0015149950249,50.5285196366098));
#22388=CARTESIAN_POINT('',(33.6632910880953,31.9999843288606,50.7214803633902));
#22389=CARTESIAN_POINT('',(33.666,32.,48.));
#22390=CARTESIAN_POINT('Ctrl Pts',(33.6632910880953,31.9999843288606,50.7214803633902));
#22391=CARTESIAN_POINT('Ctrl Pts',(33.6632676777025,32.2789818870778,50.7400656131361));
#22392=CARTESIAN_POINT('Ctrl Pts',(33.5968498065901,32.5579899196603,50.758650862882));
#22393=CARTESIAN_POINT('Ctrl Pts',(33.4640996397272,32.8007206148323,50.7772361126279));
#22394=CARTESIAN_POINT('Ctrl Pts',(33.1995081264924,33.2845202473439,50.8142793757012));
#22395=CARTESIAN_POINT('Ctrl Pts',(32.6714007905922,33.6242022625819,50.8513226387744));
#22396=CARTESIAN_POINT('Ctrl Pts',(32.1214366854017,33.6643300122038,50.8883659018477));
#22397=CARTESIAN_POINT('Ctrl Pts',(31.5714725802113,33.7044577618257,50.9254091649209));
#22398=CARTESIAN_POINT('Ctrl Pts',(30.9996517057307,33.4450312458314,50.9624524279942));
#22399=CARTESIAN_POINT('Ctrl Pts',(30.6676361935327,33.0047626312951,50.9994956910674));
#22400=CARTESIAN_POINT('Ctrl Pts',(30.3356206813347,32.5644940167588,51.0365389541406));
#22401=CARTESIAN_POINT('Ctrl Pts',(30.2434105314195,31.9433833036805,51.0735822172139));
#22402=CARTESIAN_POINT('Ctrl Pts',(30.4332006084387,31.4256473864592,51.1106254802871));
#22403=CARTESIAN_POINT('Ctrl Pts',(30.622990685458,30.907911469238,51.1476687433604));
#22404=CARTESIAN_POINT('Ctrl Pts',(31.0947809894117,30.4935503478738,51.1847120064336));
#22405=CARTESIAN_POINT('Ctrl Pts',(31.6326828353093,30.3721734248677,51.2217552695068));
#22406=CARTESIAN_POINT('Ctrl Pts',(32.1705846812069,30.2507965018616,51.2587985325801));
#22407=CARTESIAN_POINT('Ctrl Pts',(32.7745980690483,30.4224037772137,51.2958417956533));
#22408=CARTESIAN_POINT('Ctrl Pts',(33.1683297478377,30.8084686919385,51.3328850587266));
#22409=CARTESIAN_POINT('Ctrl Pts',(33.4822219839608,31.1162488018455,51.3624168269478));
#22410=CARTESIAN_POINT('Ctrl Pts',(33.6624663848319,31.5603308249559,51.391948595169));
#22411=CARTESIAN_POINT('Ctrl Pts',(33.6665286630119,32.001478985866,51.4214803633902));
#22412=CARTESIAN_POINT('Ctrl Pts',(33.6686262728084,31.9995820848651,51.2285196366098));
#22413=CARTESIAN_POINT('Ctrl Pts',(33.6687027939276,31.9768562569798,51.2269932938115));
#22414=CARTESIAN_POINT('Ctrl Pts',(33.668278692763,31.9541333498619,51.2254669510132));
#22415=CARTESIAN_POINT('Ctrl Pts',(33.6673450880065,31.9314313957851,51.2239406082149));
#22416=CARTESIAN_POINT('Ctrl Pts',(33.6446871591072,31.3804709836974,51.1868973451416));
#22417=CARTESIAN_POINT('Ctrl Pts',(33.3219322965282,30.8418518847528,51.1498540820684));
#22418=CARTESIAN_POINT('Ctrl Pts',(32.8467713752829,30.562043278107,51.1128108189951));
#22419=CARTESIAN_POINT('Ctrl Pts',(32.3716104540377,30.2822346714611,51.0757675559219));
#22420=CARTESIAN_POINT('Ctrl Pts',(31.7440434741263,30.261236557114,51.0387242928486));
#22421=CARTESIAN_POINT('Ctrl Pts',(31.2512416827347,30.5086575583237,51.0016810297754));
#22422=CARTESIAN_POINT('Ctrl Pts',(30.7584398913431,30.7560785595334,50.9646377667022));
#22423=CARTESIAN_POINT('Ctrl Pts',(30.4004032884713,31.2719186763,50.9275945036289));
#22424=CARTESIAN_POINT('Ctrl Pts',(30.3409674822114,31.8201322682224,50.8905512405557));
#22425=CARTESIAN_POINT('Ctrl Pts',(30.2815316759514,32.3683458601448,50.8535079774825));
#22426=CARTESIAN_POINT('Ctrl Pts',(30.5206966663033,32.9489329272231,50.8164647144092));
#22427=CARTESIAN_POINT('Ctrl Pts',(30.949021850505,33.2962199756621,50.7794214513359));
#22428=CARTESIAN_POINT('Ctrl Pts',(31.3773470347066,33.6435070241011,50.7423781882627));
#22429=CARTESIAN_POINT('Ctrl Pts',(31.994832412758,33.7574940539007,50.7053349251895));
#22430=CARTESIAN_POINT('Ctrl Pts',(32.5189200238354,33.5860212182949,50.6682916621162));
#22431=CARTESIAN_POINT('Ctrl Pts',(33.0430076349128,33.4145483826891,50.631248399043));
#22432=CARTESIAN_POINT('Ctrl Pts',(33.4736974790163,32.9576156816778,50.5942051359697));
#22433=CARTESIAN_POINT('Ctrl Pts',(33.6139082188038,32.4243130416287,50.5571618728965));
#22434=CARTESIAN_POINT('Ctrl Pts',(33.6500456862382,32.286861325614,50.5476144608009));
#22435=CARTESIAN_POINT('Ctrl Pts',(33.6668871327276,32.1443364875697,50.5380670487053));
#22436=CARTESIAN_POINT('Ctrl Pts',(33.6656098327441,32.0015149950249,50.5285196366098));
#22437=CARTESIAN_POINT('Origin',(32.,32.,48.));
#22438=CARTESIAN_POINT('',(33.6634354704477,31.999492392636,49.8285196366098));
#22439=CARTESIAN_POINT('',(33.6665861757579,31.9985292434177,50.0214803633902));
#22440=CARTESIAN_POINT('',(33.666,32.,48.));
#22441=CARTESIAN_POINT('Ctrl Pts',(33.6665861757579,31.9985292434177,50.0214803633902));
#22442=CARTESIAN_POINT('Ctrl Pts',(33.6625140098534,32.4415387358119,50.05113936803));
#22443=CARTESIAN_POINT('Ctrl Pts',(33.4805422963843,32.8875029945088,50.0807983726698));
#22444=CARTESIAN_POINT('Ctrl Pts',(33.1642404568284,33.1955272547085,50.1104573773096));
#22445=CARTESIAN_POINT('Ctrl Pts',(32.7691883505449,33.580240897061,50.1475006403828));
#22446=CARTESIAN_POINT('Ctrl Pts',(32.1645905457089,33.7497776897714,50.1845439034561));
#22447=CARTESIAN_POINT('Ctrl Pts',(31.6271077195186,33.6265585157702,50.2215871665293));
#22448=CARTESIAN_POINT('Ctrl Pts',(31.0896248933283,33.503339341769,50.2586304296025));
#22449=CARTESIAN_POINT('Ctrl Pts',(30.6192570457837,33.0873642010562,50.2956736926758));
#22450=CARTESIAN_POINT('Ctrl Pts',(30.4312419534573,32.5689810624913,50.332716955749));
#22451=CARTESIAN_POINT('Ctrl Pts',(30.2432268611308,32.0505979239263,50.3697602188223));
#22452=CARTESIAN_POINT('Ctrl Pts',(30.3375645240227,31.4298067875093,50.4068034818955));
#22453=CARTESIAN_POINT('Ctrl Pts',(30.6710865391189,30.9906783111636,50.4438467449688));
#22454=CARTESIAN_POINT('Ctrl Pts',(31.004608554215,30.5515498348179,50.480890008042));
#22455=CARTESIAN_POINT('Ctrl Pts',(31.5773149215154,30.2940840185436,50.5179332711152));
#22456=CARTESIAN_POINT('Ctrl Pts',(32.1271383127132,30.3360958238199,50.5549765341885));
#22457=CARTESIAN_POINT('Ctrl Pts',(32.6769617039109,30.3781076290962,50.5920197972617));
#22458=CARTESIAN_POINT('Ctrl Pts',(33.2039021190059,30.7195970559231,50.629063060335));
#22459=CARTESIAN_POINT('Ctrl Pts',(33.4668344812687,31.2043003942292,50.6661063234082));
#22460=CARTESIAN_POINT('Ctrl Pts',(33.5978491015855,31.4458196324391,50.6845643367355));
#22461=CARTESIAN_POINT('Ctrl Pts',(33.6633143382183,31.7228968149303,50.7030223500629));
#22462=CARTESIAN_POINT('Ctrl Pts',(33.6632910880953,31.9999843288606,50.7214803633902));
#22463=CARTESIAN_POINT('Ctrl Pts',(33.6656098327441,32.0015149950249,50.5285196366098));
#22464=CARTESIAN_POINT('Ctrl Pts',(33.6619313018869,31.5901995059569,50.5010237856321));
#22465=CARTESIAN_POINT('Ctrl Pts',(33.5079762466969,31.1764235703383,50.4735279346545));
#22466=CARTESIAN_POINT('Ctrl Pts',(33.2318651140294,30.874278170747,50.4460320836768));
#22467=CARTESIAN_POINT('Ctrl Pts',(32.8598796339962,30.467218519001,50.4089888206036));
#22468=CARTESIAN_POINT('Ctrl Pts',(32.2661770384583,30.2627717945958,50.3719455575303));
#22469=CARTESIAN_POINT('Ctrl Pts',(31.7224324159159,30.3544917100529,50.334902294457));
#22470=CARTESIAN_POINT('Ctrl Pts',(31.1786877933735,30.4462116255099,50.2978590313838));
#22471=CARTESIAN_POINT('Ctrl Pts',(30.6849011438266,30.8340981808292,50.2608157683105));
#22472=CARTESIAN_POINT('Ctrl Pts',(30.4670265606612,31.3406565915239,50.2237725052373));
#22473=CARTESIAN_POINT('Ctrl Pts',(30.2491519774957,31.8472150022187,50.1867292421641));
#22474=CARTESIAN_POINT('Ctrl Pts',(30.3071894607117,32.4724452682889,50.1496859790909));
#22475=CARTESIAN_POINT('Ctrl Pts',(30.6145813726846,32.9302454101508,50.1126427160176));
#22476=CARTESIAN_POINT('Ctrl Pts',(30.9219732846575,33.3880455520127,50.0755994529444));
#22477=CARTESIAN_POINT('Ctrl Pts',(31.4787196253875,33.6784155696663,50.0385561898711));
#22478=CARTESIAN_POINT('Ctrl Pts',(32.0300562881877,33.6684837174991,50.0015129267979));
#22479=CARTESIAN_POINT('Ctrl Pts',(32.5813929509879,33.6585518653319,49.9644696637246));
#22480=CARTESIAN_POINT('Ctrl Pts',(33.1273199358584,33.3483181433439,49.9274264006514));
#22481=CARTESIAN_POINT('Ctrl Pts',(33.4180240146883,32.8797438205446,49.8903831375781));
#22482=CARTESIAN_POINT('Ctrl Pts',(33.5798525593878,32.618898836713,49.8697619705887));
#22483=CARTESIAN_POINT('Ctrl Pts',(33.6625899967803,32.3089856338718,49.8491408035992));
#22484=CARTESIAN_POINT('Ctrl Pts',(33.6634354704477,31.999492392636,49.8285196366098));
#22485=CARTESIAN_POINT('Origin',(32.,32.,48.));
#22486=CARTESIAN_POINT('',(33.6674693445231,31.9987546512162,49.1285196366098));
#22487=CARTESIAN_POINT('',(33.6680840189634,32.0009409208067,49.3214803633902));
#22488=CARTESIAN_POINT('',(33.666,32.,48.));
#22489=CARTESIAN_POINT('Ctrl Pts',(33.6680840189634,32.0009409208067,49.3214803633902));
#22490=CARTESIAN_POINT('Ctrl Pts',(33.668455705338,32.0559214501504,49.3251698598506));
#22491=CARTESIAN_POINT('Ctrl Pts',(33.665972975259,32.1108680016515,49.3288593563111));
#22492=CARTESIAN_POINT('Ctrl Pts',(33.6605254320909,32.1655190244238,49.3325488527715));
#22493=CARTESIAN_POINT('Ctrl Pts',(33.6058310376544,32.7142259375462,49.3695921158448));
#22494=CARTESIAN_POINT('Ctrl Pts',(33.2522671445756,33.2331419261279,49.406635378918));
#22495=CARTESIAN_POINT('Ctrl Pts',(32.761622673207,33.4848138474987,49.4436786419912));
#22496=CARTESIAN_POINT('Ctrl Pts',(32.2709782018384,33.7364857688695,49.4807219050644));
#22497=CARTESIAN_POINT('Ctrl Pts',(31.6432531521799,33.7209136230295,49.5177651681377));
#22498=CARTESIAN_POINT('Ctrl Pts',(31.165691103258,33.4452231394785,49.5548084312109));
#22499=CARTESIAN_POINT('Ctrl Pts',(30.6881290543361,33.1695326559275,49.5918516942842));
#22500=CARTESIAN_POINT('Ctrl Pts',(30.3607300061507,32.6337238346656,49.6288949573574));
#22501=CARTESIAN_POINT('Ctrl Pts',(30.3333099879041,32.0829798869999,49.6659382204307));
#22502=CARTESIAN_POINT('Ctrl Pts',(30.3058899696574,31.5322359393341,49.7029814835039));
#22503=CARTESIAN_POINT('Ctrl Pts',(30.5784489813495,30.9665568652646,49.7400247465771));
#22504=CARTESIAN_POINT('Ctrl Pts',(31.0262654971198,30.6447943418184,49.7770680096504));
#22505=CARTESIAN_POINT('Ctrl Pts',(31.47408201289,30.3230318183722,49.8141112727237));
#22506=CARTESIAN_POINT('Ctrl Pts',(32.0971560327385,30.2451858455493,49.8511545357969));
#22507=CARTESIAN_POINT('Ctrl Pts',(32.6103722636605,30.4468783184113,49.8881977988701));
#22508=CARTESIAN_POINT('Ctrl Pts',(33.1235884945826,30.6485707912734,49.9252410619434));
#22509=CARTESIAN_POINT('Ctrl Pts',(33.5269469365783,31.1298017098203,49.9622843250166));
#22510=CARTESIAN_POINT('Ctrl Pts',(33.6358729537107,31.670362415091,49.9993275880898));
#22511=CARTESIAN_POINT('Ctrl Pts',(33.6575864258484,31.7781185795195,50.0067118465233));
#22512=CARTESIAN_POINT('Ctrl Pts',(33.6676000305986,31.8882323329164,50.0140961049567));
#22513=CARTESIAN_POINT('Ctrl Pts',(33.6665861757579,31.9985292434177,50.0214803633902));
#22514=CARTESIAN_POINT('Ctrl Pts',(33.6634354704477,31.999492392636,49.8285196366098));
#22515=CARTESIAN_POINT('Ctrl Pts',(33.6641087810226,31.7530210000391,49.812097540526));
#22516=CARTESIAN_POINT('Ctrl Pts',(33.6128456746512,31.5068159498285,49.7956754444422));
#22517=CARTESIAN_POINT('Ctrl Pts',(33.5082315407763,31.2858719194522,49.7792533483584));
#22518=CARTESIAN_POINT('Ctrl Pts',(33.2722538152451,30.7874892647698,49.7422100852852));
#22519=CARTESIAN_POINT('Ctrl Pts',(32.7648171913937,30.4176388790156,49.7051668222119));
#22520=CARTESIAN_POINT('Ctrl Pts',(32.2181219168358,30.3455622932806,49.6681235591387));
#22521=CARTESIAN_POINT('Ctrl Pts',(31.6714266422779,30.2734857075455,49.6310802960654));
#22522=CARTESIAN_POINT('Ctrl Pts',(31.0854727170135,30.4991829218297,49.5940370329922));
#22523=CARTESIAN_POINT('Ctrl Pts',(30.7283894800409,30.9193761146687,49.5569937699189));
#22524=CARTESIAN_POINT('Ctrl Pts',(30.3713062430682,31.3395693075078,49.5199505068457));
#22525=CARTESIAN_POINT('Ctrl Pts',(30.2430936943872,31.9542584789018,49.4829072437725));
#22526=CARTESIAN_POINT('Ctrl Pts',(30.4024212010707,32.482165197034,49.4458639806992));
#22527=CARTESIAN_POINT('Ctrl Pts',(30.5617487077542,33.0100719151663,49.408820717626));
#22528=CARTESIAN_POINT('Ctrl Pts',(31.0086162698022,33.4511961800368,49.3717774545528));
#22529=CARTESIAN_POINT('Ctrl Pts',(31.53853971386,33.6036819199376,49.3347341914795));
#22530=CARTESIAN_POINT('Ctrl Pts',(32.0684631579178,33.7561676598384,49.2976909284063));
#22531=CARTESIAN_POINT('Ctrl Pts',(32.6814424839853,33.6200148747694,49.260647665333));
#22532=CARTESIAN_POINT('Ctrl Pts',(33.0969816761962,33.2575263409205,49.2236044022598));
#22533=CARTESIAN_POINT('Ctrl Pts',(33.4525249287045,32.9473742427852,49.1919094803764));
#22534=CARTESIAN_POINT('Ctrl Pts',(33.6635254234559,32.4715253702981,49.1602145584931));
#22535=CARTESIAN_POINT('Ctrl Pts',(33.6674693445231,31.9987546512162,49.1285196366098));
#22536=CARTESIAN_POINT('Origin',(32.,32.,48.));
#22537=CARTESIAN_POINT('',(33.6673135177489,32.0013000734092,48.4285196366098));
#22538=CARTESIAN_POINT('',(33.6637467286262,32.0008713513863,48.6214803633902));
#22539=CARTESIAN_POINT('',(33.666,32.,48.));
#22540=CARTESIAN_POINT('Ctrl Pts',(33.6637467286262,32.0008713513863,48.6214803633902));
#22541=CARTESIAN_POINT('Ctrl Pts',(33.6647971283749,32.2223423012086,48.6362436147445));
#22542=CARTESIAN_POINT('Ctrl Pts',(33.623699448009,32.4434392475646,48.6510068660988));
#22543=CARTESIAN_POINT('Ctrl Pts',(33.5386160306917,32.6460665354014,48.6657701174531));
#22544=CARTESIAN_POINT('Ctrl Pts',(33.325128680567,33.154489493801,48.7028133805264));
#22545=CARTESIAN_POINT('Ctrl Pts',(32.8347136828381,33.5466302334562,48.7398566435996));
#22546=CARTESIAN_POINT('Ctrl Pts',(32.2917822813012,33.6430472781955,48.7768999066728));
#22547=CARTESIAN_POINT('Ctrl Pts',(31.7488508797643,33.7394643229347,48.8139431697461));
#22548=CARTESIAN_POINT('Ctrl Pts',(31.1534030744194,33.540157672758,48.8509864328194));
#22549=CARTESIAN_POINT('Ctrl Pts',(30.777912552311,33.1363289700909,48.8880296958926));
#22550=CARTESIAN_POINT('Ctrl Pts',(30.4024220302026,32.7325002674237,48.9250729589658));
#22551=CARTESIAN_POINT('Ctrl Pts',(30.2468887913307,32.1241495122662,48.962116222039));
#22552=CARTESIAN_POINT('Ctrl Pts',(30.3824840024592,31.5896547115336,48.9991594851123));
#22553=CARTESIAN_POINT('Ctrl Pts',(30.5180792135878,31.0551599108011,49.0362027481855));
#22554=CARTESIAN_POINT('Ctrl Pts',(30.9448028747168,30.5945210644937,49.0732460112588));
#22555=CARTESIAN_POINT('Ctrl Pts',(31.4673885523263,30.4185240109715,49.1102892743321));
#22556=CARTESIAN_POINT('Ctrl Pts',(31.9899742299358,30.2425269574493,49.1473325374053));
#22557=CARTESIAN_POINT('Ctrl Pts',(32.6084219240258,30.3511716967123,49.1843758004785));
#22558=CARTESIAN_POINT('Ctrl Pts',(33.0397333231737,30.6947429851753,49.2214190635517));
#22559=CARTESIAN_POINT('Ctrl Pts',(33.4280862529947,31.0040946896297,49.2547728301645));
#22560=CARTESIAN_POINT('Ctrl Pts',(33.6647239017427,31.503906226873,49.2881265967774));
#22561=CARTESIAN_POINT('Ctrl Pts',(33.6680840189634,32.0009409208067,49.3214803633902));
#22562=CARTESIAN_POINT('Ctrl Pts',(33.6674693445231,31.9987546512162,49.1285196366098));
#22563=CARTESIAN_POINT('Ctrl Pts',(33.6681348591936,31.9189772307336,49.1231712954199));
#22564=CARTESIAN_POINT('Ctrl Pts',(33.6629045043801,31.8392874596813,49.11782295423));
#22565=CARTESIAN_POINT('Ctrl Pts',(33.6514779047485,31.7604962919983,49.1124746130401));
#22566=CARTESIAN_POINT('Ctrl Pts',(33.572335882736,31.2147790595537,49.0754313499668));
#22567=CARTESIAN_POINT('Ctrl Pts',(33.1959527803567,30.7121688772935,49.0383880868935));
#22568=CARTESIAN_POINT('Ctrl Pts',(32.6945594644071,30.4826574393297,49.0013448238203));
#22569=CARTESIAN_POINT('Ctrl Pts',(32.1931661484575,30.2531460013658,48.9643015607471));
#22570=CARTESIAN_POINT('Ctrl Pts',(31.5667626189377,30.2967333076982,48.9272582976738));
#22571=CARTESIAN_POINT('Ctrl Pts',(31.1019877344241,30.5934740432916,48.8902150346006));
#22572=CARTESIAN_POINT('Ctrl Pts',(30.6372128499105,30.8902147788851,48.8531717715274));
#22573=CARTESIAN_POINT('Ctrl Pts',(30.3340666104031,31.4401089437394,48.8161285084541));
#22574=CARTESIAN_POINT('Ctrl Pts',(30.3312670913586,31.9915279496943,48.7790852453808));
#22575=CARTESIAN_POINT('Ctrl Pts',(30.3284675723141,32.5429469556492,48.7420419823076));
#22576=CARTESIAN_POINT('Ctrl Pts',(30.6260147737323,33.0958908027046,48.7049987192344));
#22577=CARTESIAN_POINT('Ctrl Pts',(31.0877527096269,33.3973353846611,48.6679554561611));
#22578=CARTESIAN_POINT('Ctrl Pts',(31.5494906455215,33.6987799666177,48.6309121930879));
#22579=CARTESIAN_POINT('Ctrl Pts',(32.1754193158924,33.7487252834754,48.5938689300147));
#22580=CARTESIAN_POINT('Ctrl Pts',(32.6791171551348,33.5243166290574,48.5568256669414));
#22581=CARTESIAN_POINT('Ctrl Pts',(33.1828149943771,33.2999079746393,48.5197824038682));
#22582=CARTESIAN_POINT('Ctrl Pts',(33.564282002491,32.8011453489455,48.4827391407949));
#22583=CARTESIAN_POINT('Ctrl Pts',(33.6489609449821,32.2562598250658,48.4456958777217));
#22584=CARTESIAN_POINT('Ctrl Pts',(33.6620489382515,32.1720422160678,48.4399704640177));
#22585=CARTESIAN_POINT('Ctrl Pts',(33.6680470054324,32.0867227839946,48.4342450503138));
#22586=CARTESIAN_POINT('Ctrl Pts',(33.6673135177489,32.0013000734092,48.4285196366098));
#22587=CARTESIAN_POINT('Origin',(32.,32.,48.));
#22588=CARTESIAN_POINT('',(33.6633884534296,32.0004190051222,47.7285196366098));
#22589=CARTESIAN_POINT('',(33.6649068449334,31.9985848581839,47.9214803633902));
#22590=CARTESIAN_POINT('',(33.666,32.,48.));
#22591=CARTESIAN_POINT('Ctrl Pts',(33.6649068449334,31.9985848581839,47.9214803633902));
#22592=CARTESIAN_POINT('Ctrl Pts',(33.6617821224527,32.3854996191865,47.9473173696384));
#22593=CARTESIAN_POINT('Ctrl Pts',(33.5274209634318,32.7743714298488,47.9731543758866));
#22594=CARTESIAN_POINT('Ctrl Pts',(33.2809047599811,33.0695906945765,47.9989913821348));
#22595=CARTESIAN_POINT('Ctrl Pts',(32.9274673497593,33.4928550922606,48.036034645208));
#22596=CARTESIAN_POINT('Ctrl Pts',(32.3434864284141,33.7236093190898,48.0730779082812));
#22597=CARTESIAN_POINT('Ctrl Pts',(31.7961884990483,33.6562614920799,48.1101211713545));
#22598=CARTESIAN_POINT('Ctrl Pts',(31.2488905696825,33.5889136650699,48.1471644344277));
#22599=CARTESIAN_POINT('Ctrl Pts',(30.7382756322961,33.2234637842209,48.184207697501));
#22600=CARTESIAN_POINT('Ctrl Pts',(30.4979983135429,32.7271397334397,48.2212509605743));
#22601=CARTESIAN_POINT('Ctrl Pts',(30.2577209947897,32.2308156826585,48.2582942236475));
#22602=CARTESIAN_POINT('Ctrl Pts',(30.2877812946696,31.6036174619452,48.2953374867207));
#22603=CARTESIAN_POINT('Ctrl Pts',(30.574423782953,31.1325475762575,48.3323807497939));
#22604=CARTESIAN_POINT('Ctrl Pts',(30.8610662712363,30.6614776905698,48.3694240128672));
#22605=CARTESIAN_POINT('Ctrl Pts',(31.4042909479229,30.3465361399077,48.4064672759405));
#22606=CARTESIAN_POINT('Ctrl Pts',(31.9555211464742,30.3318384701547,48.4435105390137));
#22607=CARTESIAN_POINT('Ctrl Pts',(32.5067513450255,30.3171408004017,48.4805538020869));
#22608=CARTESIAN_POINT('Ctrl Pts',(33.0659870654415,30.6026870115578,48.5175970651601));
#22609=CARTESIAN_POINT('Ctrl Pts',(33.3773250743892,31.0578127057078,48.5546403282334));
#22610=CARTESIAN_POINT('Ctrl Pts',(33.5645821870844,31.3315522458558,48.5769203399523));
#22611=CARTESIAN_POINT('Ctrl Pts',(33.6621615142211,31.6666377033218,48.5992003516713));
#22612=CARTESIAN_POINT('Ctrl Pts',(33.6637467286262,32.0008713513863,48.6214803633902));
#22613=CARTESIAN_POINT('Ctrl Pts',(33.6673135177489,32.0013000734092,48.4285196366098));
#22614=CARTESIAN_POINT('Ctrl Pts',(33.6633013610779,31.5340402872771,48.3972017872405));
#22615=CARTESIAN_POINT('Ctrl Pts',(33.4578771286557,31.0636903473883,48.3658839378712));
#22616=CARTESIAN_POINT('Ctrl Pts',(33.1096935602187,30.7536768081961,48.334566088502));
#22617=CARTESIAN_POINT('Ctrl Pts',(32.6978563560956,30.3869877372719,48.2975228254287));
#22618=CARTESIAN_POINT('Ctrl Pts',(32.086291070981,30.2446180174893,48.2604795623555));
#22619=CARTESIAN_POINT('Ctrl Pts',(31.5548466632686,30.3917152606531,48.2234362992822));
#22620=CARTESIAN_POINT('Ctrl Pts',(31.0234022555563,30.5388125038169,48.186393036209));
#22621=CARTESIAN_POINT('Ctrl Pts',(30.5720787252461,30.9753767099272,48.1493497731357));
#22622=CARTESIAN_POINT('Ctrl Pts',(30.4073992726082,31.5016384654387,48.1123065100625));
#22623=CARTESIAN_POINT('Ctrl Pts',(30.2427198199703,32.0279002209502,48.0752632469893));
#22624=CARTESIAN_POINT('Ctrl Pts',(30.3646844450046,32.6438595258629,48.038219983916));
#22625=CARTESIAN_POINT('Ctrl Pts',(30.717482796621,33.067656742149,48.0011767208428));
#22626=CARTESIAN_POINT('Ctrl Pts',(31.0702811482375,33.4914539584351,47.9641334577695));
#22627=CARTESIAN_POINT('Ctrl Pts',(31.6539132264361,33.7230890860946,47.9270901946963));
#22628=CARTESIAN_POINT('Ctrl Pts',(32.2013121568464,33.6565671466998,47.890046931623));
#22629=CARTESIAN_POINT('Ctrl Pts',(32.7487110872566,33.5900452073049,47.8530036685498));
#22630=CARTESIAN_POINT('Ctrl Pts',(33.2598768698785,33.2253662008556,47.8159604054766));
#22631=CARTESIAN_POINT('Ctrl Pts',(33.5009028142653,32.7294052633136,47.7789171424033));
#22632=CARTESIAN_POINT('Ctrl Pts',(33.610208397529,32.5044863248485,47.7621179738055));
#22633=CARTESIAN_POINT('Ctrl Pts',(33.663956091105,32.2525674922054,47.7453188052076));
#22634=CARTESIAN_POINT('Ctrl Pts',(33.6633884534296,32.0004190051222,47.7285196366098));
#22635=CARTESIAN_POINT('Origin',(32.,32.,48.));
#22636=CARTESIAN_POINT('',(33.66577763495,31.9984781750094,47.0285196366098));
#22637=CARTESIAN_POINT('',(33.668753764066,31.9999631497191,47.2214803633902));
#22638=CARTESIAN_POINT('',(33.666,32.,48.));
#22639=CARTESIAN_POINT('Ctrl Pts',(33.6687533715572,31.9999631549716,47.2214803633902));
#22640=CARTESIAN_POINT('Ctrl Pts',(33.668574581605,32.5494177579999,47.2583911245323));
#22641=CARTESIAN_POINT('Ctrl Pts',(33.3706768371093,33.0990384969375,47.2953018856743));
#22642=CARTESIAN_POINT('Ctrl Pts',(32.9101378227849,33.3987102636369,47.3322126468164));
#22643=CARTESIAN_POINT('Ctrl Pts',(32.4479455694893,33.6994577894531,47.3692559098897));
#22644=CARTESIAN_POINT('Ctrl Pts',(31.8219422540236,33.7484585927198,47.4062991729629));
#22645=CARTESIAN_POINT('Ctrl Pts',(31.3185835991834,33.5232901715579,47.4433424360361));
#22646=CARTESIAN_POINT('Ctrl Pts',(30.8152249443432,33.2981217503961,47.4803856991094));
#22647=CARTESIAN_POINT('Ctrl Pts',(30.4345109501285,32.7987841048057,47.5174289621826));
#22648=CARTESIAN_POINT('Ctrl Pts',(30.3506542759561,32.2537714338632,47.5544722252559));
#22649=CARTESIAN_POINT('Ctrl Pts',(30.2667976017838,31.7087587629208,47.5915154883291));
#22650=CARTESIAN_POINT('Ctrl Pts',(30.4797982476539,31.1180710666263,47.6285587514024));
#22651=CARTESIAN_POINT('Ctrl Pts',(30.8921882729642,30.7520038319335,47.6656020144756));
#22652=CARTESIAN_POINT('Ctrl Pts',(31.3045782982745,30.3859365972407,47.7026452775488));
#22653=CARTESIAN_POINT('Ctrl Pts',(31.916357703025,30.2444898241495,47.7396885406221));
#22654=CARTESIAN_POINT('Ctrl Pts',(32.4475795488375,30.3923887890633,47.7767318036953));
#22655=CARTESIAN_POINT('Ctrl Pts',(32.9788013946501,30.5402877539772,47.8137750667686));
#22656=CARTESIAN_POINT('Ctrl Pts',(33.4294656815247,30.977532456896,47.8508183298418));
#22657=CARTESIAN_POINT('Ctrl Pts',(33.5933508754128,31.5040420926248,47.887861592915));
#22658=CARTESIAN_POINT('Ctrl Pts',(33.6429291096225,31.6633207767725,47.8990678497401));
#22659=CARTESIAN_POINT('Ctrl Pts',(33.6662621274414,31.8307687366275,47.9102741065651));
#22660=CARTESIAN_POINT('Ctrl Pts',(33.6649068449334,31.9985848581839,47.9214803633902));
#22661=CARTESIAN_POINT('Ctrl Pts',(33.6633884534296,32.0004190051222,47.7285196366098));
#22662=CARTESIAN_POINT('Ctrl Pts',(33.6627044129868,31.696563622958,47.7082755421344));
#22663=CARTESIAN_POINT('Ctrl Pts',(33.583144610912,31.3923747406851,47.688031447659));
#22664=CARTESIAN_POINT('Ctrl Pts',(33.4268834926819,31.1346995930135,47.6677873531836));
#22665=CARTESIAN_POINT('Ctrl Pts',(33.14095212056,30.6631977288903,47.6307440901104));
#22666=CARTESIAN_POINT('Ctrl Pts',(32.5982032701644,30.3474368692789,47.5937008270371));
#22667=CARTESIAN_POINT('Ctrl Pts',(32.0469958725032,30.3319074713953,47.5566575639639));
#22668=CARTESIAN_POINT('Ctrl Pts',(31.4957884748419,30.3163780735117,47.5196143008907));
#22669=CARTESIAN_POINT('Ctrl Pts',(30.9361225299148,30.6010801373561,47.4825710378174));
#22670=CARTESIAN_POINT('Ctrl Pts',(30.6240981394585,31.0557355422459,47.4455277747441));
#22671=CARTESIAN_POINT('Ctrl Pts',(30.3120737490021,31.5103909471357,47.4084845116709));
#22672=CARTESIAN_POINT('Ctrl Pts',(30.2476909130165,32.1349996930709,47.3714412485977));
#22673=CARTESIAN_POINT('Ctrl Pts',(30.4604108681471,32.6437442047115,47.3343979855245));
#22674=CARTESIAN_POINT('Ctrl Pts',(30.6731308232777,33.152488716352,47.2973547224512));
#22675=CARTESIAN_POINT('Ctrl Pts',(31.1629535695247,33.5453689936979,47.2603114593779));
#22676=CARTESIAN_POINT('Ctrl Pts',(31.7057388741586,33.6426051521403,47.2232681963047));
#22677=CARTESIAN_POINT('Ctrl Pts',(32.2485241787925,33.7398413105826,47.1862249332314));
#22678=CARTESIAN_POINT('Ctrl Pts',(32.8442720418133,33.5414333501214,47.1491816701582));
#22679=CARTESIAN_POINT('Ctrl Pts',(33.2203714714111,33.1381716776414,47.112138407085));
#22680=CARTESIAN_POINT('Ctrl Pts',(33.5033646463302,32.8347404782366,47.0842654835932));
#22681=CARTESIAN_POINT('Ctrl Pts',(33.6619995478179,32.4153273274213,47.0563925601015));
#22682=CARTESIAN_POINT('Ctrl Pts',(33.66577763495,31.9984781750094,47.0285196366098));
#22683=CARTESIAN_POINT('Origin',(32.,32.,48.));
#22684=CARTESIAN_POINT('',(33.6685588008505,32.0005167954687,46.3285196366098));
#22685=CARTESIAN_POINT('',(33.6650142123929,32.0014384754572,46.5214803633902));
#22686=CARTESIAN_POINT('',(33.666,32.,48.));
#22687=CARTESIAN_POINT('Ctrl Pts',(33.6650142123929,32.0014384754572,46.5214803633902));
#22688=CARTESIAN_POINT('Ctrl Pts',(33.6663656089876,32.1652593743191,46.5324216163529));
#22689=CARTESIAN_POINT('Ctrl Pts',(33.6441442932285,32.3287216649132,46.5433628693156));
#22690=CARTESIAN_POINT('Ctrl Pts',(33.5968494360195,32.4845752126874,46.5543041222783));
#22691=CARTESIAN_POINT('Ctrl Pts',(33.4367255595701,33.0122409188706,46.5913473853516));
#22692=CARTESIAN_POINT('Ctrl Pts',(32.9891929020642,33.4526904053733,46.6283906484248));
#22693=CARTESIAN_POINT('Ctrl Pts',(32.4590399809318,33.6043763754097,46.665433911498));
#22694=CARTESIAN_POINT('Ctrl Pts',(31.9288870597995,33.7560623454462,46.7024771745713));
#22695=CARTESIAN_POINT('Ctrl Pts',(31.3161138750406,33.6189847990163,46.7395204376445));
#22696=CARTESIAN_POINT('Ctrl Pts',(30.9011221133767,33.2558696780945,46.7765637007178));
#22697=CARTESIAN_POINT('Ctrl Pts',(30.4861303517127,32.8927545571726,46.813606963791));
#22698=CARTESIAN_POINT('Ctrl Pts',(30.2689200131437,32.3036018617586,46.8506502268643));
#22699=CARTESIAN_POINT('Ctrl Pts',(30.3488853708247,31.7580046707266,46.8876934899375));
#22700=CARTESIAN_POINT('Ctrl Pts',(30.4288507285058,31.2124074796946,46.9247367530107));
#22701=CARTESIAN_POINT('Ctrl Pts',(30.8059917824369,30.7103657930446,46.961780016084));
#22702=CARTESIAN_POINT('Ctrl Pts',(31.3077308313014,30.4816111643798,46.9988232791572));
#22703=CARTESIAN_POINT('Ctrl Pts',(31.809469880166,30.252856535715,47.0358665422305));
#22704=CARTESIAN_POINT('Ctrl Pts',(32.4358069239639,30.2973889650355,47.0729098053037));
#22705=CARTESIAN_POINT('Ctrl Pts',(32.9001335276246,30.5948306541513,47.109953068377));
#22706=CARTESIAN_POINT('Ctrl Pts',(33.3644601312852,30.892272343267,47.1469963314502));
#22707=CARTESIAN_POINT('Ctrl Pts',(33.6667762948085,31.4426232921781,47.1840395945234));
#22708=CARTESIAN_POINT('Ctrl Pts',(33.6687437810073,31.9940458908165,47.2210828575967));
#22709=CARTESIAN_POINT('Ctrl Pts',(33.6687508186088,31.996018302347,47.2212153595278));
#22710=CARTESIAN_POINT('Ctrl Pts',(33.6687540133758,31.9979907275889,47.221347861459));
#22711=CARTESIAN_POINT('Ctrl Pts',(33.6687533715572,31.9999631549716,47.2214803633902));
#22712=CARTESIAN_POINT('Ctrl Pts',(33.66577763495,31.9984781750094,47.0285196366098));
#22713=CARTESIAN_POINT('Ctrl Pts',(33.6670206456439,31.8613325941729,47.0193492970283));
#22714=CARTESIAN_POINT('Ctrl Pts',(33.6515012597471,31.724464552031,47.0101789574468));
#22715=CARTESIAN_POINT('Ctrl Pts',(33.6181333324057,31.592095826723,47.0010086178653));
#22716=CARTESIAN_POINT('Ctrl Pts',(33.4833447676279,31.0573970327836,46.963965354792));
#22717=CARTESIAN_POINT('Ctrl Pts',(33.0573166418977,30.5961148294036,46.9269220917188));
#22718=CARTESIAN_POINT('Ctrl Pts',(32.5349971155079,30.4193294516512,46.8898788286455));
#22719=CARTESIAN_POINT('Ctrl Pts',(32.0126775891181,30.2425440738987,46.8528355655723));
#22720=CARTESIAN_POINT('Ctrl Pts',(31.3940666620687,30.3502555217738,46.815792302499));
#22721=CARTESIAN_POINT('Ctrl Pts',(30.9622373402994,30.6931756207699,46.7787490394258));
#22722=CARTESIAN_POINT('Ctrl Pts',(30.5304080185301,31.0360957197659,46.7417057763526));
#22723=CARTESIAN_POINT('Ctrl Pts',(30.2853603020409,31.6142244698828,46.7046625132793));
#22724=CARTESIAN_POINT('Ctrl Pts',(30.3392266971815,32.1630132898397,46.6676192502061));
#22725=CARTESIAN_POINT('Ctrl Pts',(30.393093092322,32.7118021097967,46.6305759871328));
#22726=CARTESIAN_POINT('Ctrl Pts',(30.7458735990921,33.2312509995936,46.5935327240596));
#22727=CARTESIAN_POINT('Ctrl Pts',(31.2361377704666,33.4836629638538,46.5564894609863));
#22728=CARTESIAN_POINT('Ctrl Pts',(31.726401941841,33.736074928114,46.5194461979131));
#22729=CARTESIAN_POINT('Ctrl Pts',(32.3541497778197,33.7214499668374,46.4824029348399));
#22730=CARTESIAN_POINT('Ctrl Pts',(32.8321272724797,33.4464803830037,46.4453596717666));
#22731=CARTESIAN_POINT('Ctrl Pts',(33.3101047671398,33.17151079917,46.4083164086934));
#22732=CARTESIAN_POINT('Ctrl Pts',(33.6383119204811,32.6361965927792,46.3712731456201));
#22733=CARTESIAN_POINT('Ctrl Pts',(33.6665629187639,32.0854946420552,46.3342298825469));
#22734=CARTESIAN_POINT('Ctrl Pts',(33.6680145560729,32.0571976066811,46.3323264672345));
#22735=CARTESIAN_POINT('Ctrl Pts',(33.6686742275888,32.0288599434787,46.3304230519221));
#22736=CARTESIAN_POINT('Ctrl Pts',(33.6685588008505,32.0005167954687,46.3285196366098));
#22737=CARTESIAN_POINT('Origin',(32.,32.,48.));
#22738=CARTESIAN_POINT('',(33.664255890244,32.0011936369589,45.6285196366098));
#22739=CARTESIAN_POINT('',(33.6636859641007,31.9991832784139,45.8214803633902));
#22740=CARTESIAN_POINT('',(33.666,32.,48.));
#22741=CARTESIAN_POINT('Ctrl Pts',(33.6636859641007,31.9991832784139,45.8214803633902));
#22742=CARTESIAN_POINT('Ctrl Pts',(33.6622209772371,32.3294716616209,45.8434953712468));
#22743=CARTESIAN_POINT('Ctrl Pts',(33.5671083678426,32.660537694823,45.8655103791034));
#22744=CARTESIAN_POINT('Ctrl Pts',(33.3840134044156,32.932334786686,45.88752538696));
#22745=CARTESIAN_POINT('Ctrl Pts',(33.0759310752249,33.3896705842477,45.9245686500332));
#22746=CARTESIAN_POINT('Ctrl Pts',(32.5187472361758,33.6792002013809,45.9616119131064));
#22747=CARTESIAN_POINT('Ctrl Pts',(31.9674261908138,33.6684364551945,45.9986551761797));
#22748=CARTESIAN_POINT('Ctrl Pts',(31.4161051454517,33.657672709008,46.0356984392529));
#22749=CARTESIAN_POINT('Ctrl Pts',(30.8706468937767,33.3466155995018,46.0727417023262));
#22750=CARTESIAN_POINT('Ctrl Pts',(30.5806501741309,32.877603173349,46.1097849653994));
#22751=CARTESIAN_POINT('Ctrl Pts',(30.2906534544851,32.4085907471962,46.1468282284727));
#22752=CARTESIAN_POINT('Ctrl Pts',(30.2561182668687,31.7816230043967,46.1838714915459));
#22753=CARTESIAN_POINT('Ctrl Pts',(30.4928477258755,31.2835969844646,46.2209147546191));
#22754=CARTESIAN_POINT('Ctrl Pts',(30.7295771848824,30.7855709645325,46.2579580176924));
#22755=CARTESIAN_POINT('Ctrl Pts',(31.2375712905126,30.4164866674678,46.2950012807656));
#22756=CARTESIAN_POINT('Ctrl Pts',(31.784374694513,30.345235066331,46.3320445438389));
#22757=CARTESIAN_POINT('Ctrl Pts',(32.3311780985135,30.2739834651943,46.3690878069121));
#22758=CARTESIAN_POINT('Ctrl Pts',(32.9167908008843,30.5005645599854,46.4061310699854));
#22759=CARTESIAN_POINT('Ctrl Pts',(33.2732396043732,30.9212960703129,46.4431743330586));
#22760=CARTESIAN_POINT('Ctrl Pts',(33.5244061998796,31.2177585637675,46.4692763431691));
#22761=CARTESIAN_POINT('Ctrl Pts',(33.6617902518739,31.6106189986581,46.4953783532797));
#22762=CARTESIAN_POINT('Ctrl Pts',(33.6650142123929,32.0014384754572,46.5214803633902));
#22763=CARTESIAN_POINT('Ctrl Pts',(33.6685588008505,32.0005167954687,46.3285196366098));
#22764=CARTESIAN_POINT('Ctrl Pts',(33.666427853399,31.4772605730014,46.2933797888489));
#22765=CARTESIAN_POINT('Ctrl Pts',(33.4001233193856,30.9521349858584,46.258239941088));
#22766=CARTESIAN_POINT('Ctrl Pts',(32.9757782549176,30.6462651318486,46.2231000933272));
#22767=CARTESIAN_POINT('Ctrl Pts',(32.5284477495642,30.3238272674229,46.1860568302539));
#22768=CARTESIAN_POINT('Ctrl Pts',(31.9054918956329,30.2450412336288,46.1490135671807));
#22769=CARTESIAN_POINT('Ctrl Pts',(31.3919719140453,30.4459590923308,46.1119703041074));
#22770=CARTESIAN_POINT('Ctrl Pts',(30.8784519324577,30.6468769510328,46.0749270410342));
#22771=CARTESIAN_POINT('Ctrl Pts',(30.4743678232137,31.127498702231,46.037883777961));
#22772=CARTESIAN_POINT('Ctrl Pts',(30.3646262836486,31.66789443864,46.0008405148877));
#22773=CARTESIAN_POINT('Ctrl Pts',(30.2548847440835,32.208290175049,45.9637972518145));
#22774=CARTESIAN_POINT('Ctrl Pts',(30.4394857741973,32.8084598966689,45.9267539887412));
#22775=CARTESIAN_POINT('Ctrl Pts',(30.8339569435673,33.1937691931711,45.889710725668));
#22776=CARTESIAN_POINT('Ctrl Pts',(31.2284281129373,33.5790784896733,45.8526674625947));
#22777=CARTESIAN_POINT('Ctrl Pts',(31.8327694215635,33.7495273610579,45.8156241995215));
#22778=CARTESIAN_POINT('Ctrl Pts',(32.3704375635228,33.6271193279998,45.7785809364483));
#22779=CARTESIAN_POINT('Ctrl Pts',(32.9081057054821,33.5047112949417,45.741537673375));
#22780=CARTESIAN_POINT('Ctrl Pts',(33.3791006807746,33.0894463574409,45.7044944103018));
#22781=CARTESIAN_POINT('Ctrl Pts',(33.5678977425703,32.5713474992175,45.6674511472285));
#22782=CARTESIAN_POINT('Ctrl Pts',(33.6340380175379,32.3898446695792,45.6544739770223));
#22783=CARTESIAN_POINT('Ctrl Pts',(33.665544876609,32.1957213003327,45.641496806816));
#22784=CARTESIAN_POINT('Ctrl Pts',(33.664255890244,32.0011936369589,45.6285196366098));
#22785=CARTESIAN_POINT('Origin',(32.,32.,48.));
#22786=CARTESIAN_POINT('',(33.6642508883749,31.9988087175676,44.9285196366098));
#22787=CARTESIAN_POINT('',(33.6679951520813,31.9990039461198,45.1214803633902));
#22788=CARTESIAN_POINT('',(33.666,32.,48.));
#22789=CARTESIAN_POINT('Ctrl Pts',(33.6679951520813,31.9990039461198,45.1214803633902));
#22790=CARTESIAN_POINT('Ctrl Pts',(33.6645084345824,32.4921586880507,45.1545691261406));
#22791=CARTESIAN_POINT('Ctrl Pts',(33.4320886779645,32.9881690369999,45.1876578888911));
#22792=CARTESIAN_POINT('Ctrl Pts',(33.0490210948825,33.2978042997919,45.2207466516416));
#22793=CARTESIAN_POINT('Ctrl Pts',(32.6201723838579,33.6444446556993,45.2577899147148));
#22794=CARTESIAN_POINT('Ctrl Pts',(32.002515719258,33.7574998385532,45.2948331777881));
#22795=CARTESIAN_POINT('Ctrl Pts',(31.4786874417,33.5852364096959,45.3318764408613));
#22796=CARTESIAN_POINT('Ctrl Pts',(30.954859164142,33.4129729808386,45.3689197039346));
#22797=CARTESIAN_POINT('Ctrl Pts',(30.5248592736258,32.9553909402701,45.4059629670078));
#22798=CARTESIAN_POINT('Ctrl Pts',(30.3854533884744,32.4218773486192,45.4430062300811));
#22799=CARTESIAN_POINT('Ctrl Pts',(30.246047503323,31.8883637569683,45.4800494931543));
#22800=CARTESIAN_POINT('Ctrl Pts',(30.3972356235363,31.2789186142351,45.5170927562275));
#22801=CARTESIAN_POINT('Ctrl Pts',(30.7698348850881,30.8724207131555,45.5541360193008));
#22802=CARTESIAN_POINT('Ctrl Pts',(31.14243414664,30.465922812076,45.591179282374));
#22803=CARTESIAN_POINT('Ctrl Pts',(31.7364445495304,30.2623721526502,45.6282225454473));
#22804=CARTESIAN_POINT('Ctrl Pts',(32.280050154284,30.3549124129238,45.6652658085205));
#22805=CARTESIAN_POINT('Ctrl Pts',(32.8236557590377,30.4474526731974,45.7023090715938));
#22806=CARTESIAN_POINT('Ctrl Pts',(33.3168565656545,30.8360838531705,45.739352334667));
#22807=CARTESIAN_POINT('Ctrl Pts',(33.5339665592967,31.3429704321522,45.7763955977402));
#22808=CARTESIAN_POINT('Ctrl Pts',(33.6220469313765,31.5486116268756,45.7914238529569));
#22809=CARTESIAN_POINT('Ctrl Pts',(33.664686018092,31.7737162629005,45.8064521081735));
#22810=CARTESIAN_POINT('Ctrl Pts',(33.6636859641007,31.9991832784139,45.8214803633902));
#22811=CARTESIAN_POINT('Ctrl Pts',(33.664255890244,32.0011936369589,45.6285196366098));
#22812=CARTESIAN_POINT('Ctrl Pts',(33.6618654719116,31.640443123746,45.6044535437428));
#22813=CARTESIAN_POINT('Ctrl Pts',(33.5466852070223,31.2783021822037,45.5803874508758));
#22814=CARTESIAN_POINT('Ctrl Pts',(33.3304349107605,30.9926846351569,45.5563213580088));
#22815=CARTESIAN_POINT('Ctrl Pts',(32.997575868856,30.553053408266,45.5192780949356));
#22816=CARTESIAN_POINT('Ctrl Pts',(32.4252586367481,30.2947237334304,45.4822348318623));
#22817=CARTESIAN_POINT('Ctrl Pts',(31.8753724765885,30.3359058691205,45.4451915687891));
#22818=CARTESIAN_POINT('Ctrl Pts',(31.3254863164288,30.3770880048106,45.4081483057158));
#22819=CARTESIAN_POINT('Ctrl Pts',(30.7980312282173,30.7177819510265,45.3711050426426));
#22820=CARTESIAN_POINT('Ctrl Pts',(30.5343678003135,31.2020880053156,45.3340617795693));
#22821=CARTESIAN_POINT('Ctrl Pts',(30.2707043724096,31.6863940596048,45.2970185164961));
#22822=CARTESIAN_POINT('Ctrl Pts',(30.2708326048134,32.3143122219674,45.2599752534229));
#22823=CARTESIAN_POINT('Ctrl Pts',(30.5346938190722,32.7985105460506,45.2229319903496));
#22824=CARTESIAN_POINT('Ctrl Pts',(30.798555033331,33.2827088701339,45.1858887272764));
#22825=CARTESIAN_POINT('Ctrl Pts',(31.3261492294448,33.6231873559379,45.1488454642032));
#22826=CARTESIAN_POINT('Ctrl Pts',(31.8760521640323,33.6641448945264,45.1118022011299));
#22827=CARTESIAN_POINT('Ctrl Pts',(32.4259550986198,33.7051024331148,45.0747589380567));
#22828=CARTESIAN_POINT('Ctrl Pts',(32.9981667716809,33.4465390244878,45.0377156749834));
#22829=CARTESIAN_POINT('Ctrl Pts',(33.3308462243117,33.0067718824314,45.0006724119102));
#22830=CARTESIAN_POINT('Ctrl Pts',(33.5468436266396,32.7212461020977,44.97662148681));
#22831=CARTESIAN_POINT('Ctrl Pts',(33.6618671500066,32.3593345903844,44.9525705617099));
#22832=CARTESIAN_POINT('Ctrl Pts',(33.6642508883749,31.9988087175676,44.9285196366098));
#22833=CARTESIAN_POINT('Origin',(32.,32.,48.));
#22834=CARTESIAN_POINT('',(33.6685558202892,31.9994792812332,44.2285196366098));
#22835=CARTESIAN_POINT('',(33.6667054848825,32.0014513625929,44.4214803633902));
#22836=CARTESIAN_POINT('',(33.666,32.,48.));
#22837=CARTESIAN_POINT('Ctrl Pts',(33.6667054848825,32.0014513625929,44.4214803633902));
#22838=CARTESIAN_POINT('Ctrl Pts',(33.6676777367435,32.1077703681721,44.4285996179613));
#22839=CARTESIAN_POINT('Ctrl Pts',(33.6583759250957,32.2139199029793,44.4357188725324));
#22840=CARTESIAN_POINT('Ctrl Pts',(33.6381835786891,32.3179556896481,44.4428381271035));
#22841=CARTESIAN_POINT('Ctrl Pts',(33.5331177473534,32.8592799218571,44.4798813901767));
#22842=CARTESIAN_POINT('Ctrl Pts',(33.133203613556,33.3433769320565,44.51692465325));
#22843=CARTESIAN_POINT('Ctrl Pts',(32.6214397164782,33.5487265532852,44.5539679163233));
#22844=CARTESIAN_POINT('Ctrl Pts',(32.1096758194004,33.7540761745139,44.5910111793965));
#22845=CARTESIAN_POINT('Ctrl Pts',(31.4860621590421,33.6806784067719,44.6280544424697));
#22846=CARTESIAN_POINT('Ctrl Pts',(31.0359609649793,33.3621196705955,44.665097705543));
#22847=CARTESIAN_POINT('Ctrl Pts',(30.5858597709165,33.043560934419,44.7021409686162));
#22848=CARTESIAN_POINT('Ctrl Pts',(30.3092710431491,32.4798412298081,44.7391842316895));
#22849=CARTESIAN_POINT('Ctrl Pts',(30.3327602837635,31.9289156369497,44.7762274947627));
#22850=CARTESIAN_POINT('Ctrl Pts',(30.3562495243778,31.3779900440912,44.813270757836));
#22851=CARTESIAN_POINT('Ctrl Pts',(30.679816733374,30.8398585629853,44.8503140209092));
#22852=CARTESIAN_POINT('Ctrl Pts',(31.1553993103854,30.5607672414896,44.8873572839824));
#22853=CARTESIAN_POINT('Ctrl Pts',(31.6309818873969,30.2816759199939,44.9244005470557));
#22854=CARTESIAN_POINT('Ctrl Pts',(32.2585798324236,30.2616247581084,44.9614438101289));
#22855=CARTESIAN_POINT('Ctrl Pts',(32.7510077288296,30.509789058789,44.9984870732022));
#22856=CARTESIAN_POINT('Ctrl Pts',(33.2434356252356,30.7579533594696,45.0355303362754));
#22857=CARTESIAN_POINT('Ctrl Pts',(33.6006934730207,31.2743331227162,45.0725735993486));
#22858=CARTESIAN_POINT('Ctrl Pts',(33.6593020181886,31.8226357688199,45.1096168624218));
#22859=CARTESIAN_POINT('Ctrl Pts',(33.6655586892147,31.8811690299613,45.1135713627446));
#22860=CARTESIAN_POINT('Ctrl Pts',(33.668411856253,31.9400660945945,45.1175258630674));
#22861=CARTESIAN_POINT('Ctrl Pts',(33.6679951520813,31.9990039461198,45.1214803633902));
#22862=CARTESIAN_POINT('Ctrl Pts',(33.6642508883749,31.9988087175676,44.9285196366098));
#22863=CARTESIAN_POINT('Ctrl Pts',(33.6655385866398,31.8040522178409,44.9155272986367));
#22864=CARTESIAN_POINT('Ctrl Pts',(33.6339560460374,31.6097000715273,44.9025349606635));
#22865=CARTESIAN_POINT('Ctrl Pts',(33.5676642525274,31.4280121615218,44.8895426226904));
#22866=CARTESIAN_POINT('Ctrl Pts',(33.3786555959121,30.9099904581544,44.8524993596172));
#22867=CARTESIAN_POINT('Ctrl Pts',(32.9074910504814,30.4949179269053,44.815456096544));
#22868=CARTESIAN_POINT('Ctrl Pts',(32.3697729574409,30.3727295074374,44.7784128334707));
#22869=CARTESIAN_POINT('Ctrl Pts',(31.8320548644005,30.2505410879696,44.7413695703975));
#22870=CARTESIAN_POINT('Ctrl Pts',(31.2277832237503,30.4212367802829,44.7043263073242));
#22871=CARTESIAN_POINT('Ctrl Pts',(30.8334694617253,30.806707161133,44.667283044251));
#22872=CARTESIAN_POINT('Ctrl Pts',(30.4391556997004,31.1921775419831,44.6302397811777));
#22873=CARTESIAN_POINT('Ctrl Pts',(30.2547998163006,31.79242261137,44.5931965181045));
#22874=CARTESIAN_POINT('Ctrl Pts',(30.3647620641418,32.332773480237,44.5561532550313));
#22875=CARTESIAN_POINT('Ctrl Pts',(30.4747243119829,32.873124349104,44.519109991958));
#22876=CARTESIAN_POINT('Ctrl Pts',(30.8790046910649,33.353581017451,44.4820667288848));
#22877=CARTESIAN_POINT('Ctrl Pts',(31.3926066920388,33.5542891190076,44.4450234658115));
#22878=CARTESIAN_POINT('Ctrl Pts',(31.9062086930126,33.7549972205642,44.4079802027383));
#22879=CARTESIAN_POINT('Ctrl Pts',(32.5291323158784,33.6759567553303,44.370936939665));
#22880=CARTESIAN_POINT('Ctrl Pts',(32.9763310884756,33.3533362116233,44.3338936765918));
#22881=CARTESIAN_POINT('Ctrl Pts',(33.4003680786871,33.0474251655366,44.2987689965978));
#22882=CARTESIAN_POINT('Ctrl Pts',(33.6664114806385,32.5225121367035,44.2636443166038));
#22883=CARTESIAN_POINT('Ctrl Pts',(33.6685558202892,31.9994792812332,44.2285196366098));
#22884=CARTESIAN_POINT('Origin',(32.,32.,48.));
#22885=CARTESIAN_POINT('',(33.6657844257744,32.0015219728729,43.5285196366098));
#22886=CARTESIAN_POINT('',(33.6632945194008,32.000080914311,43.7214803633902));
#22887=CARTESIAN_POINT('',(33.666,32.,48.));
#22888=CARTESIAN_POINT('Ctrl Pts',(33.6632945194008,32.000080914311,43.7214803633902));
#22889=CARTESIAN_POINT('Ctrl Pts',(33.663412856101,32.273188844988,43.7396733728552));
#22890=CARTESIAN_POINT('Ctrl Pts',(33.5999068196939,32.5462449457584,43.7578663823202));
#22891=CARTESIAN_POINT('Ctrl Pts',(33.472475203927,32.7852120935461,43.7760593917852));
#22892=CARTESIAN_POINT('Ctrl Pts',(33.2130083534433,33.2717793620567,43.8131026548584));
#22893=CARTESIAN_POINT('Ctrl Pts',(32.6885182052593,33.6170203129166,43.8501459179316));
#22894=CARTESIAN_POINT('Ctrl Pts',(32.1390086072293,33.6629545589702,43.8871891810049));
#22895=CARTESIAN_POINT('Ctrl Pts',(31.5894990091993,33.7088888050238,43.9242324440781));
#22896=CARTESIAN_POINT('Ctrl Pts',(31.0149699613232,33.4555163462711,43.9612757071514));
#22897=CARTESIAN_POINT('Ctrl Pts',(30.678322840668,33.0187790459991,43.9983189702246));
#22898=CARTESIAN_POINT('Ctrl Pts',(30.3416757200127,32.5820417457271,44.0353622332979));
#22899=CARTESIAN_POINT('Ctrl Pts',(30.2429105265783,31.961939603936,44.0724054963711));
#22900=CARTESIAN_POINT('Ctrl Pts',(30.4272216773419,31.4422279983368,44.1094487594443));
#22901=CARTESIAN_POINT('Ctrl Pts',(30.6115328281055,30.9225163927377,44.1464920225176));
#22902=CARTESIAN_POINT('Ctrl Pts',(31.078920323067,30.5031953233307,44.1835352855908));
#22903=CARTESIAN_POINT('Ctrl Pts',(31.6155101788386,30.3761438378069,44.220578548664));
#22904=CARTESIAN_POINT('Ctrl Pts',(32.1521000346101,30.2490923522831,44.2576218117373));
#22905=CARTESIAN_POINT('Ctrl Pts',(32.7578922511917,30.4143104506425,44.2946650748106));
#22906=CARTESIAN_POINT('Ctrl Pts',(33.1556795950453,30.7961952269315,44.3317083378838));
#22907=CARTESIAN_POINT('Ctrl Pts',(33.4770171574514,31.1046864975282,44.3616323463859));
#22908=CARTESIAN_POINT('Ctrl Pts',(33.662618867012,31.5545659766137,44.3915563548881));
#22909=CARTESIAN_POINT('Ctrl Pts',(33.6667054848825,32.0014513625929,44.4214803633902));
#22910=CARTESIAN_POINT('Ctrl Pts',(33.6685558202892,31.9994792812332,44.2285196366098));
#22911=CARTESIAN_POINT('Ctrl Pts',(33.6686729485811,31.9709101387794,44.2266010535306));
#22912=CARTESIAN_POINT('Ctrl Pts',(33.6680027151203,31.9423466059576,44.2246824704513));
#22913=CARTESIAN_POINT('Ctrl Pts',(33.6665278606096,31.9138246796869,44.2227638873721));
#22914=CARTESIAN_POINT('Ctrl Pts',(33.6380519378177,31.3631343136376,44.1857206242988));
#22915=CARTESIAN_POINT('Ctrl Pts',(33.3096261699052,30.827954203719,44.1486773612256));
#22916=CARTESIAN_POINT('Ctrl Pts',(32.8315364074553,30.5531798663578,44.1116340981523));
#22917=CARTESIAN_POINT('Ctrl Pts',(32.3534466450053,30.2784055289966,44.0745908350791));
#22918=CARTESIAN_POINT('Ctrl Pts',(31.725692888018,30.2640369641928,44.0375475720059));
#22919=CARTESIAN_POINT('Ctrl Pts',(31.2355318518357,30.5166491492484,44.0005043089327));
#22920=CARTESIAN_POINT('Ctrl Pts',(30.7453708156534,30.769261334304,43.9634610458594));
#22921=CARTESIAN_POINT('Ctrl Pts',(30.3928025002761,31.288854269219,43.9264177827861));
#22922=CARTESIAN_POINT('Ctrl Pts',(30.3391602551023,31.8376650444346,43.8893745197129));
#22923=CARTESIAN_POINT('Ctrl Pts',(30.2855180099285,32.3864758196501,43.8523312566396));
#22924=CARTESIAN_POINT('Ctrl Pts',(30.530801834958,32.9645044351661,43.8152879935664));
#22925=CARTESIAN_POINT('Ctrl Pts',(30.9627711818461,33.3072481305883,43.7782447304932));
#22926=CARTESIAN_POINT('Ctrl Pts',(31.3947405287341,33.6499918260105,43.7412014674199));
#22927=CARTESIAN_POINT('Ctrl Pts',(32.0133953974807,33.7574506013388,43.7041582043467));
#22928=CARTESIAN_POINT('Ctrl Pts',(32.5356426746786,33.5804519039783,43.6671149412734));
#22929=CARTESIAN_POINT('Ctrl Pts',(33.0578899518765,33.4034532066179,43.6300716782002));
#22930=CARTESIAN_POINT('Ctrl Pts',(33.4837296375257,32.9419970365686,43.593028415127));
#22931=CARTESIAN_POINT('Ctrl Pts',(33.6182998004632,32.4072432344611,43.5559851520537));
#22932=CARTESIAN_POINT('Ctrl Pts',(33.6515585595629,32.2750798522248,43.5468299802391));
#22933=CARTESIAN_POINT('Ctrl Pts',(33.6670259413327,32.138439290855,43.5376748084244));
#22934=CARTESIAN_POINT('Ctrl Pts',(33.6657844257744,32.0015219728729,43.5285196366098));
#22935=CARTESIAN_POINT('Origin',(32.,32.,48.));
#22936=CARTESIAN_POINT('',(33.6633867512256,31.999584573057,42.8285196366098));
#22937=CARTESIAN_POINT('',(33.6664085438525,31.9985061360825,43.0214803633902));
#22938=CARTESIAN_POINT('',(33.666,32.,48.));
#22939=CARTESIAN_POINT('Ctrl Pts',(33.6664085438525,31.9985061360825,43.0214803633902));
#22940=CARTESIAN_POINT('Ctrl Pts',(33.6623727759815,32.4357766487213,43.0507471277491));
#22941=CARTESIAN_POINT('Ctrl Pts',(33.4856937087816,32.8759335396009,43.0800138921079));
#22942=CARTESIAN_POINT('Ctrl Pts',(33.1768027043535,33.1831638308965,43.1092806564668));
#22943=CARTESIAN_POINT('Ctrl Pts',(32.7858359887411,33.5720285637718,43.14632391954));
#22944=CARTESIAN_POINT('Ctrl Pts',(32.1830625609484,33.7479416781363,43.1833671826133));
#22945=CARTESIAN_POINT('Ctrl Pts',(31.6443082716033,33.6304062847013,43.2204104456865));
#22946=CARTESIAN_POINT('Ctrl Pts',(31.1055539822583,33.5128708912663,43.2574537087598));
#22947=CARTESIAN_POINT('Ctrl Pts',(30.6308188313608,33.1018869900318,43.294496971833));
#22948=CARTESIAN_POINT('Ctrl Pts',(30.437339050589,32.585518586748,43.3315402349062));
#22949=CARTESIAN_POINT('Ctrl Pts',(30.2438592698172,32.0691501834641,43.3685834979795));
#22950=CARTESIAN_POINT('Ctrl Pts',(30.3316348591709,31.4473972781309,43.4056267610527));
#22951=CARTESIAN_POINT('Ctrl Pts',(30.6605001845156,31.0047706284025,43.442670024126));
#22952=CARTESIAN_POINT('Ctrl Pts',(30.9893655098603,30.5621439786741,43.4797132871992));
#22953=CARTESIAN_POINT('Ctrl Pts',(31.5593205711959,30.2986435845506,43.5167565502724));
#22954=CARTESIAN_POINT('Ctrl Pts',(32.1095570231048,30.3348457978698,43.5537998133457));
#22955=CARTESIAN_POINT('Ctrl Pts',(32.6597934750136,30.3710480111891,43.5908430764189));
#22956=CARTESIAN_POINT('Ctrl Pts',(33.1903113174957,30.7069528319511,43.6278863394922));
#22957=CARTESIAN_POINT('Ctrl Pts',(33.458348462345,31.1888520354127,43.6649296025654));
#22958=CARTESIAN_POINT('Ctrl Pts',(33.5947448739368,31.4340767117839,43.6837798561737));
#22959=CARTESIAN_POINT('Ctrl Pts',(33.6631719076463,31.7171066342395,43.7026301097819));
#22960=CARTESIAN_POINT('Ctrl Pts',(33.6632945194008,32.000080914311,43.7214803633902));
#22961=CARTESIAN_POINT('Ctrl Pts',(33.6657844257744,32.0015219728729,43.5285196366098));
#22962=CARTESIAN_POINT('Ctrl Pts',(33.6620025743914,31.5844503180668,43.5006315453512));
#22963=CARTESIAN_POINT('Ctrl Pts',(33.5031776477221,31.1648106184981,43.4727434540926));
#22964=CARTESIAN_POINT('Ctrl Pts',(33.2199064985647,30.8613299724877,43.444855362834));
#22965=CARTESIAN_POINT('Ctrl Pts',(32.843642393503,30.4582219467875,43.4078120997608));
#22966=CARTESIAN_POINT('Ctrl Pts',(32.2478135431539,30.2600573295529,43.3707688366875));
#22967=CARTESIAN_POINT('Ctrl Pts',(31.7050679985738,30.357515172611,43.3337255736143));
#22968=CARTESIAN_POINT('Ctrl Pts',(31.1623224539937,30.454973015669,43.296682310541));
#22969=CARTESIAN_POINT('Ctrl Pts',(30.6726602151827,30.8480533190197,43.2596390474678));
#22970=CARTESIAN_POINT('Ctrl Pts',(30.4601480677671,31.356884672221,43.2225957843945));
#22971=CARTESIAN_POINT('Ctrl Pts',(30.2476359203515,31.8657160254224,43.1855525213213));
#22972=CARTESIAN_POINT('Ctrl Pts',(30.3122738643314,32.4902984284745,43.1485092582481));
#22973=CARTESIAN_POINT('Ctrl Pts',(30.6244839265721,32.9448263505345,43.1114659951748));
#22974=CARTESIAN_POINT('Ctrl Pts',(30.9366939888128,33.3993542725945,43.0744227321016));
#22975=CARTESIAN_POINT('Ctrl Pts',(31.4964761693141,33.6838277136625,43.0373794690283));
#22976=CARTESIAN_POINT('Ctrl Pts',(32.0476771784704,33.6680731891249,43.0003362059551));
#22977=CARTESIAN_POINT('Ctrl Pts',(32.5988781876267,33.6523186645873,42.9632929428818));
#22978=CARTESIAN_POINT('Ctrl Pts',(33.1414980254379,33.3363361744442,42.9262496798086));
#22979=CARTESIAN_POINT('Ctrl Pts',(33.4272367945752,32.8647175541852,42.8892064167354));
#22980=CARTESIAN_POINT('Ctrl Pts',(33.5832756566817,32.6071717088116,42.8689774900269));
#22981=CARTESIAN_POINT('Ctrl Pts',(33.6627091320695,32.3032130779553,42.8487485633184));
#22982=CARTESIAN_POINT('Ctrl Pts',(33.6633867512256,31.999584573057,42.8285196366098));
#22983=CARTESIAN_POINT('Origin',(32.,32.,48.));
#22984=CARTESIAN_POINT('',(33.6673070786563,31.998696213291,42.1285196366098));
#22985=CARTESIAN_POINT('',(33.6682077659727,32.0008552789479,42.3214803633902));
#22986=CARTESIAN_POINT('',(33.666,32.,48.));
#22987=CARTESIAN_POINT('Ctrl Pts',(33.6682077659727,32.0008552789479,42.3214803633902));
#22988=CARTESIAN_POINT('Ctrl Pts',(33.6685153159273,32.0499810826626,42.3247776195697));
#22989=CARTESIAN_POINT('Ctrl Pts',(33.6665333409633,32.0990817203467,42.3280748757492));
#22990=CARTESIAN_POINT('Ctrl Pts',(33.6621810758368,32.1479713477299,42.3313721319287));
#22991=CARTESIAN_POINT('Ctrl Pts',(33.6132852384284,32.6972254032584,42.368415395002));
#22992=CARTESIAN_POINT('Ctrl Pts',(33.2652217688373,33.2198466637373,42.4054586580752));
#22993=CARTESIAN_POINT('Ctrl Pts',(32.7772628054379,33.4766867130642,42.4425019211484));
#22994=CARTESIAN_POINT('Ctrl Pts',(32.2893038420385,33.7335267623911,42.4795451842217));
#22995=CARTESIAN_POINT('Ctrl Pts',(31.6614493848307,33.7245856005659,42.5165884472949));
#22996=CARTESIAN_POINT('Ctrl Pts',(31.1810021371072,33.4539545340837,42.5536317103682));
#22997=CARTESIAN_POINT('Ctrl Pts',(30.7005548893838,33.1833234676016,42.5906749734414));
#22998=CARTESIAN_POINT('Ctrl Pts',(30.3675148511445,32.6510024964624,42.6277182365146));
#22999=CARTESIAN_POINT('Ctrl Pts',(30.3342793844886,32.1005788716261,42.6647614995879));
#23000=CARTESIAN_POINT('Ctrl Pts',(30.3010439178327,31.5501552467898,42.7018047626611));
#23001=CARTESIAN_POINT('Ctrl Pts',(30.5676130227601,30.9816289682562,42.7388480257344));
#23002=CARTESIAN_POINT('Ctrl Pts',(31.0120060988108,30.6551545475858,42.7758912888076));
#23003=CARTESIAN_POINT('Ctrl Pts',(31.4563991748616,30.3286801269153,42.8129345518809));
#23004=CARTESIAN_POINT('Ctrl Pts',(32.0786162220357,30.2442575641079,42.8499778149541));
#23005=CARTESIAN_POINT('Ctrl Pts',(32.5939341052261,30.4405181816957,42.8870210780273));
#23006=CARTESIAN_POINT('Ctrl Pts',(33.1092519884165,30.6367787992834,42.9240643411006));
#23007=CARTESIAN_POINT('Ctrl Pts',(33.5176707076233,31.1137225972663,42.9611076041738));
#23008=CARTESIAN_POINT('Ctrl Pts',(33.6323000655106,31.6531026719508,42.9981508672471));
#23009=CARTESIAN_POINT('Ctrl Pts',(33.656364226718,31.7663348256369,43.0059273659615));
#23010=CARTESIAN_POINT('Ctrl Pts',(33.6674808914231,31.882318588403,43.0137038646758));
#23011=CARTESIAN_POINT('Ctrl Pts',(33.6664085438525,31.9985061360825,43.0214803633902));
#23012=CARTESIAN_POINT('Ctrl Pts',(33.6633867512256,31.999584573057,42.8285196366098));
#23013=CARTESIAN_POINT('Ctrl Pts',(33.6639499900263,31.7472077720117,42.8117053002451));
#23014=CARTESIAN_POINT('Ctrl Pts',(33.6101009847085,31.495059054249,42.7948909638803));
#23015=CARTESIAN_POINT('Ctrl Pts',(33.5006047722315,31.2699817522125,42.7780766275156));
#23016=CARTESIAN_POINT('Ctrl Pts',(33.2593762802871,30.7741193208738,42.7410333644424));
#23017=CARTESIAN_POINT('Ctrl Pts',(32.7480615959347,30.4096492085713,42.7039901013691));
#23018=CARTESIAN_POINT('Ctrl Pts',(32.2006355392698,30.3433508109352,42.6669468382959));
#23019=CARTESIAN_POINT('Ctrl Pts',(31.653209482605,30.277052413299,42.6299035752227));
#23020=CARTESIAN_POINT('Ctrl Pts',(31.0696720536276,30.508925730329,42.5928603121494));
#23021=CARTESIAN_POINT('Ctrl Pts',(30.7170468295479,30.9328670893641,42.5558170490762));
#23022=CARTESIAN_POINT('Ctrl Pts',(30.3644216054682,31.3568084483991,42.5187737860029));
#23023=CARTESIAN_POINT('Ctrl Pts',(30.242708586286,31.9728178494392,42.4817305229297));
#23024=CARTESIAN_POINT('Ctrl Pts',(30.4076029622781,32.4990121369647,42.4446872598564));
#23025=CARTESIAN_POINT('Ctrl Pts',(30.5724973382702,33.0252064244902,42.4076439967832));
#23026=CARTESIAN_POINT('Ctrl Pts',(31.0239991094365,33.4615855985011,42.37060073371));
#23027=CARTESIAN_POINT('Ctrl Pts',(31.5555035675824,33.6084660906392,42.3335574706367));
#23028=CARTESIAN_POINT('Ctrl Pts',(32.0870080257284,33.7553465827773,42.2965142075635));
#23029=CARTESIAN_POINT('Ctrl Pts',(32.698515170854,33.6127283930426,42.2594709444902));
#23030=CARTESIAN_POINT('Ctrl Pts',(33.1102025419581,33.2458705045939,42.222427681417));
#23031=CARTESIAN_POINT('Ctrl Pts',(33.4580908657248,32.9358644542971,42.1911249998146));
#23032=CARTESIAN_POINT('Ctrl Pts',(33.6632926257187,32.4657341508945,42.1598223182122));
#23033=CARTESIAN_POINT('Ctrl Pts',(33.6673070786563,31.998696213291,42.1285196366098));
#23034=CARTESIAN_POINT('Origin',(32.,32.,48.));
#23035=CARTESIAN_POINT('',(33.6674739163907,32.0012102324881,41.4285196366098));
#23036=CARTESIAN_POINT('',(33.6638410485742,32.0009454217316,41.6214803633902));
#23037=CARTESIAN_POINT('',(33.666,32.,48.));
#23038=CARTESIAN_POINT('',(30.7309291201476,33.0793586530485,41.));
#23039=CARTESIAN_POINT('Ctrl Pts',(33.6674739163907,32.0012102324881,41.4285196366098));
#23040=CARTESIAN_POINT('Ctrl Pts',(33.6635382116946,31.5283279659125,41.3968095469596));
#23041=CARTESIAN_POINT('Ctrl Pts',(33.4523210017542,31.0524651525534,41.3650994573094));
#23042=CARTESIAN_POINT('Ctrl Pts',(33.0964756390096,30.7421790963558,41.3333893676592));
#23043=CARTESIAN_POINT('Ctrl Pts',(32.6807822893234,30.3797074624224,41.296346104586));
#23044=CARTESIAN_POINT('Ctrl Pts',(32.067721107232,30.2431913221054,41.2593028415127));
#23045=CARTESIAN_POINT('Ctrl Pts',(31.5378645260577,30.3962173009215,41.2222595784394));
#23046=CARTESIAN_POINT('Ctrl Pts',(31.0080079448833,30.5492432797376,41.1852163153662));
#23047=CARTESIAN_POINT('Ctrl Pts',(30.5613559646262,30.9918113776869,41.148173052293));
#23048=CARTESIAN_POINT('Ctrl Pts',(30.4023646913452,31.5188488463209,41.1111297892197));
#23049=CARTESIAN_POINT('Ctrl Pts',(30.2433734180642,32.0458863149549,41.0740865261465));
#23050=CARTESIAN_POINT('Ctrl Pts',(30.3720428517593,32.6573931542737,41.0370432630732));
#23051=CARTESIAN_POINT('Ctrl Pts',(30.7309291201476,33.0793586530485,41.));
#23052=CARTESIAN_POINT('',(33.2714670682823,33.0812099660022,41.));
#23053=CARTESIAN_POINT('Origin',(32.,32.,41.));
#23054=CARTESIAN_POINT('Ctrl Pts',(33.2714683883714,33.0812109859128,41.));
#23055=CARTESIAN_POINT('Ctrl Pts',(32.9206802907987,33.4926491725661,41.0363148168372));
#23056=CARTESIAN_POINT('Ctrl Pts',(32.350892837512,33.7186726653411,41.0726296336745));
#23057=CARTESIAN_POINT('Ctrl Pts',(31.8135997899101,33.6581999673401,41.1089444505117));
#23058=CARTESIAN_POINT('Ctrl Pts',(31.2655290726889,33.5965142352919,41.145987713585));
#23059=CARTESIAN_POINT('Ctrl Pts',(30.7512694596539,33.2367232647846,41.1830309766582));
#23060=CARTESIAN_POINT('Ctrl Pts',(30.5058095822466,32.7430255187007,41.2200742397314));
#23061=CARTESIAN_POINT('Ctrl Pts',(30.2603497048393,32.2493277726168,41.2571175028047));
#23062=CARTESIAN_POINT('Ctrl Pts',(30.2836895630596,31.6217232509564,41.2941607658779));
#23063=CARTESIAN_POINT('Ctrl Pts',(30.5653172802778,31.1476214797862,41.3312040289512));
#23064=CARTESIAN_POINT('Ctrl Pts',(30.8469449974961,30.6735197086161,41.3682472920244));
#23065=CARTESIAN_POINT('Ctrl Pts',(31.3868605737123,30.3529206879363,41.4052905550977));
#23066=CARTESIAN_POINT('Ctrl Pts',(31.9379165708235,30.3324171997514,41.4423338181709));
#23067=CARTESIAN_POINT('Ctrl Pts',(32.4889725679347,30.3119137115664,41.4793770812441));
#23068=CARTESIAN_POINT('Ctrl Pts',(33.0511689859409,30.5915057558763,41.5164203443174));
#23069=CARTESIAN_POINT('Ctrl Pts',(33.3672907256419,31.0433098899838,41.5534636073906));
#23070=CARTESIAN_POINT('Ctrl Pts',(33.5607723779188,31.3198356691197,41.5761358593905));
#23071=CARTESIAN_POINT('Ctrl Pts',(33.6620738029635,31.6608725539045,41.5988081113903));
#23072=CARTESIAN_POINT('Ctrl Pts',(33.6638410485742,32.0009454217316,41.6214803633902));
#23073=CARTESIAN_POINT('Origin',(32.,32.,39.4540747194623));
#23074=CARTESIAN_POINT('',(34.0532846274147,32.0018314602113,53.7459252805377));
#23075=CARTESIAN_POINT('',(34.0546389144305,31.9981689288227,53.8040747194623));
#23076=CARTESIAN_POINT('',(34.05475,32.0000000000002,39.4540747194623));
#23077=CARTESIAN_POINT('',(31.6163320011532,34.0186125009919,54.));
#23078=CARTESIAN_POINT('Ctrl Pts',(34.0546389144305,31.9981689288227,53.8040747194623));
#23079=CARTESIAN_POINT('Ctrl Pts',(34.049372166387,32.5196382919465,53.832339883235));
#23080=CARTESIAN_POINT('Ctrl Pts',(33.5817166966653,33.7322181453664,53.8976483100809));
#23081=CARTESIAN_POINT('Ctrl Pts',(32.2875197530249,34.146181938655,53.9629567369268));
#23082=CARTESIAN_POINT('Ctrl Pts',(31.6163320011532,34.0186125009919,54.));
#23083=CARTESIAN_POINT('',(30.6584342291726,33.5612633655757,54.));
#23084=CARTESIAN_POINT('Origin',(32.,32.,54.));
#23085=CARTESIAN_POINT('Ctrl Pts',(34.0532846274147,32.0018314602113,53.7459252805377));
#23086=CARTESIAN_POINT('Ctrl Pts',(34.0549510377389,32.2111834105163,53.7572587737813));
#23087=CARTESIAN_POINT('Ctrl Pts',(33.9292547992907,33.10278246478,53.8056355300982));
#23088=CARTESIAN_POINT('Ctrl Pts',(32.6546770842451,34.3305889284731,53.8903271032523));
#23089=CARTESIAN_POINT('Ctrl Pts',(31.1647629090491,33.9952107638275,53.9636851831627));
#23090=CARTESIAN_POINT('Ctrl Pts',(30.6584328166059,33.5612648614875,54.));
#23091=CARTESIAN_POINT('Origin',(32.,32.,39.4540747194623));
#23092=CARTESIAN_POINT('',(34.0520083050621,31.9988943672661,53.0459252805377));
#23093=CARTESIAN_POINT('',(34.0578094464953,32.0007573833008,53.1040747194624));
#23094=CARTESIAN_POINT('',(34.05475,32.0000000000002,39.4540747194623));
#23095=CARTESIAN_POINT('Ctrl Pts',(34.0578094464953,32.0007573833008,53.1040747194624));
#23096=CARTESIAN_POINT('Ctrl Pts',(34.0580096988745,32.0429235568551,53.1063703750556));
#23097=CARTESIAN_POINT('Ctrl Pts',(34.037719062628,32.7652974437369,53.1457092937222));
#23098=CARTESIAN_POINT('Ctrl Pts',(33.188671276515,34.1177969804317,53.2220914754619));
#23099=CARTESIAN_POINT('Ctrl Pts',(30.8656743329815,34.1473078555715,53.3332212646817));
#23100=CARTESIAN_POINT('Ctrl Pts',(29.5804895506539,32.2117839119326,53.4443510539014));
#23101=CARTESIAN_POINT('Ctrl Pts',(30.5102290402516,30.0821246648111,53.5554808431211));
#23102=CARTESIAN_POINT('Ctrl Pts',(32.8021732937378,29.7083047001831,53.6666106323408));
#23103=CARTESIAN_POINT('Ctrl Pts',(33.9655643210943,30.9925292306587,53.7494752577879));
#23104=CARTESIAN_POINT('Ctrl Pts',(34.0562745687535,31.8362201112415,53.7952966201617));
#23105=CARTESIAN_POINT('Ctrl Pts',(34.0546389144305,31.9981689288227,53.8040747194623));
#23106=CARTESIAN_POINT('Ctrl Pts',(34.0520083050621,31.9988943672661,53.0459252805377));
#23107=CARTESIAN_POINT('Ctrl Pts',(34.0499814160986,32.4134550802263,53.0683325286752));
#23108=CARTESIAN_POINT('Ctrl Pts',(33.7267546549923,33.5162657199585,53.127783039886));
#23109=CARTESIAN_POINT('Ctrl Pts',(31.9269572256365,34.4274725972727,53.2242768141699));
#23110=CARTESIAN_POINT('Ctrl Pts',(29.9209961576786,33.2553327321614,53.3354066033897));
#23111=CARTESIAN_POINT('Ctrl Pts',(29.8177590626321,30.9342477419074,53.4465363926093));
#23112=CARTESIAN_POINT('Ctrl Pts',(31.7116016611041,29.5886825160599,53.5576661818292));
#23113=CARTESIAN_POINT('Ctrl Pts',(33.6494719816339,30.36181998904,53.6574624778052));
#23114=CARTESIAN_POINT('Ctrl Pts',(34.0495044137635,31.5269213561486,53.7202155107081));
#23115=CARTESIAN_POINT('Ctrl Pts',(34.0532846274147,32.0018314602113,53.7459252805377));
#23116=CARTESIAN_POINT('Origin',(32.,32.,39.4540747194623));
#23117=CARTESIAN_POINT('',(34.0573711123367,31.9988731525912,52.3459252805377));
#23118=CARTESIAN_POINT('',(34.0524438258503,32.0013942153142,52.4040747194624));
#23119=CARTESIAN_POINT('',(34.05475,32.0000000000002,39.4540747194623));
#23120=CARTESIAN_POINT('Ctrl Pts',(34.0524438258503,32.0013942153142,52.4040747194623));
#23121=CARTESIAN_POINT('Ctrl Pts',(34.0539875421913,32.2486122323593,52.4174441299495));
#23122=CARTESIAN_POINT('Ctrl Pts',(33.8982128380036,33.1789291235334,52.4678568035099));
#23123=CARTESIAN_POINT('Ctrl Pts',(32.5140660369754,34.3735522478524,52.5553127401435));
#23124=CARTESIAN_POINT('Ctrl Pts',(30.2847730690242,33.7193028360775,52.6664425293633));
#23125=CARTESIAN_POINT('Ctrl Pts',(29.6252320317178,31.4915687389112,52.7775723185829));
#23126=CARTESIAN_POINT('Ctrl Pts',(31.1390630925179,29.7291402212096,52.8887021078028));
#23127=CARTESIAN_POINT('Ctrl Pts',(33.3932462266972,30.0384636275678,52.9975362414291));
#23128=CARTESIAN_POINT('Ctrl Pts',(34.0547783772501,31.3625198132227,53.0693271119824));
#23129=CARTESIAN_POINT('Ctrl Pts',(34.0578094464953,32.0007573833008,53.1040747194624));
#23130=CARTESIAN_POINT('Ctrl Pts',(34.0573711123367,31.9988731525912,52.3459252805377));
#23131=CARTESIAN_POINT('Ctrl Pts',(34.0533078419724,32.6141860750411,52.3794062835691));
#23132=CARTESIAN_POINT('Ctrl Pts',(33.4332399393382,33.917382784162,52.4499305496737));
#23133=CARTESIAN_POINT('Ctrl Pts',(31.216995453309,34.2988945058415,52.5574980788517));
#23134=CARTESIAN_POINT('Ctrl Pts',(29.6439536232049,32.5891178954443,52.6686278680713));
#23135=CARTESIAN_POINT('Ctrl Pts',(30.2271405879685,30.340185676392,52.7797576572911));
#23136=CARTESIAN_POINT('Ctrl Pts',(32.4328278728442,29.6103000988841,52.8908874465108));
#23137=CARTESIAN_POINT('Ctrl Pts',(33.8775323764099,30.773632426936,52.979609987593));
#23138=CARTESIAN_POINT('Ctrl Pts',(34.0533322327912,31.7281107016673,53.031289265602));
#23139=CARTESIAN_POINT('Ctrl Pts',(34.0520083050621,31.9988943672661,53.0459252805377));
#23140=CARTESIAN_POINT('Origin',(32.,32.,39.4540747194623));
#23141=CARTESIAN_POINT('',(34.0554020230033,32.0018240973642,51.6459252805377));
#23142=CARTESIAN_POINT('',(34.0527564569811,31.9984585482624,51.7040747194623));
#23143=CARTESIAN_POINT('',(34.05475,32.0000000000002,39.4540747194623));
#23144=CARTESIAN_POINT('Ctrl Pts',(34.0527564569812,31.9984585482624,51.7040747194623));
#23145=CARTESIAN_POINT('Ctrl Pts',(34.0496054294021,32.4502717890878,51.7285178848434));
#23146=CARTESIAN_POINT('Ctrl Pts',(33.6800481554996,33.5914868140557,51.7900043132977));
#23147=CARTESIAN_POINT('Ctrl Pts',(31.7940455819115,34.4198338709223,51.8885340048252));
#23148=CARTESIAN_POINT('Ctrl Pts',(29.8553459812909,33.1395052258002,51.9996637940449));
#23149=CARTESIAN_POINT('Ctrl Pts',(29.879410395147,30.8163137990511,52.1107935832647));
#23150=CARTESIAN_POINT('Ctrl Pts',(31.8442155880729,29.5764190605415,52.2219233724844));
#23151=CARTESIAN_POINT('Ctrl Pts',(33.6980657674601,30.436884819778,52.3196837512169));
#23152=CARTESIAN_POINT('Ctrl Pts',(34.0497102937227,31.5636334854927,52.3804008668763));
#23153=CARTESIAN_POINT('Ctrl Pts',(34.0524438258503,32.0013942153142,52.4040747194623));
#23154=CARTESIAN_POINT('Ctrl Pts',(34.0554020230033,32.0018240973642,51.6459252805377));
#23155=CARTESIAN_POINT('Ctrl Pts',(34.0566763784363,32.1402143135672,51.6534367753898));
#23156=CARTESIAN_POINT('Ctrl Pts',(33.9808503772797,32.9596933290486,51.697991533315));
#23157=CARTESIAN_POINT('Ctrl Pts',(32.8805414680095,34.2633293614917,51.7795895543134));
#23158=CARTESIAN_POINT('Ctrl Pts',(30.5761492876849,33.9673998582603,51.8907193435333));
#23159=CARTESIAN_POINT('Ctrl Pts',(29.5748498323699,31.8709273512164,52.0018491327529));
#23160=CARTESIAN_POINT('Ctrl Pts',(30.7930215224583,29.8925807110175,52.1129789219727));
#23161=CARTESIAN_POINT('Ctrl Pts',(33.1158068029996,29.8429213928206,52.2241087111924));
#23162=CARTESIAN_POINT('Ctrl Pts',(34.0252705758902,31.1875940610687,52.3017574973808));
#23163=CARTESIAN_POINT('Ctrl Pts',(34.0578034299003,31.9334060387527,52.3423630204959));
#23164=CARTESIAN_POINT('Ctrl Pts',(34.0573711123367,31.9988731525912,52.3459252805377));
#23165=CARTESIAN_POINT('Origin',(32.,32.,39.4540747194623));
#23166=CARTESIAN_POINT('',(34.0514089815509,31.9999806721048,50.9459252805377));
#23167=CARTESIAN_POINT('',(34.0579890960703,31.9994845671529,51.0040747194623));
#23168=CARTESIAN_POINT('',(34.05475,32.0000000000002,39.4540747194623));
#23169=CARTESIAN_POINT('Ctrl Pts',(34.0579890960703,31.9994845671529,51.0040747194623));
#23170=CARTESIAN_POINT('Ctrl Pts',(34.0557930142123,32.6516937718654,51.0395916397372));
#23171=CARTESIAN_POINT('Ctrl Pts',(33.3683017971665,33.9881257659273,51.1121518230855));
#23172=CARTESIAN_POINT('Ctrl Pts',(31.0922024415436,34.2525356254733,51.2217552695068));
#23173=CARTESIAN_POINT('Ctrl Pts',(29.6152124997993,32.4591314922087,51.3328850587266));
#23174=CARTESIAN_POINT('Ctrl Pts',(30.3207542148726,30.2455351970729,51.4440148479463));
#23175=CARTESIAN_POINT('Ctrl Pts',(32.5631234646485,29.6376060617633,51.5551446371661));
#23176=CARTESIAN_POINT('Ctrl Pts',(33.9102709101462,30.8498857953214,51.6418312610047));
#23177=CARTESIAN_POINT('Ctrl Pts',(34.0543807660552,31.7655553671776,51.6914746217701));
#23178=CARTESIAN_POINT('Ctrl Pts',(34.0527564569812,31.9984585482624,51.7040747194623));
#23179=CARTESIAN_POINT('Ctrl Pts',(34.0514089815509,31.9999806721048,50.9459252805377));
#23180=CARTESIAN_POINT('Ctrl Pts',(34.0513801084989,32.3440804516646,50.9645105302836));
#23181=CARTESIAN_POINT('Ctrl Pts',(33.8061927971795,33.3740627169736,51.0201390431027));
#23182=CARTESIAN_POINT('Ctrl Pts',(32.1767300276281,34.4221435893461,51.1128108189952));
#23183=CARTESIAN_POINT('Ctrl Pts',(30.0609756305588,33.4622576942574,51.2239406082148));
#23184=CARTESIAN_POINT('Ctrl Pts',(29.7197953084608,31.1641294150899,51.3350703974346));
#23185=CARTESIAN_POINT('Ctrl Pts',(31.4654335924627,29.6309808302345,51.4462001866543));
#23186=CARTESIAN_POINT('Ctrl Pts',(33.5492418761722,30.2230151611312,51.549818481022));
#23187=CARTESIAN_POINT('Ctrl Pts',(34.0503918392758,31.457736952328,51.6163935123165));
#23188=CARTESIAN_POINT('Ctrl Pts',(34.0554020230033,32.0018240973642,51.6459252805377));
#23189=CARTESIAN_POINT('Origin',(32.,32.,39.4540747194623));
#23190=CARTESIAN_POINT('',(34.0554729559656,31.9981860521685,50.2459252805377));
#23191=CARTESIAN_POINT('',(34.0542687898145,32.00186850902,50.3040747194623));
#23192=CARTESIAN_POINT('',(34.05475,32.0000000000002,39.4540747194623));
#23193=CARTESIAN_POINT('Ctrl Pts',(34.0542687898145,32.00186850902,50.3040747194623));
#23194=CARTESIAN_POINT('Ctrl Pts',(34.0558441392389,32.1780164452784,50.3136221315579));
#23195=CARTESIAN_POINT('Ctrl Pts',(33.9544817783467,33.0358200834104,50.3602128067267));
#23196=CARTESIAN_POINT('Ctrl Pts',(32.7551980676263,34.3081787255302,50.4438467449689));
#23197=CARTESIAN_POINT('Ctrl Pts',(30.4704836368621,33.8864232942922,50.5549765341884));
#23198=CARTESIAN_POINT('Ctrl Pts',(29.5855659947393,31.7382337215207,50.6661063234083));
#23199=CARTESIAN_POINT('Ctrl Pts',(30.910312170761,29.8296098080883,50.7772361126278));
#23200=CARTESIAN_POINT('Ctrl Pts',(33.2323288309766,29.9073034613682,50.8883659018477));
#23201=CARTESIAN_POINT('Ctrl Pts',(34.0448660563587,31.2632801450257,50.9639787707924));
#23202=CARTESIAN_POINT('Ctrl Pts',(34.0580834728828,31.9714558187451,51.002548376664));
#23203=CARTESIAN_POINT('Ctrl Pts',(34.0579890960703,31.9994845671529,51.0040747194623));
#23204=CARTESIAN_POINT('Ctrl Pts',(34.0554729559656,31.9981860521685,50.2459252805377));
#23205=CARTESIAN_POINT('Ctrl Pts',(34.0504505772786,32.544568857989,50.2755842851775));
#23206=CARTESIAN_POINT('Ctrl Pts',(33.5457057188836,33.7815642256422,50.3422865528905));
#23207=CARTESIAN_POINT('Ctrl Pts',(31.4573199785767,34.3671737292195,50.4460320836768));
#23208=CARTESIAN_POINT('Ctrl Pts',(29.7169448259793,32.828053224334,50.5571618728965));
#23209=CARTESIAN_POINT('Ctrl Pts',(30.0659970099416,30.5311073884045,50.6682916621163));
#23210=CARTESIAN_POINT('Ctrl Pts',(32.1850277570195,29.5784761411241,50.7794214513359));
#23211=CARTESIAN_POINT('Ctrl Pts',(33.8086577448288,30.6306870895215,50.8719659908098));
#23212=CARTESIAN_POINT('Ctrl Pts',(34.0514376569353,31.6582366329401,50.9274672672104));
#23213=CARTESIAN_POINT('Ctrl Pts',(34.0514089815509,31.9999806721048,50.9459252805377));
#23214=CARTESIAN_POINT('Origin',(32.,32.,39.4540747194623));
#23215=CARTESIAN_POINT('',(34.0573203109033,32.0011604784082,49.5459252805377));
#23216=CARTESIAN_POINT('',(34.0515870545632,31.9993739458396,49.6040747194623));
#23217=CARTESIAN_POINT('',(34.05475,32.0000000000002,39.4540747194623));
#23218=CARTESIAN_POINT('Ctrl Pts',(34.0515870545632,31.9993739458396,49.6040747194623));
#23219=CARTESIAN_POINT('Ctrl Pts',(34.0505442952487,32.3810853728681,49.6246958864518));
#23220=CARTESIAN_POINT('Ctrl Pts',(33.7651923599736,33.4499404762536,49.6823603165144));
#23221=CARTESIAN_POINT('Ctrl Pts',(32.0437417130131,34.4281885867619,49.7770680096504));
#23222=CARTESIAN_POINT('Ctrl Pts',(29.9837635432384,33.3538108068575,49.8881977988701));
#23223=CARTESIAN_POINT('Ctrl Pts',(29.7690231135183,31.0404400579838,49.9993275880899));
#23224=CARTESIAN_POINT('Ctrl Pts',(31.5960485363689,29.6052481620493,50.1104573773095));
#23225=CARTESIAN_POINT('Ctrl Pts',(33.6040409849523,30.2967180694215,50.2120397544338));
#23226=CARTESIAN_POINT('Ctrl Pts',(34.0497318982905,31.4945752910354,50.2765788684846));
#23227=CARTESIAN_POINT('Ctrl Pts',(34.0542687898145,32.00186850902,50.3040747194623));
#23228=CARTESIAN_POINT('Ctrl Pts',(34.0573203109033,32.0011604784082,49.5459252805377));
#23229=CARTESIAN_POINT('Ctrl Pts',(34.0577787278171,32.0689703479572,49.5496147769981));
#23230=CARTESIAN_POINT('Ctrl Pts',(34.023973004455,32.8171418610241,49.5903475365318));
#23231=CARTESIAN_POINT('Ctrl Pts',(33.1084096674749,34.160888955732,49.6681235591387));
#23232=CARTESIAN_POINT('Ctrl Pts',(30.7858081444514,34.1032715487725,49.7792533483584));
#23233=CARTESIAN_POINT('Ctrl Pts',(29.5744218402637,32.1207628294065,49.8903831375782));
#23234=CARTESIAN_POINT('Ctrl Pts',(30.5828983635668,30.0277332781861,50.0015129267979));
#23235=CARTESIAN_POINT('Ctrl Pts',(32.8882909367063,29.7397008424277,50.1126427160176));
#23236=CARTESIAN_POINT('Ctrl Pts',(33.9824181138614,31.0450604721018,50.1941135005975));
#23237=CARTESIAN_POINT('Ctrl Pts',(34.0567233870784,31.8621520924731,50.2385410221042));
#23238=CARTESIAN_POINT('Ctrl Pts',(34.0554729559656,31.9981860521685,50.2459252805377));
#23239=CARTESIAN_POINT('Origin',(32.,32.,39.4540747194623));
#23240=CARTESIAN_POINT('',(34.0519709427639,32.0010746754271,48.8459252805377));
#23241=CARTESIAN_POINT('',(34.0565622062779,31.9984640573749,48.9040747194623));
#23242=CARTESIAN_POINT('',(34.05475,32.0000000000002,39.4540747194623));
#23243=CARTESIAN_POINT('Ctrl Pts',(34.0565622062779,31.9984640573749,48.9040747194623));
#23244=CARTESIAN_POINT('Ctrl Pts',(34.0516979975066,32.5815526738416,48.9357696413457));
#23245=CARTESIAN_POINT('Ctrl Pts',(33.4873125068621,33.8543563214718,49.0045078263022));
#23246=CARTESIAN_POINT('Ctrl Pts',(31.3284246119414,34.3338808128292,49.1102892743321));
#23247=CARTESIAN_POINT('Ctrl Pts',(29.6750012209723,32.7017077937846,49.2214190635517));
#23248=CARTESIAN_POINT('Ctrl Pts',(30.1493914990076,30.4273394115725,49.3325488527715));
#23249=CARTESIAN_POINT('Ctrl Pts',(32.3174386081376,29.5922529450954,49.4436786419912));
#23250=CARTESIAN_POINT('Ctrl Pts',(33.8465760377496,30.7067804380472,49.5341872642215));
#23251=CARTESIAN_POINT('Ctrl Pts',(34.0524174776748,31.6953900959366,49.5876526233785));
#23252=CARTESIAN_POINT('Ctrl Pts',(34.0515870545632,31.9993739458396,49.6040747194623));
#23253=CARTESIAN_POINT('Ctrl Pts',(34.0519709427639,32.0010746754271,48.8459252805377));
#23254=CARTESIAN_POINT('Ctrl Pts',(34.0532664462955,32.2742243958035,48.860688531892));
#23255=CARTESIAN_POINT('Ctrl Pts',(33.8753960544161,33.231129995864,48.9124950463196));
#23256=CARTESIAN_POINT('Ctrl Pts',(32.4246384893326,34.3911702623054,49.0013448238203));
#23257=CARTESIAN_POINT('Ctrl Pts',(30.221463738974,33.6537296750593,49.1124746130401));
#23258=CARTESIAN_POINT('Ctrl Pts',(29.6459860872837,31.4028136231505,49.2236044022597));
#23259=CARTESIAN_POINT('Ctrl Pts',(31.2248764402936,29.6984360671178,49.3347341914796));
#23260=CARTESIAN_POINT('Ctrl Pts',(33.4371809965651,30.0870788803797,49.4421744842388));
#23261=CARTESIAN_POINT('Ctrl Pts',(34.0531761327167,31.3881460502207,49.5125715139249));
#23262=CARTESIAN_POINT('Ctrl Pts',(34.0573203109033,32.0011604784082,49.5459252805377));
#23263=CARTESIAN_POINT('Origin',(32.,32.,39.4540747194623));
#23264=CARTESIAN_POINT('',(34.0534017644819,31.9982546442701,48.1459252805377));
#23265=CARTESIAN_POINT('',(34.056370018364,32.0016034368772,48.2040747194623));
#23266=CARTESIAN_POINT('',(34.05475,32.0000000000002,39.4540747194623));
#23267=CARTESIAN_POINT('Ctrl Pts',(34.056370018364,32.0016034368772,48.2040747194623));
#23268=CARTESIAN_POINT('Ctrl Pts',(34.0572746605115,32.1069589678349,48.2098001331663));
#23269=CARTESIAN_POINT('Ctrl Pts',(34.0020142307117,32.893010264768,48.2525688099435));
#23270=CARTESIAN_POINT('Ctrl Pts',(32.9883371997446,34.2183784009811,48.3323807497939));
#23271=CARTESIAN_POINT('Ctrl Pts',(30.672382333998,34.0335792296485,48.4435105390137));
#23272=CARTESIAN_POINT('Ctrl Pts',(29.5714487587624,31.98767040059,48.5546403282333));
#23273=CARTESIAN_POINT('Ctrl Pts',(30.6930989429659,29.9530454872026,48.6657701174531));
#23274=CARTESIAN_POINT('Ctrl Pts',(33.0108108018152,29.7917711456301,48.7768999066728));
#23275=CARTESIAN_POINT('Ctrl Pts',(34.0062530028036,31.1210534192114,48.8563347740093));
#23276=CARTESIAN_POINT('Ctrl Pts',(34.0573830143626,31.9000711073529,48.8987263782724));
#23277=CARTESIAN_POINT('Ctrl Pts',(34.0565622062779,31.9984640573749,48.9040747194623));
#23278=CARTESIAN_POINT('Ctrl Pts',(34.0534017644819,31.9982546442701,48.1459252805377));
#23279=CARTESIAN_POINT('Ctrl Pts',(34.0495479088292,32.475453386869,48.1717622867859));
#23280=CARTESIAN_POINT('Ctrl Pts',(33.6462463167416,33.6427000934394,48.2346425561073));
#23281=CARTESIAN_POINT('Ctrl Pts',(31.7033877194777,34.4104012580895,48.3345660885019));
#23282=CARTESIAN_POINT('Ctrl Pts',(29.81409712657,33.0582257310643,48.4456958777218));
#23283=CARTESIAN_POINT('Ctrl Pts',(29.9253211382958,30.7375734909492,48.5568256669414));
#23284=CARTESIAN_POINT('Ctrl Pts',(31.935268745298,29.572280301472,48.6679554561612));
#23285=CARTESIAN_POINT('Ctrl Pts',(33.7295722946507,30.4884531450101,48.7643219940265));
#23286=CARTESIAN_POINT('Ctrl Pts',(34.0500158291392,31.5888498324735,48.8236452688188));
#23287=CARTESIAN_POINT('Ctrl Pts',(34.0519709427639,32.0010746754271,48.8459252805377));
#23288=CARTESIAN_POINT('Origin',(32.,32.,39.4540747194623));
#23289=CARTESIAN_POINT('',(34.0581463365634,31.9999545509518,47.4459252805377));
#23290=CARTESIAN_POINT('',(34.0515290664373,32.0005167771758,47.5040747194623));
#23291=CARTESIAN_POINT('',(34.05475,32.0000000000002,39.4540747194623));
#23292=CARTESIAN_POINT('Ctrl Pts',(34.0515290664373,32.0005167771758,47.5040747194623));
#23293=CARTESIAN_POINT('Ctrl Pts',(34.0522291585822,32.311502433739,47.5208738880601));
#23294=CARTESIAN_POINT('Ctrl Pts',(33.8397674344737,33.3073239463972,47.5747163197312));
#23295=CARTESIAN_POINT('Ctrl Pts',(32.2929749187864,34.410846085361,47.6656020144756));
#23296=CARTESIAN_POINT('Ctrl Pts',(30.1335187134828,33.5537891611861,47.7767318036953));
#23297=CARTESIAN_POINT('Ctrl Pts',(29.682245940453,31.2747212468355,47.8878615929151));
#23298=CARTESIAN_POINT('Ctrl Pts',(31.3521565477245,29.6594205820605,47.9989913821348));
#23299=CARTESIAN_POINT('Ctrl Pts',(33.4983863486385,30.1590534794509,48.1043957576505));
#23300=CARTESIAN_POINT('Ctrl Pts',(34.0514216516656,31.4253116928468,48.172756870093));
#23301=CARTESIAN_POINT('Ctrl Pts',(34.056370018364,32.0016034368772,48.2040747194623));
#23302=CARTESIAN_POINT('Ctrl Pts',(34.0581458524653,31.9999545574299,47.4459252805377));
#23303=CARTESIAN_POINT('Ctrl Pts',(34.0579253430689,32.6776207312427,47.4828360416797));
#23304=CARTESIAN_POINT('Ctrl Pts',(33.3217860203539,34.0357962998308,47.5567900658952));
#23305=CARTESIAN_POINT('Ctrl Pts',(31.0083166470601,34.21688457017,47.6677873531835));
#23306=CARTESIAN_POINT('Ctrl Pts',(29.5996634424752,32.3693202953617,47.7789171424034));
#23307=CARTESIAN_POINT('Ctrl Pts',(30.387772224771,30.1837580913501,47.890046931623));
#23308=CARTESIAN_POINT('Ctrl Pts',(32.6513743830742,29.6604007858116,48.0011767208428));
#23309=CARTESIAN_POINT('Ctrl Pts',(33.9311687217662,30.9020862526129,48.0864695038143));
#23310=CARTESIAN_POINT('Ctrl Pts',(34.0550732931334,31.791279748851,48.1347190237126));
#23311=CARTESIAN_POINT('Ctrl Pts',(34.0534017644819,31.9982546442701,48.1459252805377));
#23312=CARTESIAN_POINT('Origin',(32.,32.,39.4540747194623));
#23313=CARTESIAN_POINT('',(34.0535341854227,32.0017741341213,46.7459252805377));
#23314=CARTESIAN_POINT('',(34.0544757475471,31.9981230672873,46.8040747194623));
#23315=CARTESIAN_POINT('',(34.05475,32.0000000000002,39.4540747194623));
#23316=CARTESIAN_POINT('Ctrl Pts',(34.0544757475471,31.9981230672873,46.8040747194623));
#23317=CARTESIAN_POINT('Ctrl Pts',(34.0498160689549,32.5122411920882,46.831947642954));
#23318=CARTESIAN_POINT('Ctrl Pts',(33.5941431568701,33.7169900210427,46.896863829519));
#23319=CARTESIAN_POINT('Ctrl Pts',(31.571753982492,34.3905268245362,46.9988232791573));
#23320=CARTESIAN_POINT('Ctrl Pts',(29.7593951208157,32.9368580072316,47.1099530683769));
#23321=CARTESIAN_POINT('Ctrl Pts',(29.9976135462207,30.6257869015107,47.2210828575967));
#23322=CARTESIAN_POINT('Ctrl Pts',(32.0683943391477,29.5723807208067,47.3322126468164));
#23323=CARTESIAN_POINT('Ctrl Pts',(33.7730095526596,30.5640931209952,47.4265432674383));
#23324=CARTESIAN_POINT('Ctrl Pts',(34.0506854097146,31.6257587660702,47.4838306249869));
#23325=CARTESIAN_POINT('Ctrl Pts',(34.0515290664373,32.0005167771758,47.5040747194623));
#23326=CARTESIAN_POINT('Ctrl Pts',(34.0535341854227,32.0017741341213,46.7459252805377));
#23327=CARTESIAN_POINT('Ctrl Pts',(34.055200921409,32.2038215482488,46.7568665335004));
#23328=CARTESIAN_POINT('Ctrl Pts',(33.9350055282046,33.0879912574129,46.8048510495364));
#23329=CARTESIAN_POINT('Ctrl Pts',(32.6680530537252,34.3348914722883,46.8898788286455));
#23330=CARTESIAN_POINT('Ctrl Pts',(30.4007738795658,33.8277004365258,47.0010086178653));
#23331=CARTESIAN_POINT('Ctrl Pts',(29.5970891079424,31.6478177818408,47.112138407085));
#23332=CARTESIAN_POINT('Ctrl Pts',(30.9925223262469,29.790248473958,47.2232681963047));
#23333=CARTESIAN_POINT('Ctrl Pts',(33.3099881859296,29.9550197989514,47.3343979855245));
#23334=CARTESIAN_POINT('Ctrl Pts',(34.0570411385846,31.3149910839429,47.4086170136021));
#23335=CARTESIAN_POINT('Ctrl Pts',(34.058146644048,31.9975218772589,47.4457927786065));
#23336=CARTESIAN_POINT('Ctrl Pts',(34.0581458524653,31.9999545574299,47.4459252805377));
#23337=CARTESIAN_POINT('Origin',(32.,32.,39.4540747194623));
#23338=CARTESIAN_POINT('',(34.0518959992412,31.9989927018737,46.0459252805377));
#23339=CARTESIAN_POINT('',(34.0579058799806,32.0006373862481,46.1040747194624));
#23340=CARTESIAN_POINT('',(34.05475,32.0000000000002,39.4540747194623));
#23341=CARTESIAN_POINT('Ctrl Pts',(34.0579058799806,32.0006373862481,46.1040747194624));
#23342=CARTESIAN_POINT('Ctrl Pts',(34.0580482407791,32.0355942190053,46.1059781347747));
#23343=CARTESIAN_POINT('Ctrl Pts',(34.0414007574156,32.7507240455061,46.1449248131603));
#23344=CARTESIAN_POINT('Ctrl Pts',(33.2110168799234,34.1051012486052,46.2209147546191));
#23345=CARTESIAN_POINT('Ctrl Pts',(30.8883310468311,34.1592140442528,46.3320445438389));
#23346=CARTESIAN_POINT('Ctrl Pts',(29.5830325841312,32.2372375623016,46.4431743330585));
#23347=CARTESIAN_POINT('Ctrl Pts',(30.4897164895143,30.0981438360661,46.5543041222784));
#23348=CARTESIAN_POINT('Ctrl Pts',(32.7785954853513,29.6996082462917,46.665433911498));
#23349=CARTESIAN_POINT('Ctrl Pts',(33.9595497672164,30.9782871886646,46.7486907772261));
#23350=CARTESIAN_POINT('Ctrl Pts',(34.0560088065047,31.8289754789177,46.7949043798808));
#23351=CARTESIAN_POINT('Ctrl Pts',(34.0544757475471,31.9981230672873,46.8040747194623));
#23352=CARTESIAN_POINT('Ctrl Pts',(34.0518959992412,31.9989927018737,46.0459252805377));
#23353=CARTESIAN_POINT('Ctrl Pts',(34.0500891674537,32.406351678701,46.0679402883943));
#23354=CARTESIAN_POINT('Ctrl Pts',(33.7353984216385,33.5017208160384,46.1269985593241));
#23355=CARTESIAN_POINT('Ctrl Pts',(31.9525944719365,34.4281198046771,46.2231000933271));
#23356=CARTESIAN_POINT('Ctrl Pts',(29.9343825704431,33.2771991640567,46.3342298825469));
#23357=CARTESIAN_POINT('Ctrl Pts',(29.806601339792,30.9573996991398,46.4453596717666));
#23358=CARTESIAN_POINT('Ctrl Pts',(31.6861947765452,29.5917767230407,46.5564894609864));
#23359=CARTESIAN_POINT('Ctrl Pts',(33.6396491688907,30.3475933797668,46.6566779972434));
#23360=CARTESIAN_POINT('Ctrl Pts',(34.0495579351968,31.5197595363103,46.7198232704272));
#23361=CARTESIAN_POINT('Ctrl Pts',(34.0535341854227,32.0017741341213,46.7459252805377));
#23362=CARTESIAN_POINT('Origin',(32.,32.,39.4540747194623));
#23363=CARTESIAN_POINT('',(34.0572107075264,31.9987715235836,45.3459252805377));
#23364=CARTESIAN_POINT('',(34.0525989138529,32.0014721641904,45.4040747194623));
#23365=CARTESIAN_POINT('',(34.05475,32.0000000000002,39.4540747194623));
#23366=CARTESIAN_POINT('Ctrl Pts',(34.0525989138529,32.0014721641904,45.4040747194623));
#23367=CARTESIAN_POINT('Ctrl Pts',(34.0541886765981,32.2413915617398,45.4170518896686));
#23368=CARTESIAN_POINT('Ctrl Pts',(33.9044077369096,33.1642376187088,45.4670723229481));
#23369=CARTESIAN_POINT('Ctrl Pts',(32.539107606757,34.3679898941243,45.5541360193008));
#23370=CARTESIAN_POINT('Ctrl Pts',(30.3030266273459,33.737323954489,45.6652658085205));
#23371=CARTESIAN_POINT('Ctrl Pts',(29.6199972756779,31.516677972199,45.7763955977403));
#23372=CARTESIAN_POINT('Ctrl Pts',(31.1151206072547,29.7383630683434,45.88752538696));
#23373=CARTESIAN_POINT('Ctrl Pts',(33.3805970136183,30.0248808040469,45.9967517608673));
#23374=CARTESIAN_POINT('Ctrl Pts',(34.055277690139,31.355282810549,46.0689348717015));
#23375=CARTESIAN_POINT('Ctrl Pts',(34.0579058799806,32.0006373862481,46.1040747194624));
#23376=CARTESIAN_POINT('Ctrl Pts',(34.0572107075264,31.9987715235836,45.3459252805377));
#23377=CARTESIAN_POINT('Ctrl Pts',(34.0529103877299,32.6070006388191,45.3790140432882));
#23378=CARTESIAN_POINT('Ctrl Pts',(33.4453451887035,33.9036142777098,45.4491460691119));
#23379=CARTESIAN_POINT('Ctrl Pts',(31.2413200135407,34.3070365727709,45.5563213580088));
#23380=CARTESIAN_POINT('Ctrl Pts',(29.6503075134721,32.6139692897129,45.6674511472286));
#23381=CARTESIAN_POINT('Ctrl Pts',(30.2097080957199,30.3590039709295,45.7785809364483));
#23382=CARTESIAN_POINT('Ctrl Pts',(32.4075644138576,29.6058604220904,45.889710725668));
#23383=CARTESIAN_POINT('Ctrl Pts',(33.8709146442334,30.7589476010144,45.9788255070311));
#23384=CARTESIAN_POINT('Ctrl Pts',(34.0531294091684,31.7209144605013,46.030897025321));
#23385=CARTESIAN_POINT('Ctrl Pts',(34.0518959992412,31.9989927018737,46.0459252805377));
#23386=CARTESIAN_POINT('Origin',(32.,32.,39.4540747194623));
#23387=CARTESIAN_POINT('',(34.0556201050794,32.0017900283843,44.6459252805377));
#23388=CARTESIAN_POINT('',(34.0525927448309,31.9985307397491,44.7040747194623));
#23389=CARTESIAN_POINT('',(34.05475,32.0000000000002,39.4540747194623));
#23390=CARTESIAN_POINT('Ctrl Pts',(34.0525927448309,31.9985307397491,44.7040747194623));
#23391=CARTESIAN_POINT('Ctrl Pts',(34.0496527769965,32.4431829229246,44.7281256445624));
#23392=CARTESIAN_POINT('Ctrl Pts',(33.6892909574588,33.5770300444085,44.7892198327358));
#23393=CARTESIAN_POINT('Ctrl Pts',(31.8196154283712,34.4218741826645,44.8873572839824));
#23394=CARTESIAN_POINT('Ctrl Pts',(29.8675010685907,33.1620935667478,44.9984870732022));
#23395=CARTESIAN_POINT('Ctrl Pts',(29.8670266048481,30.8387775209235,45.1096168624218));
#23396=CARTESIAN_POINT('Ctrl Pts',(31.8186262612152,29.5781996950166,45.2207466516417));
#23397=CARTESIAN_POINT('Ctrl Pts',(33.6889357232157,30.4224105767702,45.318899270655));
#23398=CARTESIAN_POINT('Ctrl Pts',(34.0496507073291,31.5565429222791,45.3800086265953));
#23399=CARTESIAN_POINT('Ctrl Pts',(34.0525989138529,32.0014721641904,45.4040747194623));
#23400=CARTESIAN_POINT('Ctrl Pts',(34.0556201050794,32.0017900283843,44.6459252805377));
#23401=CARTESIAN_POINT('Ctrl Pts',(34.0568192254344,32.1329178655474,44.6530445351088));
#23402=CARTESIAN_POINT('Ctrl Pts',(33.9856535075787,32.9450400768571,44.6972070527531));
#23403=CARTESIAN_POINT('Ctrl Pts',(32.9043976941981,34.2539028108345,44.7784128334707));
#23404=CARTESIAN_POINT('Ctrl Pts',(30.5970084349764,33.9823288673751,44.8895426226904));
#23405=CARTESIAN_POINT('Ctrl Pts',(29.5736218412549,31.8965490419561,45.0006724119102));
#23406=CARTESIAN_POINT('Ctrl Pts',(30.7708302254411,29.9054464114596,45.1118022011299));
#23407=CARTESIAN_POINT('Ctrl Pts',(33.0929614575128,29.8312565107077,45.2229319903496));
#23408=CARTESIAN_POINT('Ctrl Pts',(34.0212425543896,31.1729921114884,45.3009730168189));
#23409=CARTESIAN_POINT('Ctrl Pts',(34.0577246468402,31.9260809170879,45.3419707802149));
#23410=CARTESIAN_POINT('Ctrl Pts',(34.0572107075264,31.9987715235836,45.3459252805377));
#23411=CARTESIAN_POINT('Origin',(32.,32.,39.4540747194623));
#23412=CARTESIAN_POINT('',(34.0514132135286,32.0000997951266,43.9459252805377));
#23413=CARTESIAN_POINT('',(34.0579022039251,31.9993577749783,44.0040747194624));
#23414=CARTESIAN_POINT('',(34.05475,32.0000000000002,39.4540747194623));
#23415=CARTESIAN_POINT('Ctrl Pts',(34.0579022039251,31.9993577749783,44.0040747194624));
#23416=CARTESIAN_POINT('Ctrl Pts',(34.0552574969039,32.6444368624799,44.0391993994564));
#23417=CARTESIAN_POINT('Ctrl Pts',(33.3810890294814,33.9745950606643,44.1113673425235));
#23418=CARTESIAN_POINT('Ctrl Pts',(31.1160444164971,34.2619981602002,44.2205785486641));
#23419=CARTESIAN_POINT('Ctrl Pts',(29.6201948806291,32.4842940678484,44.3317083378838));
#23420=CARTESIAN_POINT('Ctrl Pts',(30.3023171820977,30.2633692965589,44.4428381271035));
#23421=CARTESIAN_POINT('Ctrl Pts',(32.5381403879069,29.6317901120796,44.5539679163233));
#23422=CARTESIAN_POINT('Ctrl Pts',(33.9041700015856,30.8351942625182,44.6410467804428));
#23423=CARTESIAN_POINT('Ctrl Pts',(34.0541809189064,31.7583291084085,44.6910823814892));
#23424=CARTESIAN_POINT('Ctrl Pts',(34.0525927448309,31.9985307397491,44.7040747194623));
#23425=CARTESIAN_POINT('Ctrl Pts',(34.0514132135286,32.0000997951266,43.9459252805377));
#23426=CARTESIAN_POINT('Ctrl Pts',(34.0515591633093,32.3369356418003,43.9641182900027));
#23427=CARTESIAN_POINT('Ctrl Pts',(33.8137553478573,33.359417696568,44.0193545625409));
#23428=CARTESIAN_POINT('Ctrl Pts',(32.2023029113298,34.4201418557892,44.1116340981523));
#23429=CARTESIAN_POINT('Ctrl Pts',(30.0765281914199,33.4826561541886,44.2227638873721));
#23430=CARTESIAN_POINT('Ctrl Pts',(29.7110940115711,31.1882596190528,44.3338936765918));
#23431=CARTESIAN_POINT('Ctrl Pts',(31.4404417701646,29.6367590775809,44.4450234658115));
#23432=CARTESIAN_POINT('Ctrl Pts',(33.5382982520961,30.2089088165319,44.5490340004602));
#23433=CARTESIAN_POINT('Ctrl Pts',(34.0505799021566,31.4506269150344,44.6160012720355));
#23434=CARTESIAN_POINT('Ctrl Pts',(34.0556201050794,32.0017900283843,44.6459252805377));
#23435=CARTESIAN_POINT('Origin',(32.,32.,39.4540747194623));
#23436=CARTESIAN_POINT('',(34.0552538748384,31.9981575528908,43.2459252805377));
#23437=CARTESIAN_POINT('',(34.0544841229652,32.0018771151024,43.3040747194623));
#23438=CARTESIAN_POINT('',(34.05475,32.0000000000002,39.4540747194623));
#23439=CARTESIAN_POINT('Ctrl Pts',(34.0544841229652,32.0018771151024,43.3040747194623));
#23440=CARTESIAN_POINT('Ctrl Pts',(34.0560153379072,32.1707431770014,43.313229891277));
#23441=CARTESIAN_POINT('Ctrl Pts',(33.9597518572347,33.021145412764,43.3594283261648));
#23442=CARTESIAN_POINT('Ctrl Pts',(32.7795349847121,34.3000735544458,43.442670024126));
#23443=CARTESIAN_POINT('Ctrl Pts',(30.490493403277,33.9024728606777,43.5537998133457));
#23444=CARTESIAN_POINT('Ctrl Pts',(29.5829358892083,31.763749635471,43.6649296025654));
#23445=CARTESIAN_POINT('Ctrl Pts',(30.887449237386,29.8412401822595,43.7760593917852));
#23446=CARTESIAN_POINT('Ctrl Pts',(33.2101569783881,29.8944043032633,43.8871891810048));
#23447=CARTESIAN_POINT('Ctrl Pts',(34.0412598208513,31.2487125032873,43.9631942902306));
#23448=CARTESIAN_POINT('Ctrl Pts',(34.0580466633235,31.9641222134796,44.0021561363831));
#23449=CARTESIAN_POINT('Ctrl Pts',(34.0579022039251,31.9993577749783,44.0040747194624));
#23450=CARTESIAN_POINT('Ctrl Pts',(34.0552538748384,31.9981575528908,43.2459252805377));
#23451=CARTESIAN_POINT('Ctrl Pts',(34.0502763874237,32.5374622262668,43.2751920448965));
#23452=CARTESIAN_POINT('Ctrl Pts',(33.5565644973773,33.767436404629,43.3415020723287));
#23453=CARTESIAN_POINT('Ctrl Pts',(31.4823523987704,34.3727734903307,43.444855362834));
#23454=CARTESIAN_POINT('Ctrl Pts',(29.7258180926964,32.8521207213123,43.5559851520537));
#23455=CARTESIAN_POINT('Ctrl Pts',(30.0505904076267,30.5516163115282,43.6671149412734));
#23456=CARTESIAN_POINT('Ctrl Pts',(32.1594412400625,29.576656945096,43.7782447304932));
#23457=CARTESIAN_POINT('Ctrl Pts',(33.801022445043,30.6160471338321,43.8711815102479));
#23458=CARTESIAN_POINT('Ctrl Pts',(34.0512619911382,31.6510953521632,43.9270750269294));
#23459=CARTESIAN_POINT('Ctrl Pts',(34.0514132135286,32.0000997951266,43.9459252805377));
#23460=CARTESIAN_POINT('Origin',(32.,32.,39.4540747194623));
#23461=CARTESIAN_POINT('',(34.0574729334528,32.0010548525921,42.5459252805377));
#23462=CARTESIAN_POINT('',(34.0515269670353,31.9994876359477,42.6040747194623));
#23463=CARTESIAN_POINT('',(34.05475,32.0000000000002,39.4540747194623));
#23464=CARTESIAN_POINT('Ctrl Pts',(34.0515269670353,31.9994876359477,42.6040747194623));
#23465=CARTESIAN_POINT('Ctrl Pts',(34.0506912299639,32.3739658294889,42.6243036461709));
#23466=CARTESIAN_POINT('Ctrl Pts',(33.7733218574882,33.4353422112672,42.6815758359526));
#23467=CARTESIAN_POINT('Ctrl Pts',(32.0693858609145,34.4275911150555,42.7758912888076));
#23468=CARTESIAN_POINT('Ctrl Pts',(29.9981749928738,33.3750308454857,42.8870210780274));
#23469=CARTESIAN_POINT('Ctrl Pts',(29.7590126602339,31.0640572092229,42.9981508672471));
#23470=CARTESIAN_POINT('Ctrl Pts',(31.5707776395802,29.6096482896975,43.1092806564668));
#23471=CARTESIAN_POINT('Ctrl Pts',(33.5937426392217,30.2824590886342,43.2112552738719));
#23472=CARTESIAN_POINT('Ctrl Pts',(34.0498198017591,31.487484568456,43.2761866282037));
#23473=CARTESIAN_POINT('Ctrl Pts',(34.0544841229652,32.0018771151024,43.3040747194623));
#23474=CARTESIAN_POINT('Ctrl Pts',(34.0574729334528,32.0010548525921,42.5459252805377));
#23475=CARTESIAN_POINT('Ctrl Pts',(34.0578522481403,32.0616438352948,42.5492225367172));
#23476=CARTESIAN_POINT('Ctrl Pts',(34.0279453790661,32.8025443861859,42.5895630559699));
#23477=CARTESIAN_POINT('Ctrl Pts',(33.1311710776567,34.1490612048519,42.6669468382959));
#23478=CARTESIAN_POINT('Ctrl Pts',(30.8080907428172,34.1159786377566,42.7780766275156));
#23479=CARTESIAN_POINT('Ctrl Pts',(29.5758326061327,32.1463750685223,42.8892064167354));
#23480=CARTESIAN_POINT('Ctrl Pts',(30.5621462946373,30.0428107753347,43.0003362059551));
#23481=CARTESIAN_POINT('Ctrl Pts',(32.8643680431626,29.7304447592571,43.1114659951748));
#23482=CARTESIAN_POINT('Ctrl Pts',(33.9775551897302,31.0304040426633,43.1933290200357));
#23483=CARTESIAN_POINT('Ctrl Pts',(34.05657644757,31.8548584150789,43.2381487818233));
#23484=CARTESIAN_POINT('Ctrl Pts',(34.0552538748384,31.9981575528908,43.2459252805377));
#23485=CARTESIAN_POINT('Origin',(32.,32.,39.4540747194623));
#23486=CARTESIAN_POINT('',(34.0520872716434,32.0011660295939,41.8459252805377));
#23487=CARTESIAN_POINT('',(34.0563620767522,31.9983919833491,41.9040747194623));
#23488=CARTESIAN_POINT('',(34.05475,32.0000000000002,39.4540747194623));
#23489=CARTESIAN_POINT('Ctrl Pts',(34.0563620767522,31.9983919833491,41.9040747194623));
#23490=CARTESIAN_POINT('Ctrl Pts',(34.0514108779685,32.574410111975,41.9353774010647));
#23491=CARTESIAN_POINT('Ctrl Pts',(33.4988294551637,33.8404093508007,42.0037233457404));
#23492=CARTESIAN_POINT('Ctrl Pts',(31.3531125056534,34.3408422066741,42.1091125534892));
#23493=CARTESIAN_POINT('Ctrl Pts',(29.6825424018648,32.7262261662198,42.220242342709));
#23494=CARTESIAN_POINT('Ctrl Pts',(30.1328842256904,30.4469728946945,42.3313721319287));
#23495=CARTESIAN_POINT('Ctrl Pts',(32.2919902260347,29.5890346627002,42.4425019211484));
#23496=CARTESIAN_POINT('Ctrl Pts',(33.8394915366755,30.6921087455261,42.5334027836596));
#23497=CARTESIAN_POINT('Ctrl Pts',(34.0522216338574,31.6882203898806,42.5872603830976));
#23498=CARTESIAN_POINT('Ctrl Pts',(34.0515269670353,31.9994876359477,42.6040747194623));
#23499=CARTESIAN_POINT('Ctrl Pts',(34.0520872716434,32.0011660295939,41.8459252805377));
#23500=CARTESIAN_POINT('Ctrl Pts',(34.0534688437858,32.267023360204,41.860296291611));
#23501=CARTESIAN_POINT('Ctrl Pts',(33.8819549930642,33.2164555944441,41.9117105657577));
#23502=CARTESIAN_POINT('Ctrl Pts',(32.4498627820811,34.3865418359406,42.0001681029776));
#23503=CARTESIAN_POINT('Ctrl Pts',(30.2390335296879,33.6724274291408,42.1112978921972));
#23504=CARTESIAN_POINT('Ctrl Pts',(29.6398079512964,31.4277075354308,42.222427681417));
#23505=CARTESIAN_POINT('Ctrl Pts',(31.2006114825729,29.706752611882,42.3335574706367));
#23506=CARTESIAN_POINT('Ctrl Pts',(33.4249872180097,30.0733389095352,42.4413900036769));
#23507=CARTESIAN_POINT('Ctrl Pts',(34.053590809844,31.3809525260924,42.5121792736439));
#23508=CARTESIAN_POINT('Ctrl Pts',(34.0574729334528,32.0010548525921,42.5459252805377));
#23509=CARTESIAN_POINT('Origin',(32.,32.,39.4540747194623));
#23510=CARTESIAN_POINT('',(34.052676219088,31.9976391197374,41.1459252805377));
#23511=CARTESIAN_POINT('',(34.0565678449602,32.0014926321758,41.2040747194623));
#23512=CARTESIAN_POINT('',(34.05475,32.0000000000002,39.4540747194623));
#23513=CARTESIAN_POINT('',(32.5301702171886,30.0148256743283,41.));
#23514=CARTESIAN_POINT('Ctrl Pts',(32.5301702171886,30.0148256743283,41.));
#23515=CARTESIAN_POINT('Ctrl Pts',(33.1902397907527,30.1911070339301,41.0370432630732));
#23516=CARTESIAN_POINT('Ctrl Pts',(33.9249253440543,30.8871227497852,41.0856850232525));
#23517=CARTESIAN_POINT('Ctrl Pts',(34.0542945901694,31.7833429360997,41.1343267834317));
#23518=CARTESIAN_POINT('Ctrl Pts',(34.052676219088,31.9976391197375,41.1459252805377));
#23519=CARTESIAN_POINT('',(31.4686977725381,30.0112667465652,41.));
#23520=CARTESIAN_POINT('Origin',(32.,32.,41.));
#23521=CARTESIAN_POINT('Ctrl Pts',(31.4686971487471,30.0112647854283,41.));
#23522=CARTESIAN_POINT('Ctrl Pts',(32.1131668553171,29.8399814440384,41.0363148168372));
#23523=CARTESIAN_POINT('Ctrl Pts',(33.4928785396173,30.1592359611441,41.1043397233247));
#23524=CARTESIAN_POINT('Ctrl Pts',(34.0517137697956,31.4182664393509,41.1723646298121));
#23525=CARTESIAN_POINT('Ctrl Pts',(34.0565678449602,32.0014926321758,41.2040747194623));
#23526=CARTESIAN_POINT('Origin',(-32.,32.,48.));
#23527=CARTESIAN_POINT('',(-30.3315194671681,32.0006140847627,53.3285196366098));
#23528=CARTESIAN_POINT('',(-30.335188098255,32.0014849307108,53.5214803633902));
#23529=CARTESIAN_POINT('',(-30.334,32.,48.));
#23530=CARTESIAN_POINT('',(-32.6750771856749,30.4769022377466,54.));
#23531=CARTESIAN_POINT('Ctrl Pts',(-30.335188098255,32.0014849307108,53.5214803633902));
#23532=CARTESIAN_POINT('Ctrl Pts',(-30.3338369653803,32.1712283781921,53.5328138566338));
#23533=CARTESIAN_POINT('Ctrl Pts',(-30.3577131720504,32.3405890855005,53.5441473498775));
#23534=CARTESIAN_POINT('Ctrl Pts',(-30.4083948673629,32.5014829194567,53.5554808431211));
#23535=CARTESIAN_POINT('Ctrl Pts',(-30.5740468276277,33.027360730471,53.5925241061943));
#23536=CARTESIAN_POINT('Ctrl Pts',(-31.0260602822948,33.4627874201365,53.6295673692676));
#23537=CARTESIAN_POINT('Ctrl Pts',(-31.5578576126045,33.6090004762337,53.6666106323408));
#23538=CARTESIAN_POINT('Ctrl Pts',(-32.0896549429143,33.755213532331,53.7036538954141));
#23539=CARTESIAN_POINT('Ctrl Pts',(-32.7012361488668,33.61221295486,53.7406971584873));
#23540=CARTESIAN_POINT('Ctrl Pts',(-33.112224935063,33.2444451932609,53.7777404215606));
#23541=CARTESIAN_POINT('Ctrl Pts',(-33.5232137212592,32.8766774316618,53.8147836846338));
#23542=CARTESIAN_POINT('Ctrl Pts',(-33.7336100876993,32.2841424859346,53.851826947707));
#23543=CARTESIAN_POINT('Ctrl Pts',(-33.6481832846338,31.7403144028754,53.8888702107803));
#23544=CARTESIAN_POINT('Ctrl Pts',(-33.5627564815683,31.1964863198163,53.9259134738535));
#23545=CARTESIAN_POINT('Ctrl Pts',(-33.1815065089974,30.7013650994253,53.9629567369268));
#23546=CARTESIAN_POINT('Ctrl Pts',(-32.6750771856749,30.4769022377466,54.));
#23547=CARTESIAN_POINT('',(-30.334,32.,54.));
#23548=CARTESIAN_POINT('Origin',(-32.,32.,54.));
#23549=CARTESIAN_POINT('',(-30.334,32.,55.));
#23550=CARTESIAN_POINT('',(-30.334,32.,48.));
#23551=CARTESIAN_POINT('Origin',(-32.,32.,55.));
#23552=CARTESIAN_POINT('',(-30.3853283554254,31.5775322576866,54.));
#23553=CARTESIAN_POINT('Origin',(-32.,32.,54.));
#23554=CARTESIAN_POINT('Ctrl Pts',(-30.3853267261146,31.5775319120267,54.));
#23555=CARTESIAN_POINT('Ctrl Pts',(-30.5228595194004,31.054637565178,53.9636851831627));
#23556=CARTESIAN_POINT('Ctrl Pts',(-30.9381524315377,30.6037762063905,53.9273703663255));
#23557=CARTESIAN_POINT('Ctrl Pts',(-31.4484748501057,30.4251375769901,53.8910555494883));
#23558=CARTESIAN_POINT('Ctrl Pts',(-31.969033929005,30.2429155992892,53.8540122864151));
#23559=CARTESIAN_POINT('Ctrl Pts',(-32.5884731835828,30.343947026941,53.8169690233418));
#23560=CARTESIAN_POINT('Ctrl Pts',(-33.0238322854568,30.6822522289001,53.7799257602686));
#23561=CARTESIAN_POINT('Ctrl Pts',(-33.4591913873308,31.0205574308592,53.7428824971953));
#23562=CARTESIAN_POINT('Ctrl Pts',(-33.7104703365009,31.5961364071255,53.7058392341221));
#23563=CARTESIAN_POINT('Ctrl Pts',(-33.6624375910167,32.145481024569,53.6687959710488));
#23564=CARTESIAN_POINT('Ctrl Pts',(-33.6144048455325,32.6948256420124,53.6317527079756));
#23565=CARTESIAN_POINT('Ctrl Pts',(-33.267060405394,33.2179359006329,53.5947094449024));
#23566=CARTESIAN_POINT('Ctrl Pts',(-32.7794722527579,33.4755031203564,53.5576661818291));
#23567=CARTESIAN_POINT('Ctrl Pts',(-32.2918841001217,33.7330703400798,53.5206229187559));
#23568=CARTESIAN_POINT('Ctrl Pts',(-31.6640522349879,33.7250945209062,53.4835796556826));
#23569=CARTESIAN_POINT('Ctrl Pts',(-31.1832059468561,33.4551931614016,53.4465363926094));
#23570=CARTESIAN_POINT('Ctrl Pts',(-30.7023596587244,33.1852918018969,53.4094931295361));
#23571=CARTESIAN_POINT('Ctrl Pts',(-30.3684989475947,32.6534649020614,53.3724498664629));
#23572=CARTESIAN_POINT('Ctrl Pts',(-30.3344285753632,32.1030898303843,53.3354066033897));
#23573=CARTESIAN_POINT('Ctrl Pts',(-30.3323171566033,32.0689818305247,53.3331109477964));
#23574=CARTESIAN_POINT('Ctrl Pts',(-30.3313571017956,32.0348025952259,53.3308152922031));
#23575=CARTESIAN_POINT('Ctrl Pts',(-30.3315194671681,32.0006140847627,53.3285196366098));
#23576=CARTESIAN_POINT('Origin',(-32.,32.,48.));
#23577=CARTESIAN_POINT('',(-30.3358699394038,32.0011304355222,52.6285196366098));
#23578=CARTESIAN_POINT('',(-30.3362229430458,31.9991035479857,52.8214803633902));
#23579=CARTESIAN_POINT('',(-30.334,32.,48.));
#23580=CARTESIAN_POINT('Ctrl Pts',(-30.3362229430458,31.9991035479857,52.8214803633902));
#23581=CARTESIAN_POINT('Ctrl Pts',(-30.3378663531425,32.3352311359495,52.8438876115277));
#23582=CARTESIAN_POINT('Ctrl Pts',(-30.4366434498682,32.6722466504923,52.8662948596652));
#23583=CARTESIAN_POINT('Ctrl Pts',(-30.6259117277904,32.9469019296561,52.8887021078027));
#23584=CARTESIAN_POINT('Ctrl Pts',(-30.9388066699745,33.400957139742,52.925745370876));
#23585=CARTESIAN_POINT('Ctrl Pts',(-31.4990150314079,33.6845811229079,52.9627886339492));
#23586=CARTESIAN_POINT('Ctrl Pts',(-32.0501928386486,33.6679971146088,52.9998318970225));
#23587=CARTESIAN_POINT('Ctrl Pts',(-32.6013706458894,33.6514131063097,53.0368751600957));
#23588=CARTESIAN_POINT('Ctrl Pts',(-33.1435178989375,33.3346211065456,53.0739184231689));
#23589=CARTESIAN_POINT('Ctrl Pts',(-33.4285423718774,32.862567514634,53.1109616862422));
#23590=CARTESIAN_POINT('Ctrl Pts',(-33.7135668448172,32.3905139227225,53.1480049493154));
#23591=CARTESIAN_POINT('Ctrl Pts',(-33.7414685376489,31.7631987386633,53.1850482123887));
#23592=CARTESIAN_POINT('Ctrl Pts',(-33.4994967785869,31.2677094716929,53.222091475462));
#23593=CARTESIAN_POINT('Ctrl Pts',(-33.2575250195249,30.7722202047225,53.2591347385352));
#23594=CARTESIAN_POINT('Ctrl Pts',(-32.7456798085692,30.4085568548408,53.2961780016084));
#23595=CARTESIAN_POINT('Ctrl Pts',(-32.1981450993846,30.3430674696929,53.3332212646816));
#23596=CARTESIAN_POINT('Ctrl Pts',(-31.6506103901999,30.2775780845449,53.3702645277548));
#23597=CARTESIAN_POINT('Ctrl Pts',(-31.0673861827863,30.5102626641308,53.4073077908281));
#23598=CARTESIAN_POINT('Ctrl Pts',(-30.7154193120108,30.9347694201052,53.4443510539014));
#23599=CARTESIAN_POINT('Ctrl Pts',(-30.4711377211209,31.2293971089682,53.470060823731));
#23600=CARTESIAN_POINT('Ctrl Pts',(-30.3382531122335,31.6164258080716,53.4957705935606));
#23601=CARTESIAN_POINT('Ctrl Pts',(-30.335188098255,32.0014849307108,53.5214803633902));
#23602=CARTESIAN_POINT('Ctrl Pts',(-30.3315194671681,32.0006140847627,53.3285196366098));
#23603=CARTESIAN_POINT('Ctrl Pts',(-30.3339770693666,31.4831283846537,53.2937720291299));
#23604=CARTESIAN_POINT('Ctrl Pts',(-30.5935878007645,30.9635176892697,53.2590244216499));
#23605=CARTESIAN_POINT('Ctrl Pts',(-31.0099803387083,30.6566480755526,53.2242768141699));
#23606=CARTESIAN_POINT('Ctrl Pts',(-31.4538825076184,30.3295046359168,53.1872335510967));
#23607=CARTESIAN_POINT('Ctrl Pts',(-32.0759668787719,30.2441410001639,53.1501902880235));
#23608=CARTESIAN_POINT('Ctrl Pts',(-32.5915791609355,30.4396232555466,53.1131470249502));
#23609=CARTESIAN_POINT('Ctrl Pts',(-33.1071914430991,30.6351055109293,53.076103761877));
#23610=CARTESIAN_POINT('Ctrl Pts',(-33.5163316362729,31.1114336574476,53.0390604988037));
#23611=CARTESIAN_POINT('Ctrl Pts',(-33.6317752923808,31.6506404213303,53.0020172357305));
#23612=CARTESIAN_POINT('Ctrl Pts',(-33.7472189484887,32.1898471852129,52.9649739726572));
#23613=CARTESIAN_POINT('Ctrl Pts',(-33.5689660675308,32.7919325664598,52.927930709584));
#23614=CARTESIAN_POINT('Ctrl Pts',(-33.1785862796925,33.1813866185031,52.8908874465107));
#23615=CARTESIAN_POINT('Ctrl Pts',(-32.7882064918542,33.5708406705464,52.8538441834375));
#23616=CARTESIAN_POINT('Ctrl Pts',(-32.1856997971356,33.7476633933861,52.8168009203643));
#23617=CARTESIAN_POINT('Ctrl Pts',(-31.6467689421153,33.6309411327337,52.779757657291));
#23618=CARTESIAN_POINT('Ctrl Pts',(-31.1078380870949,33.5142188720812,52.7427143942178));
#23619=CARTESIAN_POINT('Ctrl Pts',(-30.6324830717728,33.1039516279366,52.7056711311445));
#23620=CARTESIAN_POINT('Ctrl Pts',(-30.4382243040802,32.5878757369611,52.6686278680713));
#23621=CARTESIAN_POINT('Ctrl Pts',(-30.3681137093176,32.4016170260225,52.6552584575841));
#23622=CARTESIAN_POINT('Ctrl Pts',(-30.3346182876945,32.2015758403761,52.641889047097));
#23623=CARTESIAN_POINT('Ctrl Pts',(-30.3358699394038,32.0011304355222,52.6285196366098));
#23624=CARTESIAN_POINT('Origin',(-32.,32.,48.));
#23625=CARTESIAN_POINT('',(-30.3356164568928,31.9987501844668,51.9285196366098));
#23626=CARTESIAN_POINT('',(-30.3318747561565,31.9990863473369,52.1214803633902));
#23627=CARTESIAN_POINT('',(-30.334,32.,48.));
#23628=CARTESIAN_POINT('Ctrl Pts',(-30.3318747561565,31.9990863473369,52.1214803633902));
#23629=CARTESIAN_POINT('Ctrl Pts',(-30.3351692730374,32.4979846805671,52.1549613664216));
#23630=CARTESIAN_POINT('Ctrl Pts',(-30.573848791373,32.9996174235339,52.188442369453));
#23631=CARTESIAN_POINT('Ctrl Pts',(-30.9647448495809,33.3088117421955,52.2219233724844));
#23632=CARTESIAN_POINT('Ctrl Pts',(-31.3972308627662,33.6509032403563,52.2589666355576));
#23633=CARTESIAN_POINT('Ctrl Pts',(-32.0160471389214,33.7574283392523,52.2960098986309));
#23634=CARTESIAN_POINT('Ctrl Pts',(-32.5380267774666,33.5796418646352,52.3330531617041));
#23635=CARTESIAN_POINT('Ctrl Pts',(-33.0600064160119,33.4018553900181,52.3700964247773));
#23636=CARTESIAN_POINT('Ctrl Pts',(-33.4851494169471,32.939757341888,52.4071396878506));
#23637=CARTESIAN_POINT('Ctrl Pts',(-33.6189125057485,32.4048010173491,52.4441829509238));
#23638=CARTESIAN_POINT('Ctrl Pts',(-33.7526755945498,31.8698446928101,52.4812262139971));
#23639=CARTESIAN_POINT('Ctrl Pts',(-33.5950587712171,31.2620300918623,52.5182694770703));
#23640=CARTESIAN_POINT('Ctrl Pts',(-33.2181869216583,30.8594904030147,52.5553127401436));
#23641=CARTESIAN_POINT('Ctrl Pts',(-32.8413150720994,30.4569507141672,52.5923560032168));
#23642=CARTESIAN_POINT('Ctrl Pts',(-32.2451881963143,30.2596859374199,52.62939926629));
#23643=CARTESIAN_POINT('Ctrl Pts',(-31.702590161623,30.3579623298606,52.6664425293633));
#23644=CARTESIAN_POINT('Ctrl Pts',(-31.1599921269317,30.4562387223013,52.7034857924365));
#23645=CARTESIAN_POINT('Ctrl Pts',(-30.6709229333342,30.85005628393,52.7405290555098));
#23646=CARTESIAN_POINT('Ctrl Pts',(-30.4591790980028,31.3592082832473,52.777572318583));
#23647=CARTESIAN_POINT('Ctrl Pts',(-30.3755178414248,31.5603772853363,52.7922083335188));
#23648=CARTESIAN_POINT('Ctrl Pts',(-30.3351494968746,31.7795510010796,52.8068443484545));
#23649=CARTESIAN_POINT('Ctrl Pts',(-30.3362229430458,31.9991035479857,52.8214803633902));
#23650=CARTESIAN_POINT('Ctrl Pts',(-30.3358699394038,32.0011304355222,52.6285196366098));
#23651=CARTESIAN_POINT('Ctrl Pts',(-30.3380862987625,31.6461922001661,52.6048457840237));
#23652=CARTESIAN_POINT('Ctrl Pts',(-30.4492537515405,31.289986516348,52.5811719314377));
#23653=CARTESIAN_POINT('Ctrl Pts',(-30.6590001159673,31.0067929794516,52.5574980788516));
#23654=CARTESIAN_POINT('Ctrl Pts',(-30.9871972156101,30.5636706507241,52.5204548157783));
#23655=CARTESIAN_POINT('Ctrl Pts',(-31.5567539349585,30.2993105310754,52.4834115527051));
#23656=CARTESIAN_POINT('Ctrl Pts',(-32.1070443429008,30.3346824468124,52.4463682896318));
#23657=CARTESIAN_POINT('Ctrl Pts',(-32.657334750843,30.3700543625495,52.4093250265586));
#23658=CARTESIAN_POINT('Ctrl Pts',(-33.1883588473791,30.7051583136722,52.3722817634854));
#23659=CARTESIAN_POINT('Ctrl Pts',(-33.4571228169063,31.1866525143206,52.3352385004121));
#23660=CARTESIAN_POINT('Ctrl Pts',(-33.7258867864335,31.668146714969,52.2981952373389));
#23661=CARTESIAN_POINT('Ctrl Pts',(-33.7323906289517,32.2960311651429,52.2611519742656));
#23662=CARTESIAN_POINT('Ctrl Pts',(-33.4736582559377,32.7829893626111,52.2241087111924));
#23663=CARTESIAN_POINT('Ctrl Pts',(-33.2149258829237,33.2699475600792,52.1870654481191));
#23664=CARTESIAN_POINT('Ctrl Pts',(-32.6909572943775,33.6159795048416,52.1500221850459));
#23665=CARTESIAN_POINT('Ctrl Pts',(-32.1415176578637,33.6627428463605,52.1129789219727));
#23666=CARTESIAN_POINT('Ctrl Pts',(-31.5920780213499,33.7095061878793,52.0759356588994));
#23667=CARTESIAN_POINT('Ctrl Pts',(-31.0171673368685,33.4570009261547,52.0388923958262));
#23668=CARTESIAN_POINT('Ctrl Pts',(-30.6798616251316,33.0207721042924,52.0018491327529));
#23669=CARTESIAN_POINT('Ctrl Pts',(-30.4572889192754,32.7329245349333,51.9774059673719));
#23670=CARTESIAN_POINT('Ctrl Pts',(-30.3381713232652,32.3650822547069,51.9529628019909));
#23671=CARTESIAN_POINT('Ctrl Pts',(-30.3356164568928,31.9987501844668,51.9285196366098));
#23672=CARTESIAN_POINT('Origin',(-32.,32.,48.));
#23673=CARTESIAN_POINT('',(-30.3313738111782,31.9995820848862,51.2285196366098));
#23674=CARTESIAN_POINT('',(-30.3334713021565,32.0014789858971,51.4214803633902));
#23675=CARTESIAN_POINT('',(-30.334,32.,48.));
#23676=CARTESIAN_POINT('Ctrl Pts',(-30.3334713021565,32.0014789858971,51.4214803633902));
#23677=CARTESIAN_POINT('Ctrl Pts',(-30.3324380493541,32.1136863614967,51.4289918582422));
#23678=CARTESIAN_POINT('Ctrl Pts',(-30.3428029813185,32.22570392951,51.4365033530943));
#23679=CARTESIAN_POINT('Ctrl Pts',(-30.3652660205241,32.3352404972475,51.4440148479463));
#23680=CARTESIAN_POINT('Ctrl Pts',(-30.4760434738951,32.8754248380169,51.4810581110195));
#23681=CARTESIAN_POINT('Ctrl Pts',(-30.8810483542085,33.3552709529063,51.5181013740927));
#23682=CARTESIAN_POINT('Ctrl Pts',(-31.3949526236766,33.5552038604804,51.555144637166));
#23683=CARTESIAN_POINT('Ctrl Pts',(-31.9088568931446,33.7551367680545,51.5921879002392));
#23684=CARTESIAN_POINT('Ctrl Pts',(-32.5316605517672,33.6751564683133,51.6292311633125));
#23685=CARTESIAN_POINT('Ctrl Pts',(-32.9783720235667,33.3518615149587,51.6662744263858));
#23686=CARTESIAN_POINT('Ctrl Pts',(-33.4250834953661,33.0285665616042,51.703317689459));
#23687=CARTESIAN_POINT('Ctrl Pts',(-33.6957027803424,32.4619569546363,51.7403609525322));
#23688=CARTESIAN_POINT('Ctrl Pts',(-33.666395958695,31.9113101735047,51.7774042156054));
#23689=CARTESIAN_POINT('Ctrl Pts',(-33.6370891370477,31.3606633923732,51.8144474786787));
#23690=CARTESIAN_POINT('Ctrl Pts',(-33.3078562087767,30.8259794370781,51.851490741752));
#23691=CARTESIAN_POINT('Ctrl Pts',(-32.8293523813543,30.5519267950428,51.8885340048252));
#23692=CARTESIAN_POINT('Ctrl Pts',(-32.350848553932,30.2778741530076,51.9255772678985));
#23693=CARTESIAN_POINT('Ctrl Pts',(-31.7230738273582,30.2644528242322,51.9626205309717));
#23694=CARTESIAN_POINT('Ctrl Pts',(-31.233294503268,30.5178043187989,51.9996637940449));
#23695=CARTESIAN_POINT('Ctrl Pts',(-30.7435151791779,30.7711558133657,52.0367070571181));
#23696=CARTESIAN_POINT('Ctrl Pts',(-30.3917312575714,31.2912801312746,52.0737503201914));
#23697=CARTESIAN_POINT('Ctrl Pts',(-30.3389171718758,31.8401712389419,52.1107935832646));
#23698=CARTESIAN_POINT('Ctrl Pts',(-30.3338383129549,31.8929552730132,52.1143558433065));
#23699=CARTESIAN_POINT('Ctrl Pts',(-30.3315242312385,31.9460053331347,52.1179181033484));
#23700=CARTESIAN_POINT('Ctrl Pts',(-30.3318747561565,31.9990863473369,52.1214803633902));
#23701=CARTESIAN_POINT('Ctrl Pts',(-30.3356164568928,31.9987501844668,51.9285196366098));
#23702=CARTESIAN_POINT('Ctrl Pts',(-30.3342994602853,31.8099113086153,51.9159195389176));
#23703=CARTESIAN_POINT('Ctrl Pts',(-30.3639561318528,31.6214737337898,51.9033194412254));
#23704=CARTESIAN_POINT('Ctrl Pts',(-30.4263819212587,31.4446018044738,51.8907193435332));
#23705=CARTESIAN_POINT('Ctrl Pts',(-30.609908668115,30.9246127085175,51.85367608046));
#23706=CARTESIAN_POINT('Ctrl Pts',(-31.0766629008198,30.5045868986048,51.8166328173867));
#23707=CARTESIAN_POINT('Ctrl Pts',(-31.613060415607,30.3767259090036,51.7795895543135));
#23708=CARTESIAN_POINT('Ctrl Pts',(-32.1494579303943,30.2488649194023,51.7425462912402));
#23709=CARTESIAN_POINT('Ctrl Pts',(-32.7554987272639,30.4131687501125,51.705503028167));
#23710=CARTESIAN_POINT('Ctrl Pts',(-33.1538618225511,30.7944528585221,51.6684597650938));
#23711=CARTESIAN_POINT('Ctrl Pts',(-33.5522249178383,31.1757369669317,51.6314165020206));
#23712=CARTESIAN_POINT('Ctrl Pts',(-33.742910311543,31.7740013530409,51.5943732389473));
#23713=CARTESIAN_POINT('Ctrl Pts',(-33.6386614020287,32.3154834780122,51.557329975874));
#23714=CARTESIAN_POINT('Ctrl Pts',(-33.5344124925144,32.8569656029835,51.5202867128008));
#23715=CARTESIAN_POINT('Ctrl Pts',(-33.1352292797811,33.341665466817,51.4832434497276));
#23716=CARTESIAN_POINT('Ctrl Pts',(-32.6237758372046,33.5477870398502,51.4462001866543));
#23717=CARTESIAN_POINT('Ctrl Pts',(-32.1123223946281,33.7539086128834,51.4091569235811));
#23718=CARTESIAN_POINT('Ctrl Pts',(-31.4885987222084,33.6814518951163,51.3721136605078));
#23719=CARTESIAN_POINT('Ctrl Pts',(-31.0380173905906,33.3635726877936,51.3350703974346));
#23720=CARTESIAN_POINT('Ctrl Pts',(-30.6060019603948,33.0587914799067,51.2995534771596));
#23721=CARTESIAN_POINT('Ctrl Pts',(-30.3331544035574,32.5283960429641,51.2640365568847));
#23722=CARTESIAN_POINT('Ctrl Pts',(-30.3313738111782,31.9995820848862,51.2285196366098));
#23723=CARTESIAN_POINT('Origin',(-32.,32.,48.));
#23724=CARTESIAN_POINT('',(-30.3343902510906,32.0015149949486,50.5285196366098));
#23725=CARTESIAN_POINT('',(-30.3367088771406,31.9999843288602,50.7214803633902));
#23726=CARTESIAN_POINT('',(-30.334,32.,48.));
#23727=CARTESIAN_POINT('Ctrl Pts',(-30.3367088771406,31.9999843288602,50.7214803633902));
#23728=CARTESIAN_POINT('Ctrl Pts',(-30.3367322875339,32.2789818929087,50.7400656131361));
#23729=CARTESIAN_POINT('Ctrl Pts',(-30.4031501600345,32.5579899313227,50.758650862882));
#23730=CARTESIAN_POINT('Ctrl Pts',(-30.5359003296719,32.800720631568,50.777236112628));
#23731=CARTESIAN_POINT('Ctrl Pts',(-30.8004918484369,33.2845202741914,50.8142793757012));
#23732=CARTESIAN_POINT('Ctrl Pts',(-31.328599195375,33.624202296529,50.8513226387744));
#23733=CARTESIAN_POINT('Ctrl Pts',(-31.8785633120601,33.6643300469896,50.8883659018476));
#23734=CARTESIAN_POINT('Ctrl Pts',(-32.4285274287452,33.7044577974502,50.9254091649209));
#23735=CARTESIAN_POINT('Ctrl Pts',(-33.0003483151774,33.4450312760337,50.9624524279942));
#23736=CARTESIAN_POINT('Ctrl Pts',(-33.3323638343148,33.0047626522954,50.9994956910674));
#23737=CARTESIAN_POINT('Ctrl Pts',(-33.6643793534521,32.5644940285572,51.0365389541407));
#23738=CARTESIAN_POINT('Ctrl Pts',(-33.7565895052947,31.9433833024971,51.0735822172138));
#23739=CARTESIAN_POINT('Ctrl Pts',(-33.5667994243086,31.4256473744548,51.1106254802871));
#23740=CARTESIAN_POINT('Ctrl Pts',(-33.3770093433226,30.9079114464125,51.1476687433603));
#23741=CARTESIAN_POINT('Ctrl Pts',(-32.9052190295081,30.4935503163879,51.1847120064336));
#23742=CARTESIAN_POINT('Ctrl Pts',(-32.3673171723679,30.3721733908449,51.2217552695068));
#23743=CARTESIAN_POINT('Ctrl Pts',(-31.8294153152277,30.2507964653019,51.2587985325801));
#23744=CARTESIAN_POINT('Ctrl Pts',(-31.2254019147619,30.4224037442404,51.2958417956533));
#23745=CARTESIAN_POINT('Ctrl Pts',(-30.8316702277433,30.8084686670345,51.3328850587265));
#23746=CARTESIAN_POINT('Ctrl Pts',(-30.5177779850596,31.1162487833744,51.3624168269478));
#23747=CARTESIAN_POINT('Ctrl Pts',(-30.3375335804213,31.5603308157666,51.391948595169));
#23748=CARTESIAN_POINT('Ctrl Pts',(-30.3334713021565,32.0014789858971,51.4214803633902));
#23749=CARTESIAN_POINT('Ctrl Pts',(-30.3313738111782,31.9995820848862,51.2285196366098));
#23750=CARTESIAN_POINT('Ctrl Pts',(-30.3312972900628,31.9768562581447,51.2269932938115));
#23751=CARTESIAN_POINT('Ctrl Pts',(-30.3317213912061,31.9541333521705,51.2254669510132));
#23752=CARTESIAN_POINT('Ctrl Pts',(-30.3326549959156,31.9314313992364,51.2239406082148));
#23753=CARTESIAN_POINT('Ctrl Pts',(-30.3553129236745,31.38047101488,51.1868973451416));
#23754=CARTESIAN_POINT('Ctrl Pts',(-30.6780677700083,30.8418519430456,51.1498540820683));
#23755=CARTESIAN_POINT('Ctrl Pts',(-31.1532286673374,30.5620433504833,51.1128108189951));
#23756=CARTESIAN_POINT('Ctrl Pts',(-31.6283895646664,30.2822347579209,51.0757675559219));
#23757=CARTESIAN_POINT('Ctrl Pts',(-32.2559565129908,30.2612366446307,51.0387242928487));
#23758=CARTESIAN_POINT('Ctrl Pts',(-32.7487582795783,30.5086576333871,51.0016810297754));
#23759=CARTESIAN_POINT('Ctrl Pts',(-33.2415600461658,30.7560786221434,50.9646377667022));
#23760=CARTESIAN_POINT('Ctrl Pts',(-33.5995966310166,31.2719187129463,50.9275945036289));
#23761=CARTESIAN_POINT('Ctrl Pts',(-33.659032434285,31.8201322772756,50.8905512405557));
#23762=CARTESIAN_POINT('Ctrl Pts',(-33.7184682375533,32.3683458416049,50.8535079774824));
#23763=CARTESIAN_POINT('Ctrl Pts',(-33.4793032592393,32.9489328794607,50.8164647144092));
#23764=CARTESIAN_POINT('Ctrl Pts',(-33.0509780965965,33.2962199104198,50.7794214513359));
#23765=CARTESIAN_POINT('Ctrl Pts',(-32.6226529339536,33.6435069413789,50.7423781882627));
#23766=CARTESIAN_POINT('Ctrl Pts',(-32.005167586982,33.7574939654412,50.7053349251895));
#23767=CARTESIAN_POINT('Ctrl Pts',(-31.4810800022833,33.5860211384661,50.6682916621163));
#23768=CARTESIAN_POINT('Ctrl Pts',(-30.9569924175846,33.414548311491,50.631248399043));
#23769=CARTESIAN_POINT('Ctrl Pts',(-30.5263025951589,32.9576156334784,50.5942051359698));
#23770=CARTESIAN_POINT('Ctrl Pts',(-30.3860918624286,32.4243130202719,50.5571618728965));
#23771=CARTESIAN_POINT('Ctrl Pts',(-30.3499543968131,32.2868613111755,50.5476144608009));
#23772=CARTESIAN_POINT('Ctrl Pts',(-30.3331129511714,32.1443364803049,50.5380670487054));
#23773=CARTESIAN_POINT('Ctrl Pts',(-30.3343902510906,32.0015149949486,50.5285196366098));
#23774=CARTESIAN_POINT('Origin',(-32.,32.,48.));
#23775=CARTESIAN_POINT('',(-30.3365646132776,31.9994923926615,49.8285196366098));
#23776=CARTESIAN_POINT('',(-30.3334137894091,31.9985292433869,50.0214803633902));
#23777=CARTESIAN_POINT('',(-30.334,32.,48.));
#23778=CARTESIAN_POINT('Ctrl Pts',(-30.3334137894091,31.9985292433869,50.0214803633902));
#23779=CARTESIAN_POINT('Ctrl Pts',(-30.3374859553988,32.4415387450404,50.05113936803));
#23780=CARTESIAN_POINT('Ctrl Pts',(-30.5194576726712,32.8875030130583,50.0807983726698));
#23781=CARTESIAN_POINT('Ctrl Pts',(-30.8357595188381,33.195527279696,50.1104573773096));
#23782=CARTESIAN_POINT('Ctrl Pts',(-31.2308116333785,33.5802409300893,50.1475006403828));
#23783=CARTESIAN_POINT('Ctrl Pts',(-31.835409450851,33.7497777263432,50.184543903456));
#23784=CARTESIAN_POINT('Ctrl Pts',(-32.3728922882751,33.6265585497666,50.2215871665293));
#23785=CARTESIAN_POINT('Ctrl Pts',(-32.9103751256992,33.50333937319,50.2586304296025));
#23786=CARTESIAN_POINT('Ctrl Pts',(-33.380742983075,33.087364223783,50.2956736926758));
#23787=CARTESIAN_POINT('Ctrl Pts',(-33.5687580793311,32.5689810743834,50.332716955749));
#23788=CARTESIAN_POINT('Ctrl Pts',(-33.7567731755871,32.0505979249839,50.3697602188223));
#23789=CARTESIAN_POINT('Ctrl Pts',(-33.6624355107235,31.4298067755918,50.4068034818955));
#23790=CARTESIAN_POINT('Ctrl Pts',(-33.3289134886565,30.990678290068,50.4438467449687));
#23791=CARTESIAN_POINT('Ctrl Pts',(-32.9953914665895,30.5515498045442,50.480890008042));
#23792=CARTESIAN_POINT('Ctrl Pts',(-32.422685087319,30.2940839828886,50.5179332711152));
#23793=CARTESIAN_POINT('Ctrl Pts',(-31.8728616846295,30.3360957890429,50.5549765341885));
#23794=CARTESIAN_POINT('Ctrl Pts',(-31.3230382819401,30.3781075951973,50.5920197972617));
#23795=CARTESIAN_POINT('Ctrl Pts',(-30.7960978558316,30.7195970291617,50.629063060335));
#23796=CARTESIAN_POINT('Ctrl Pts',(-30.5331654880733,31.2043003775985,50.6661063234082));
#23797=CARTESIAN_POINT('Ctrl Pts',(-30.4021508650182,31.4458196208563,50.6845643367355));
#23798=CARTESIAN_POINT('Ctrl Pts',(-30.3366856270171,31.7228968091386,50.7030223500629));
#23799=CARTESIAN_POINT('Ctrl Pts',(-30.3367088771406,31.9999843288602,50.7214803633902));
#23800=CARTESIAN_POINT('Ctrl Pts',(-30.3343902510906,32.0015149949486,50.5285196366098));
#23801=CARTESIAN_POINT('Ctrl Pts',(-30.3380687817627,31.5901995265833,50.5010237856321));
#23802=CARTESIAN_POINT('Ctrl Pts',(-30.4920238292037,31.1764236117912,50.4735279346544));
#23803=CARTESIAN_POINT('Ctrl Pts',(-30.7681349479738,30.8742782274076,50.4460320836768));
#23804=CARTESIAN_POINT('Ctrl Pts',(-31.1401204092839,30.4672185961501,50.4089888206035));
#23805=CARTESIAN_POINT('Ctrl Pts',(-31.7338229749391,30.2627718820353,50.3719455575303));
#23806=CARTESIAN_POINT('Ctrl Pts',(-32.2775675701133,30.3544917928758,50.334902294457));
#23807=CARTESIAN_POINT('Ctrl Pts',(-32.8213121652876,30.4462117037163,50.2978590313838));
#23808=CARTESIAN_POINT('Ctrl Pts',(-33.3150987899808,30.8340982395122,50.2608157683106));
#23809=CARTESIAN_POINT('Ctrl Pts',(-33.53297336218,31.3406566247105,50.2237725052373));
#23810=CARTESIAN_POINT('Ctrl Pts',(-33.7508479343793,31.8472150099088,50.1867292421641));
#23811=CARTESIAN_POINT('Ctrl Pts',(-33.6928104540846,32.4724452445095,50.1496859790908));
#23812=CARTESIAN_POINT('Ctrl Pts',(-33.3854185575835,32.930245363329,50.1126427160176));
#23813=CARTESIAN_POINT('Ctrl Pts',(-33.0780266610825,33.3880454821486,50.0755994529444));
#23814=CARTESIAN_POINT('Ctrl Pts',(-32.521280348375,33.678415485187,50.0385561898711));
#23815=CARTESIAN_POINT('Ctrl Pts',(-31.9699437133251,33.6684836335197,50.0015129267979));
#23816=CARTESIAN_POINT('Ctrl Pts',(-31.4186070782752,33.6585517818524,49.9644696637246));
#23817=CARTESIAN_POINT('Ctrl Pts',(-30.8726801208827,33.3483180754794,49.9274264006514));
#23818=CARTESIAN_POINT('Ctrl Pts',(-30.5819760566847,32.8797437762647,49.8903831375782));
#23819=CARTESIAN_POINT('Ctrl Pts',(-30.4201475201305,32.6188988055621,49.8697619705887));
#23820=CARTESIAN_POINT('Ctrl Pts',(-30.3374100869024,32.3089856183198,49.8491408035992));
#23821=CARTESIAN_POINT('Ctrl Pts',(-30.3365646132776,31.9994923926615,49.8285196366098));
#23822=CARTESIAN_POINT('Origin',(-32.,32.,48.));
#23823=CARTESIAN_POINT('',(-30.3325307394052,31.9987546512789,49.1285196366098));
#23824=CARTESIAN_POINT('',(-30.3319159461724,32.0009409208263,49.3214803633902));
#23825=CARTESIAN_POINT('',(-30.334,32.,48.));
#23826=CARTESIAN_POINT('Ctrl Pts',(-30.3319159461724,32.0009409208263,49.3214803633902));
#23827=CARTESIAN_POINT('Ctrl Pts',(-30.33154425979,32.0559214513191,49.3251698598506));
#23828=CARTESIAN_POINT('Ctrl Pts',(-30.3340269899209,32.1108680039687,49.3288593563111));
#23829=CARTESIAN_POINT('Ctrl Pts',(-30.3394745332028,32.1655190278833,49.3325488527715));
#23830=CARTESIAN_POINT('Ctrl Pts',(-30.3941689287825,32.7142259524741,49.3695921158447));
#23831=CARTESIAN_POINT('Ctrl Pts',(-30.747732829251,33.2331419519015,49.406635378918));
#23832=CARTESIAN_POINT('Ctrl Pts',(-31.2383773108745,33.4848138785325,49.4436786419912));
#23833=CARTESIAN_POINT('Ctrl Pts',(-31.729021792498,33.7364858051635,49.4807219050645));
#23834=CARTESIAN_POINT('Ctrl Pts',(-32.3567468552764,33.7209136589979,49.5177651681377));
#23835=CARTESIAN_POINT('Ctrl Pts',(-32.8343089141797,33.4452231696848,49.5548084312109));
#23836=CARTESIAN_POINT('Ctrl Pts',(-33.3118709730831,33.1695326803716,49.5918516942842));
#23837=CARTESIAN_POINT('Ctrl Pts',(-33.6392700281113,32.6337238479109,49.6288949573574));
#23838=CARTESIAN_POINT('Ctrl Pts',(-33.6666900469311,32.0829798887342,49.6659382204307));
#23839=CARTESIAN_POINT('Ctrl Pts',(-33.6941100657508,31.5322359295575,49.7029814835039));
#23840=CARTESIAN_POINT('Ctrl Pts',(-33.421551048362,30.9665568436648,49.7400247465772));
#23841=CARTESIAN_POINT('Ctrl Pts',(-32.9737345232321,30.6447943134935,49.7770680096504));
#23842=CARTESIAN_POINT('Ctrl Pts',(-32.5259179981021,30.3230317833222,49.8141112727237));
#23843=CARTESIAN_POINT('Ctrl Pts',(-31.9028439652309,30.2451858088723,49.8511545357969));
#23844=CARTESIAN_POINT('Ctrl Pts',(-31.3896277235822,30.4468782859499,49.8881977988701));
#23845=CARTESIAN_POINT('Ctrl Pts',(-30.8764114819335,30.6485707630274,49.9252410619434));
#23846=CARTESIAN_POINT('Ctrl Pts',(-30.4730530315072,31.1298016916325,49.9622843250166));
#23847=CARTESIAN_POINT('Ctrl Pts',(-30.3641270120983,31.6703624082013,49.9993275880899));
#23848=CARTESIAN_POINT('Ctrl Pts',(-30.3424135395067,31.778118574882,50.0067118465233));
#23849=CARTESIAN_POINT('Ctrl Pts',(-30.3323999345472,31.8882323305804,50.0140961049568));
#23850=CARTESIAN_POINT('Ctrl Pts',(-30.3334137894091,31.9985292433869,50.0214803633902));
#23851=CARTESIAN_POINT('Ctrl Pts',(-30.3365646132776,31.9994923926615,49.8285196366098));
#23852=CARTESIAN_POINT('Ctrl Pts',(-30.3358913027366,31.7530210124703,49.812097540526));
#23853=CARTESIAN_POINT('Ctrl Pts',(-30.3871544065278,31.5068159746518,49.7956754444422));
#23854=CARTESIAN_POINT('Ctrl Pts',(-30.4917685351372,31.2858719553962,49.7792533483584));
#23855=CARTESIAN_POINT('Ctrl Pts',(-30.7277462487909,30.7874893257988,49.7422100852852));
#23856=CARTESIAN_POINT('Ctrl Pts',(-31.2351828471017,30.4176389586602,49.7051668222119));
#23857=CARTESIAN_POINT('Ctrl Pts',(-31.7818780941429,30.345562376553,49.6681235591387));
#23858=CARTESIAN_POINT('Ctrl Pts',(-32.3285733411841,30.2734857944457,49.6310802960654));
#23859=CARTESIAN_POINT('Ctrl Pts',(-32.9145272369558,30.4991829973699,49.5940370329922));
#23860=CARTESIAN_POINT('Ctrl Pts',(-33.2716104559555,30.9193761690595,49.556993769919));
#23861=CARTESIAN_POINT('Ctrl Pts',(-33.6286936749552,31.3395693407491,49.5199505068457));
#23862=CARTESIAN_POINT('Ctrl Pts',(-33.7569062171829,31.954258481204,49.4829072437725));
#23863=CARTESIAN_POINT('Ctrl Pts',(-33.5975787185188,32.4821651727653,49.4458639806992));
#23864=CARTESIAN_POINT('Ctrl Pts',(-33.4382512198546,33.0100718643266,49.408820717626));
#23865=CARTESIAN_POINT('Ctrl Pts',(-32.9913836802987,33.4511961069941,49.3717774545528));
#23866=CARTESIAN_POINT('Ctrl Pts',(-32.4614602629135,33.6036818392199,49.3347341914795));
#23867=CARTESIAN_POINT('Ctrl Pts',(-31.9315368455282,33.7561675714457,49.2976909284063));
#23868=CARTESIAN_POINT('Ctrl Pts',(-31.3185575503135,33.6200147932296,49.260647665333));
#23869=CARTESIAN_POINT('Ctrl Pts',(-30.9030183790179,33.2575262776258,49.2236044022598));
#23870=CARTESIAN_POINT('Ctrl Pts',(-30.547475144405,32.9473741951013,49.1919094803764));
#23871=CARTESIAN_POINT('Ctrl Pts',(-30.3364746602739,32.471525346565,49.1602145584931));
#23872=CARTESIAN_POINT('Ctrl Pts',(-30.3325307394052,31.9987546512789,49.1285196366098));
#23873=CARTESIAN_POINT('Origin',(-32.,32.,48.));
#23874=CARTESIAN_POINT('',(-30.3326865661716,32.0013000733437,48.4285196366098));
#23875=CARTESIAN_POINT('',(-30.3362532366002,32.0008713514045,48.6214803633902));
#23876=CARTESIAN_POINT('',(-30.334,32.,48.));
#23877=CARTESIAN_POINT('Ctrl Pts',(-30.3362532366002,32.0008713514045,48.6214803633902));
#23878=CARTESIAN_POINT('Ctrl Pts',(-30.3352028368295,32.2223423058557,48.6362436147445));
#23879=CARTESIAN_POINT('Ctrl Pts',(-30.3763005180544,32.4434392568329,48.6510068660988));
#23880=CARTESIAN_POINT('Ctrl Pts',(-30.46138393715,32.6460665489047,48.6657701174531));
#23881=CARTESIAN_POINT('Ctrl Pts',(-30.6748712917368,33.1544895179307,48.7028133805264));
#23882=CARTESIAN_POINT('Ctrl Pts',(-31.1652862997157,33.546630265782,48.7398566435996));
#23883=CARTESIAN_POINT('Ctrl Pts',(-31.7082177126003,33.6430473125364,48.7768999066728));
#23884=CARTESIAN_POINT('Ctrl Pts',(-32.2511491254849,33.7394643592909,48.8139431697461));
#23885=CARTESIAN_POINT('Ctrl Pts',(-32.8465969432752,33.5401577049485,48.8509864328194));
#23886=CARTESIAN_POINT('Ctrl Pts',(-33.2220874732316,33.1363289938411,48.8880296958926));
#23887=CARTESIAN_POINT('Ctrl Pts',(-33.5975780031881,32.7325002827336,48.9250729589659));
#23888=CARTESIAN_POINT('Ctrl Pts',(-33.7531112453107,32.1241495148609,48.9621162220391));
#23889=CARTESIAN_POINT('Ctrl Pts',(-33.6175160313481,31.589654702957,48.9991594851123));
#23890=CARTESIAN_POINT('Ctrl Pts',(-33.4819208173855,31.0551598910532,49.0362027481855));
#23891=CARTESIAN_POINT('Ctrl Pts',(-33.0551971473377,30.5945210351181,49.0732460112588));
#23892=CARTESIAN_POINT('Ctrl Pts',(-32.5326114588057,30.4185239779174,49.110289274332));
#23893=CARTESIAN_POINT('Ctrl Pts',(-32.0100257702738,30.2425269207167,49.1473325374053));
#23894=CARTESIAN_POINT('Ctrl Pts',(-31.3915780632577,30.3511716622505,49.1843758004785));
#23895=CARTESIAN_POINT('Ctrl Pts',(-30.9602666550951,30.6947429578944,49.2214190635518));
#23896=CARTESIAN_POINT('Ctrl Pts',(-30.5719137171571,31.0040946688145,49.2547728301646));
#23897=CARTESIAN_POINT('Ctrl Pts',(-30.3352760634632,31.5039062165043,49.2881265967774));
#23898=CARTESIAN_POINT('Ctrl Pts',(-30.3319159461724,32.0009409208263,49.3214803633902));
#23899=CARTESIAN_POINT('Ctrl Pts',(-30.3325307394052,31.9987546512789,49.1285196366098));
#23900=CARTESIAN_POINT('Ctrl Pts',(-30.3318652247682,31.9189772348117,49.1231712954199));
#23901=CARTESIAN_POINT('Ctrl Pts',(-30.3370955793185,31.8392874677704,49.11782295423));
#23902=CARTESIAN_POINT('Ctrl Pts',(-30.3485221783749,31.7604963040532,49.1124746130401));
#23903=CARTESIAN_POINT('Ctrl Pts',(-30.427664196404,31.2147790990761,49.0754313499668));
#23904=CARTESIAN_POINT('Ctrl Pts',(-30.8040472798389,30.7121689421136,49.0383880868936));
#23905=CARTESIAN_POINT('Ctrl Pts',(-31.305440570552,30.4826575157017,49.0013448238203));
#23906=CARTESIAN_POINT('Ctrl Pts',(-31.806833861265,30.2531460892897,48.9643015607471));
#23907=CARTESIAN_POINT('Ctrl Pts',(-32.4332373592563,30.2967333934283,48.9272582976738));
#23908=CARTESIAN_POINT('Ctrl Pts',(-32.8980122203765,30.593474114086,48.8902150346006));
#23909=CARTESIAN_POINT('Ctrl Pts',(-33.3627870814967,30.8902148347436,48.8531717715274));
#23910=CARTESIAN_POINT('Ctrl Pts',(-33.6659333057459,31.4401089719203,48.8161285084541));
#23911=CARTESIAN_POINT('Ctrl Pts',(-33.6687328246495,31.9915279501207,48.7790852453809));
#23912=CARTESIAN_POINT('Ctrl Pts',(-33.6715323435531,32.5429469283212,48.7420419823076));
#23913=CARTESIAN_POINT('Ctrl Pts',(-33.3739851571112,33.0958907475454,48.7049987192344));
#23914=CARTESIAN_POINT('Ctrl Pts',(-32.9122472444572,33.3973353143294,48.6679554561611));
#23915=CARTESIAN_POINT('Ctrl Pts',(-32.4505093318031,33.6987798811135,48.6309121930879));
#23916=CARTESIAN_POINT('Ctrl Pts',(-31.824580692937,33.7487251954573,48.5938689300146));
#23917=CARTESIAN_POINT('Ctrl Pts',(-31.3208828790471,33.5243165523343,48.5568256669414));
#23918=CARTESIAN_POINT('Ctrl Pts',(-30.8171850651572,33.2999079092114,48.5197824038682));
#23919=CARTESIAN_POINT('Ctrl Pts',(-30.4357180762436,32.8011453086217,48.4827391407949));
#23920=CARTESIAN_POINT('Ctrl Pts',(-30.3510391380146,32.2562598121675,48.4456958777217));
#23921=CARTESIAN_POINT('Ctrl Pts',(-30.337951145404,32.1720422074084,48.4399704640177));
#23922=CARTESIAN_POINT('Ctrl Pts',(-30.331953078525,32.0867227796296,48.4342450503138));
#23923=CARTESIAN_POINT('Ctrl Pts',(-30.3326865661716,32.0013000733437,48.4285196366098));
#23924=CARTESIAN_POINT('Origin',(-32.,32.,48.));
#23925=CARTESIAN_POINT('',(-30.3366116302933,32.0004190051012,47.7285196366098));
#23926=CARTESIAN_POINT('',(-30.3350931202687,31.9985848581543,47.9214803633902));
#23927=CARTESIAN_POINT('',(-30.334,32.,48.));
#23928=CARTESIAN_POINT('Ctrl Pts',(-30.3350931202687,31.9985848581543,47.9214803633902));
#23929=CARTESIAN_POINT('Ctrl Pts',(-30.3382178428148,32.3854996272437,47.9473173696384));
#23930=CARTESIAN_POINT('Ctrl Pts',(-30.4725790046439,32.7743714460338,47.9731543758866));
#23931=CARTESIAN_POINT('Ctrl Pts',(-30.719095213247,33.0695907169318,47.9989913821348));
#23932=CARTESIAN_POINT('Ctrl Pts',(-31.0725326308559,33.4928551234624,48.036034645208));
#23933=CARTESIAN_POINT('Ctrl Pts',(-31.6565135644067,33.7236093551146,48.0730779082813));
#23934=CARTESIAN_POINT('Ctrl Pts',(-32.2038115052115,33.6562615266971,48.1101211713545));
#23935=CARTESIAN_POINT('Ctrl Pts',(-32.7511094460163,33.5889136982795,48.1471644344277));
#23936=CARTESIAN_POINT('Ctrl Pts',(-33.2617243940749,33.2234638097922,48.1842076975009));
#23937=CARTESIAN_POINT('Ctrl Pts',(-33.5020017178502,32.7271397486375,48.2212509605742));
#23938=CARTESIAN_POINT('Ctrl Pts',(-33.7422790416254,32.2308156874827,48.2582942236474));
#23939=CARTESIAN_POINT('Ctrl Pts',(-33.7122187411171,31.6036174536605,48.2953374867207));
#23940=CARTESIAN_POINT('Ctrl Pts',(-33.4255762468427,31.1325475581271,48.332380749794));
#23941=CARTESIAN_POINT('Ctrl Pts',(-33.1389337525684,30.6614776625936,48.3694240128672));
#23942=CARTESIAN_POINT('Ctrl Pts',(-32.5957090645279,30.346536105349,48.4064672759404));
#23943=CARTESIAN_POINT('Ctrl Pts',(-32.0444788544554,30.3318384352888,48.4435105390137));
#23944=CARTESIAN_POINT('Ctrl Pts',(-31.493248644383,30.3171407652286,48.4805538020869));
#23945=CARTESIAN_POINT('Ctrl Pts',(-30.9340129122786,30.6026869823528,48.5175970651601));
#23946=CARTESIAN_POINT('Ctrl Pts',(-30.6226748968236,31.0578126860153,48.5546403282334));
#23947=CARTESIAN_POINT('Ctrl Pts',(-30.4354177802146,31.3315522318847,48.5769203399523));
#23948=CARTESIAN_POINT('Ctrl Pts',(-30.3378384510384,31.6666376963542,48.5992003516713));
#23949=CARTESIAN_POINT('Ctrl Pts',(-30.3362532366002,32.0008713514045,48.6214803633902));
#23950=CARTESIAN_POINT('Ctrl Pts',(-30.3326865661716,32.0013000733437,48.4285196366098));
#23951=CARTESIAN_POINT('Ctrl Pts',(-30.3366987226406,31.5340403107302,48.3972017872405));
#23952=CARTESIAN_POINT('Ctrl Pts',(-30.5421229447233,31.0636903945153,48.3658839378712));
#23953=CARTESIAN_POINT('Ctrl Pts',(-30.8903064956353,30.753676870927,48.334566088502));
#23954=CARTESIAN_POINT('Ctrl Pts',(-31.3021436790294,30.3869878184592,48.2975228254287));
#23955=CARTESIAN_POINT('Ctrl Pts',(-31.9137089333623,30.2446181058425,48.2604795623555));
#23956=CARTESIAN_POINT('Ctrl Pts',(-32.4451533143256,30.3917153416025,48.2234362992823));
#23957=CARTESIAN_POINT('Ctrl Pts',(-32.9765976952889,30.5388125773625,48.186393036209));
#23958=CARTESIAN_POINT('Ctrl Pts',(-33.4279212028827,30.9753767614993,48.1493497731358));
#23959=CARTESIAN_POINT('Ctrl Pts',(-33.5926006472318,31.5016384905226,48.1123065100625));
#23960=CARTESIAN_POINT('Ctrl Pts',(-33.757280091581,32.0279002195459,48.0752632469893));
#23961=CARTESIAN_POINT('Ctrl Pts',(-33.6353154726855,32.6438594934557,48.0382199839161));
#23962=CARTESIAN_POINT('Ctrl Pts',(-33.2825171388263,33.0676566884109,48.0011767208428));
#23963=CARTESIAN_POINT('Ctrl Pts',(-32.9297188049672,33.4914538833661,47.9641334577696));
#23964=CARTESIAN_POINT('Ctrl Pts',(-32.3460867561444,33.7230889993668,47.9270901946963));
#23965=CARTESIAN_POINT('Ctrl Pts',(-31.7986878532862,33.6565670633202,47.890046931623));
#23966=CARTESIAN_POINT('Ctrl Pts',(-31.2512889504281,33.5900451272736,47.8530036685498));
#23967=CARTESIAN_POINT('Ctrl Pts',(-30.7401231935345,33.2253661391796,47.8159604054766));
#23968=CARTESIAN_POINT('Ctrl Pts',(-30.4990972612792,32.7294052266006,47.7789171424033));
#23969=CARTESIAN_POINT('Ctrl Pts',(-30.3897916835172,32.5044862994563,47.7621179738055));
#23970=CARTESIAN_POINT('Ctrl Pts',(-30.3360439926465,32.252567479493,47.7453188052076));
#23971=CARTESIAN_POINT('Ctrl Pts',(-30.3366116302933,32.0004190051012,47.7285196366098));
#23972=CARTESIAN_POINT('Origin',(-32.,32.,48.));
#23973=CARTESIAN_POINT('',(-30.3342224488932,31.998478175086,47.0285196366098));
#23974=CARTESIAN_POINT('',(-30.3312462010541,31.9999631497184,47.2214803633902));
#23975=CARTESIAN_POINT('',(-30.334,32.,48.));
#23976=CARTESIAN_POINT('Ctrl Pts',(-30.3312465935645,31.9999631549708,47.2214803633902));
#23977=CARTESIAN_POINT('Ctrl Pts',(-30.3314253835204,32.5494177694831,47.2583911245323));
#23978=CARTESIAN_POINT('Ctrl Pts',(-30.6293231342425,33.0990385199082,47.2953018856743));
#23979=CARTESIAN_POINT('Ctrl Pts',(-31.0898621581925,33.3987102928711,47.3322126468164));
#23980=CARTESIAN_POINT('Ctrl Pts',(-31.5520544211483,33.6994578249731,47.3692559098896));
#23981=CARTESIAN_POINT('Ctrl Pts',(-32.1780577496979,33.748458629264,47.4062991729629));
#23982=CARTESIAN_POINT('Ctrl Pts',(-32.6814164150587,33.5232902033959,47.4433424360361));
#23983=CARTESIAN_POINT('Ctrl Pts',(-33.1847750804195,33.2981217775279,47.4803856991094));
#23984=CARTESIAN_POINT('Ctrl Pts',(-33.5654890825915,32.7987841215009,47.5174289621826));
#23985=CARTESIAN_POINT('Ctrl Pts',(-33.6493457585165,32.2537714391672,47.5544722252558));
#23986=CARTESIAN_POINT('Ctrl Pts',(-33.7332024344415,31.7087587568336,47.5915154883291));
#23987=CARTESIAN_POINT('Ctrl Pts',(-33.5202017841195,31.1180710481933,47.6285587514023));
#23988=CARTESIAN_POINT('Ctrl Pts',(-33.10781175019,30.7520038058494,47.6656020144756));
#23989=CARTESIAN_POINT('Ctrl Pts',(-32.6954217162604,30.3859365635055,47.7026452775488));
#23990=CARTESIAN_POINT('Ctrl Pts',(-32.0836422987232,30.2444897874579,47.7396885406221));
#23991=CARTESIAN_POINT('Ctrl Pts',(-31.5524204418077,30.392388755463,47.7767318036953));
#23992=CARTESIAN_POINT('Ctrl Pts',(-31.0211985848922,30.540287723468,47.8137750667685));
#23993=CARTESIAN_POINT('Ctrl Pts',(-30.5705342885984,30.9775324355256,47.8508183298418));
#23994=CARTESIAN_POINT('Ctrl Pts',(-30.4066490912849,31.5040420822589,47.887861592915));
#23995=CARTESIAN_POINT('Ctrl Pts',(-30.357070856039,31.6633207697356,47.8990678497401));
#23996=CARTESIAN_POINT('Ctrl Pts',(-30.3337378377324,31.8307687330905,47.9102741065651));
#23997=CARTESIAN_POINT('Ctrl Pts',(-30.3350931202687,31.9985848581543,47.9214803633902));
#23998=CARTESIAN_POINT('Ctrl Pts',(-30.3366116302933,32.0004190051012,47.7285196366098));
#23999=CARTESIAN_POINT('Ctrl Pts',(-30.3372956707017,31.6965636382308,47.7082755421344));
#24000=CARTESIAN_POINT('Ctrl Pts',(-30.416855468772,31.3923747712685,47.688031447659));
#24001=CARTESIAN_POINT('Ctrl Pts',(-30.573116579137,31.1346996365665,47.6677873531836));
#24002=CARTESIAN_POINT('Ctrl Pts',(-30.8590479368673,30.6631977961753,47.6307440901104));
#24003=CARTESIAN_POINT('Ctrl Pts',(-31.4017967599448,30.3474369524569,47.5937008270371));
#24004=CARTESIAN_POINT('Ctrl Pts',(-31.9530041298623,30.331907555355,47.5566575639639));
#24005=CARTESIAN_POINT('Ctrl Pts',(-32.5042114997798,30.3163781582531,47.5196143008906));
#24006=CARTESIAN_POINT('Ctrl Pts',(-33.0638774165373,30.6010802077676,47.4825710378174));
#24007=CARTESIAN_POINT('Ctrl Pts',(-33.3759017912886,31.0557355897734,47.4455277747441));
#24008=CARTESIAN_POINT('Ctrl Pts',(-33.6879261660399,31.5103909717791,47.4084845116709));
#24009=CARTESIAN_POINT('Ctrl Pts',(-33.752308998785,32.134999686276,47.3714412485977));
#24010=CARTESIAN_POINT('Ctrl Pts',(-33.5395890543612,32.6437441723101,47.3343979855244));
#24011=CARTESIAN_POINT('Ctrl Pts',(-33.3268691099373,33.1524886583441,47.2973547224512));
#24012=CARTESIAN_POINT('Ctrl Pts',(-32.8370463883445,33.5453689159152,47.260311459378));
#24013=CARTESIAN_POINT('Ctrl Pts',(-32.2942611110305,33.6426050694634,47.2232681963047));
#24014=CARTESIAN_POINT('Ctrl Pts',(-31.7514758337164,33.7398412230116,47.1862249332315));
#24015=CARTESIAN_POINT('Ctrl Pts',(-31.1557280006812,33.5414332725369,47.1491816701582));
#24016=CARTESIAN_POINT('Ctrl Pts',(-30.7796285900135,33.1381716203541,47.112138407085));
#24017=CARTESIAN_POINT('Ctrl Pts',(-30.4966354293383,32.8347404362218,47.0842654835932));
#24018=CARTESIAN_POINT('Ctrl Pts',(-30.3380005358351,32.4153273065168,47.0563925601015));
#24019=CARTESIAN_POINT('Ctrl Pts',(-30.3342224488932,31.998478175086,47.0285196366098));
#24020=CARTESIAN_POINT('Origin',(-32.,32.,48.));
#24021=CARTESIAN_POINT('',(-30.3314412831326,32.0005167954427,46.3285196366098));
#24022=CARTESIAN_POINT('',(-30.334985752807,32.0014384754872,46.5214803633902));
#24023=CARTESIAN_POINT('',(-30.334,32.,48.));
#24024=CARTESIAN_POINT('Ctrl Pts',(-30.334985752807,32.0014384754872,46.5214803633902));
#24025=CARTESIAN_POINT('Ctrl Pts',(-30.333634356184,32.1652593777732,46.5324216163529));
#24026=CARTESIAN_POINT('Ctrl Pts',(-30.3558556724076,32.3287216717838,46.5433628693156));
#24027=CARTESIAN_POINT('Ctrl Pts',(-30.403150530605,32.4845752228154,46.5543041222783));
#24028=CARTESIAN_POINT('Ctrl Pts',(-30.5632744104012,33.0122409400272,46.5913473853516));
#24029=CARTESIAN_POINT('Ctrl Pts',(-31.0108070772609,33.4526904357357,46.6283906484248));
#24030=CARTESIAN_POINT('Ctrl Pts',(-31.5409600094739,33.6043764089425,46.665433911498));
#24031=CARTESIAN_POINT('Ctrl Pts',(-32.0711129416868,33.7560623821493,46.7024771745713));
#24032=CARTESIAN_POINT('Ctrl Pts',(-32.6838861392531,33.6189848328544,46.7395204376445));
#24033=CARTESIAN_POINT('Ctrl Pts',(-33.0988779095908,33.2558697043431,46.7765637007178));
#24034=CARTESIAN_POINT('Ctrl Pts',(-33.5138696799284,32.8927545758318,46.813606963791));
#24035=CARTESIAN_POINT('Ctrl Pts',(-33.7310800230373,32.3036018681042,46.8506502268642));
#24036=CARTESIAN_POINT('Ctrl Pts',(-33.6511146636849,31.7580046656688,46.8876934899375));
#24037=CARTESIAN_POINT('Ctrl Pts',(-33.5711493043325,31.2124074632333,46.9247367530107));
#24038=CARTESIAN_POINT('Ctrl Pts',(-33.1940082425188,30.7103657660902,46.961780016084));
#24039=CARTESIAN_POINT('Ctrl Pts',(-32.6922691831675,30.4816111326442,46.9988232791572));
#24040=CARTESIAN_POINT('Ctrl Pts',(-32.1905301238162,30.2528564991983,47.0358665422305));
#24041=CARTESIAN_POINT('Ctrl Pts',(-31.5641930669273,30.2973889294496,47.0729098053037));
#24042=CARTESIAN_POINT('Ctrl Pts',(-31.0998664535619,30.5948306247821,47.109953068377));
#24043=CARTESIAN_POINT('Ctrl Pts',(-30.6355398401965,30.8922723201147,47.1469963314502));
#24044=CARTESIAN_POINT('Ctrl Pts',(-30.3332236703546,31.4426232805285,47.1840395945234));
#24045=CARTESIAN_POINT('Ctrl Pts',(-30.3312561841146,31.9940458906921,47.2210828575967));
#24046=CARTESIAN_POINT('Ctrl Pts',(-30.331249146513,31.9960183022638,47.2212153595278));
#24047=CARTESIAN_POINT('Ctrl Pts',(-30.3312459517459,31.9979907275468,47.221347861459));
#24048=CARTESIAN_POINT('Ctrl Pts',(-30.3312465935646,31.9999631549708,47.2214803633902));
#24049=CARTESIAN_POINT('Ctrl Pts',(-30.3342224488932,31.998478175086,47.0285196366098));
#24050=CARTESIAN_POINT('Ctrl Pts',(-30.3329794382619,31.8613326011525,47.0193492970283));
#24051=CARTESIAN_POINT('Ctrl Pts',(-30.3484988233775,31.7244645658994,47.0101789574468));
#24052=CARTESIAN_POINT('Ctrl Pts',(-30.3818667490394,31.592095847254,47.0010086178652));
#24053=CARTESIAN_POINT('Ctrl Pts',(-30.5166553070329,31.0573970802274,46.963965354792));
#24054=CARTESIAN_POINT('Ctrl Pts',(-30.9426834113199,30.596114900065,46.9269220917188));
#24055=CARTESIAN_POINT('Ctrl Pts',(-31.46500291142,30.4193295312107,46.8898788286455));
#24056=CARTESIAN_POINT('Ctrl Pts',(-31.98732241152,30.2425441623563,46.8528355655723));
#24057=CARTESIAN_POINT('Ctrl Pts',(-32.605933307433,30.35025560481,46.815792302499));
#24058=CARTESIAN_POINT('Ctrl Pts',(-33.0377626074672,30.6931756865459,46.7787490394258));
#24059=CARTESIAN_POINT('Ctrl Pts',(-33.4695919075013,31.0360957682818,46.7417057763525));
#24060=CARTESIAN_POINT('Ctrl Pts',(-33.7146396116566,31.6142244892999,46.7046625132793));
#24061=CARTESIAN_POINT('Ctrl Pts',(-33.6607732192273,32.1630132816348,46.6676192502061));
#24062=CARTESIAN_POINT('Ctrl Pts',(-33.606906826798,32.7118020739697,46.6305759871328));
#24063=CARTESIAN_POINT('Ctrl Pts',(-33.2541263377842,33.2312509376214,46.5935327240596));
#24064=CARTESIAN_POINT('Ctrl Pts',(-32.7638621910861,33.483662889177,46.5564894609863));
#24065=CARTESIAN_POINT('Ctrl Pts',(-32.273598044388,33.7360748407326,46.5194461979131));
#24066=CARTESIAN_POINT('Ctrl Pts',(-31.6458502400056,33.7214498801921,46.4824029348399));
#24067=CARTESIAN_POINT('Ctrl Pts',(-31.1678727694035,33.4464803101984,46.4453596717666));
#24068=CARTESIAN_POINT('Ctrl Pts',(-30.6898952988014,33.1715107402047,46.4083164086934));
#24069=CARTESIAN_POINT('Ctrl Pts',(-30.3616881619796,32.6361965607576,46.3712731456201));
#24070=CARTESIAN_POINT('Ctrl Pts',(-30.3334371651187,32.085494637752,46.3342298825469));
#24071=CARTESIAN_POINT('Ctrl Pts',(-30.3319855278829,32.0571976038022,46.3323264672345));
#24072=CARTESIAN_POINT('Ctrl Pts',(-30.3313258564002,32.0288599420261,46.3304230519221));
#24073=CARTESIAN_POINT('Ctrl Pts',(-30.3314412831326,32.0005167954427,46.3285196366098));
#24074=CARTESIAN_POINT('Origin',(-32.,32.,48.));
#24075=CARTESIAN_POINT('',(-30.3357441935225,32.0011936368988,45.6285196366098));
#24076=CARTESIAN_POINT('',(-30.336314001127,31.9991832783969,45.8214803633902));
#24077=CARTESIAN_POINT('',(-30.334,32.,48.));
#24078=CARTESIAN_POINT('Ctrl Pts',(-30.336314001127,31.9991832783969,45.8214803633902));
#24079=CARTESIAN_POINT('Ctrl Pts',(-30.3377789880212,32.3294716685071,45.8434953712468));
#24080=CARTESIAN_POINT('Ctrl Pts',(-30.4328915994036,32.6605377086288,45.8655103791034));
#24081=CARTESIAN_POINT('Ctrl Pts',(-30.6159865666574,32.9323348061725,45.88752538696));
#24082=CARTESIAN_POINT('Ctrl Pts',(-30.9240689022873,33.3896706132929,45.9245686500332));
#24083=CARTESIAN_POINT('Ctrl Pts',(-31.4812527529819,33.6792002364776,45.9616119131064));
#24084=CARTESIAN_POINT('Ctrl Pts',(-32.032573809867,33.6684364900661,45.9986551761797));
#24085=CARTESIAN_POINT('Ctrl Pts',(-32.5838948667521,33.6576727436547,46.0356984392529));
#24086=CARTESIAN_POINT('Ctrl Pts',(-33.1293531298277,33.3466156276472,46.0727417023262));
#24087=CARTESIAN_POINT('Ctrl Pts',(-33.4193498555347,32.8776031916916,46.1097849653994));
#24088=CARTESIAN_POINT('Ctrl Pts',(-33.7093465812416,32.408590755736,46.1468282284727));
#24089=CARTESIAN_POINT('Ctrl Pts',(-33.7438817695798,31.7816229998324,46.1838714915459));
#24090=CARTESIAN_POINT('Ctrl Pts',(-33.5071523056252,31.2835969694912,46.2209147546192));
#24091=CARTESIAN_POINT('Ctrl Pts',(-33.2704228416705,30.78557093915,46.2579580176924));
#24092=CARTESIAN_POINT('Ctrl Pts',(-32.7624287254228,30.4164866343711,46.2950012807656));
#24093=CARTESIAN_POINT('Ctrl Pts',(-32.2156253099937,30.3452350317451,46.3320445438389));
#24094=CARTESIAN_POINT('Ctrl Pts',(-31.6688218945646,30.2739834291191,46.3690878069121));
#24095=CARTESIAN_POINT('Ctrl Pts',(-31.0832091799541,30.500564528646,46.4061310699853));
#24096=CARTESIAN_POINT('Ctrl Pts',(-30.7267603690151,30.9212960477671,46.4431743330586));
#24097=CARTESIAN_POINT('Ctrl Pts',(-30.4755937682591,31.217758547418,46.4692763431691));
#24098=CARTESIAN_POINT('Ctrl Pts',(-30.3382097133934,31.6106189905197,46.4953783532797));
#24099=CARTESIAN_POINT('Ctrl Pts',(-30.334985752807,32.0014384754872,46.5214803633902));
#24100=CARTESIAN_POINT('Ctrl Pts',(-30.3314412831326,32.0005167954427,46.3285196366098));
#24101=CARTESIAN_POINT('Ctrl Pts',(-30.3335722304769,31.4772605993123,46.2933797888489));
#24102=CARTESIAN_POINT('Ctrl Pts',(-30.5998767510865,30.9521350386003,46.258239941088));
#24103=CARTESIAN_POINT('Ctrl Pts',(-31.0242217941959,30.6462651999857,46.2231000933271));
#24104=CARTESIAN_POINT('Ctrl Pts',(-31.471552277034,30.3238273517893,46.1860568302539));
#24105=CARTESIAN_POINT('Ctrl Pts',(-32.0945080996103,30.2450413219607,46.1490135671807));
#24106=CARTESIAN_POINT('Ctrl Pts',(-32.608028055351,30.4459591705499,46.1119703041074));
#24107=CARTESIAN_POINT('Ctrl Pts',(-33.1215480110917,30.6468770191392,46.0749270410342));
#24108=CARTESIAN_POINT('Ctrl Pts',(-33.525632099997,31.1274987461464,46.0378837779609));
#24109=CARTESIAN_POINT('Ctrl Pts',(-33.6353736340385,31.6678944553558,46.0008405148877));
#24110=CARTESIAN_POINT('Ctrl Pts',(-33.74511516808,32.2082901645652,45.9637972518145));
#24111=CARTESIAN_POINT('Ctrl Pts',(-33.5605141472577,32.8084598559768,45.9267539887412));
#24112=CARTESIAN_POINT('Ctrl Pts',(-33.1660429977425,33.1937691330854,45.889710725668));
#24113=CARTESIAN_POINT('Ctrl Pts',(-32.7715718482274,33.5790784101939,45.8526674625947));
#24114=CARTESIAN_POINT('Ctrl Pts',(-32.1672305700194,33.7495272729993,45.8156241995215));
#24115=CARTESIAN_POINT('Ctrl Pts',(-31.6295624551223,33.6271192461024,45.7785809364482));
#24116=CARTESIAN_POINT('Ctrl Pts',(-31.0918943402253,33.5047112192054,45.741537673375));
#24117=CARTESIAN_POINT('Ctrl Pts',(-30.6208993886393,33.0894463026061,45.7044944103018));
#24118=CARTESIAN_POINT('Ctrl Pts',(-30.4321023363463,32.57134747046,45.6674511472285));
#24119=CARTESIAN_POINT('Ctrl Pts',(-30.3659620647077,32.3898446499573,45.6544739770223));
#24120=CARTESIAN_POINT('Ctrl Pts',(-30.3344552072224,32.1957212904815,45.641496806816));
#24121=CARTESIAN_POINT('Ctrl Pts',(-30.3357441935225,32.0011936368988,45.6285196366098));
#24122=CARTESIAN_POINT('Origin',(-32.,32.,48.));
#24123=CARTESIAN_POINT('',(-30.3357491953914,31.9988087176276,44.9285196366098));
#24124=CARTESIAN_POINT('',(-30.3320048130563,31.999003946099,45.1214803633902));
#24125=CARTESIAN_POINT('',(-30.334,32.,48.));
#24126=CARTESIAN_POINT('Ctrl Pts',(-30.3320048130563,31.999003946099,45.1214803633902));
#24127=CARTESIAN_POINT('Ctrl Pts',(-30.3354915306281,32.4921586983372,45.1545691261407));
#24128=CARTESIAN_POINT('Ctrl Pts',(-30.5679112921037,32.9881690576534,45.1876578888911));
#24129=CARTESIAN_POINT('Ctrl Pts',(-30.9509788831921,33.297804326917,45.2207466516416));
#24130=CARTESIAN_POINT('Ctrl Pts',(-31.3798276031801,33.6444446900695,45.2577899147148));
#24131=CARTESIAN_POINT('Ctrl Pts',(-31.9974842806894,33.7574998752863,45.2948331777881));
#24132=CARTESIAN_POINT('Ctrl Pts',(-32.5213125691959,33.5852364428286,45.3318764408614));
#24133=CARTESIAN_POINT('Ctrl Pts',(-33.0451408577023,33.4129730103709,45.3689197039346));
#24134=CARTESIAN_POINT('Ctrl Pts',(-33.4751407572058,32.9553909602385,45.4059629670078));
#24135=CARTESIAN_POINT('Ctrl Pts',(-33.6145466452709,32.4218773574368,45.443006230081));
#24136=CARTESIAN_POINT('Ctrl Pts',(-33.7539525333361,31.888363754635,45.4800494931543));
#24137=CARTESIAN_POINT('Ctrl Pts',(-33.6027644099628,31.2789185991639,45.5170927562275));
#24138=CARTESIAN_POINT('Ctrl Pts',(-33.2301651406233,30.8724206895882,45.5541360193008));
#24139=CARTESIAN_POINT('Ctrl Pts',(-32.8575658712839,30.4659227800126,45.591179282374));
#24140=CARTESIAN_POINT('Ctrl Pts',(-32.2635554559781,30.2623721163323,45.6282225454473));
#24141=CARTESIAN_POINT('Ctrl Pts',(-31.7199498398627,30.3549123785401,45.6652658085205));
#24142=CARTESIAN_POINT('Ctrl Pts',(-31.1763442237472,30.4474526407479,45.7023090715938));
#24143=CARTESIAN_POINT('Ctrl Pts',(-30.6831434068221,30.8360838288437,45.739352334667));
#24144=CARTESIAN_POINT('Ctrl Pts',(-30.4660334086422,31.3429704184197,45.7763955977402));
#24145=CARTESIAN_POINT('Ctrl Pts',(-30.3779530347214,31.5486116174412,45.7914238529569));
#24146=CARTESIAN_POINT('Ctrl Pts',(-30.3353139471148,31.7737162581709,45.8064521081735));
#24147=CARTESIAN_POINT('Ctrl Pts',(-30.336314001127,31.9991832783969,45.8214803633902));
#24148=CARTESIAN_POINT('Ctrl Pts',(-30.3357441935225,32.0011936368988,45.6285196366098));
#24149=CARTESIAN_POINT('Ctrl Pts',(-30.3381346117347,31.6404431418435,45.6044535437428));
#24150=CARTESIAN_POINT('Ctrl Pts',(-30.4533148708266,31.2783022185287,45.5803874508758));
#24151=CARTESIAN_POINT('Ctrl Pts',(-30.6695651562039,30.9926846858579,45.5563213580088));
#24152=CARTESIAN_POINT('Ctrl Pts',(-31.0024241813547,30.5530534810948,45.5192780949355));
#24153=CARTESIAN_POINT('Ctrl Pts',(-31.5747413846563,30.2947238192617,45.4822348318623));
#24154=CARTESIAN_POINT('Ctrl Pts',(-32.1246275171387,30.335905952879,45.4451915687891));
#24155=CARTESIAN_POINT('Ctrl Pts',(-32.6745136496211,30.3770880864963,45.4081483057158));
#24156=CARTESIAN_POINT('Ctrl Pts',(-33.2019687112843,30.717782015564,45.3711050426426));
#24157=CARTESIAN_POINT('Ctrl Pts',(-33.4656321259172,31.2020880454767,45.3340617795694));
#24158=CARTESIAN_POINT('Ctrl Pts',(-33.7292955405502,31.6863940753895,45.2970185164961));
#24159=CARTESIAN_POINT('Ctrl Pts',(-33.7291673081528,32.3143122061471,45.2599752534228));
#24160=CARTESIAN_POINT('Ctrl Pts',(-33.4653061071749,32.7985105058593,45.2229319903496));
#24161=CARTESIAN_POINT('Ctrl Pts',(-33.2014449061969,33.2827088055716,45.1858887272763));
#24162=CARTESIAN_POINT('Ctrl Pts',(-32.6738507366385,33.6231872742384,45.1488454642032));
#24163=CARTESIAN_POINT('Ctrl Pts',(-32.1239478297291,33.6641448107654,45.1118022011299));
#24164=CARTESIAN_POINT('Ctrl Pts',(-31.5740449228197,33.7051023472924,45.0747589380567));
#24165=CARTESIAN_POINT('Ctrl Pts',(-31.0018332785595,33.4465389516795,45.0377156749834));
#24166=CARTESIAN_POINT('Ctrl Pts',(-30.6691538426735,33.0067718317578,45.0006724119101));
#24167=CARTESIAN_POINT('Ctrl Pts',(-30.4531564512173,32.7212460657954,44.97662148681));
#24168=CARTESIAN_POINT('Ctrl Pts',(-30.3381329336397,32.3593345722981,44.9525705617099));
#24169=CARTESIAN_POINT('Ctrl Pts',(-30.3357491953914,31.9988087176276,44.9285196366098));
#24170=CARTESIAN_POINT('Origin',(-32.,32.,48.));
#24171=CARTESIAN_POINT('',(-30.3314442636938,31.9994792812594,44.2285196366098));
#24172=CARTESIAN_POINT('',(-30.333294480282,32.0014513626233,44.4214803633902));
#24173=CARTESIAN_POINT('',(-30.334,32.,48.));
#24174=CARTESIAN_POINT('Ctrl Pts',(-30.333294480282,32.0014513626233,44.4214803633902));
#24175=CARTESIAN_POINT('Ctrl Pts',(-30.3323222284007,32.1077703704247,44.4285996179613));
#24176=CARTESIAN_POINT('Ctrl Pts',(-30.3416240402429,32.2139199074504,44.4357188725324));
#24177=CARTESIAN_POINT('Ctrl Pts',(-30.3618163870715,32.3179556962936,44.4428381271035));
#24178=CARTESIAN_POINT('Ctrl Pts',(-30.4668822206032,32.8592799398168,44.4798813901767));
#24179=CARTESIAN_POINT('Ctrl Pts',(-30.8667963627591,33.3433769601342,44.51692465325));
#24180=CARTESIAN_POINT('Ctrl Pts',(-31.3785602705332,33.5487265856548,44.5539679163233));
#24181=CARTESIAN_POINT('Ctrl Pts',(-31.8903241783073,33.7540762111755,44.5910111793965));
#24182=CARTESIAN_POINT('Ctrl Pts',(-32.5139378516996,33.6806784418995,44.6280544424697));
#24183=CARTESIAN_POINT('Ctrl Pts',(-32.9640390551699,33.3621196990649,44.6650977055429));
#24184=CARTESIAN_POINT('Ctrl Pts',(-33.4141402586402,33.0435609562303,44.7021409686162));
#24185=CARTESIAN_POINT('Ctrl Pts',(-33.6907289921885,32.4798412398371,44.7391842316895));
#24186=CARTESIAN_POINT('Ctrl Pts',(-33.6672397510832,31.9289156354639,44.7762274947627));
#24187=CARTESIAN_POINT('Ctrl Pts',(-33.6437505099779,31.3779900310907,44.813270757836));
#24188=CARTESIAN_POINT('Ctrl Pts',(-33.3201832942189,30.8398585387374,44.8503140209091));
#24189=CARTESIAN_POINT('Ctrl Pts',(-32.8446007072674,30.5607672114085,44.8873572839824));
#24190=CARTESIAN_POINT('Ctrl Pts',(-32.3690181203159,30.2816758840796,44.9244005470556));
#24191=CARTESIAN_POINT('Ctrl Pts',(-31.7414201621719,30.261624721775,44.9614438101289));
#24192=CARTESIAN_POINT('Ctrl Pts',(-31.2489922554738,30.5097890276424,44.9984870732021));
#24193=CARTESIAN_POINT('Ctrl Pts',(-30.7565643487757,30.7579533335098,45.0355303362754));
#24194=CARTESIAN_POINT('Ctrl Pts',(-30.3993064935235,31.2743331075492,45.0725735993487));
#24195=CARTESIAN_POINT('Ctrl Pts',(-30.3406979471307,31.8226357651129,45.1096168624219));
#24196=CARTESIAN_POINT('Ctrl Pts',(-30.3344412759738,31.8811690274777,45.1135713627447));
#24197=CARTESIAN_POINT('Ctrl Pts',(-30.3315881088759,31.9400660933418,45.1175258630674));
#24198=CARTESIAN_POINT('Ctrl Pts',(-30.3320048130563,31.999003946099,45.1214803633902));
#24199=CARTESIAN_POINT('Ctrl Pts',(-30.3357491953914,31.9988087176276,44.9285196366098));
#24200=CARTESIAN_POINT('Ctrl Pts',(-30.3344614971914,31.8040522277035,44.9155272986367));
#24201=CARTESIAN_POINT('Ctrl Pts',(-30.3660440362041,31.6097000911722,44.9025349606636));
#24202=CARTESIAN_POINT('Ctrl Pts',(-30.4323358263775,31.4280121903116,44.8895426226905));
#24203=CARTESIAN_POINT('Ctrl Pts',(-30.6213444734794,30.9099905130176,44.8524993596172));
#24204=CARTESIAN_POINT('Ctrl Pts',(-31.0925089951951,30.4949180026602,44.815456096544));
#24205=CARTESIAN_POINT('Ctrl Pts',(-31.6302270611707,30.3727295893424,44.7784128334707));
#24206=CARTESIAN_POINT('Ctrl Pts',(-32.1679451271464,30.2505411760246,44.7413695703975));
#24207=CARTESIAN_POINT('Ctrl Pts',(-32.7722167373819,30.4212368597464,44.7043263073242));
#24208=CARTESIAN_POINT('Ctrl Pts',(-33.16653047956,30.8067072211947,44.667283044251));
#24209=CARTESIAN_POINT('Ctrl Pts',(-33.5608442217381,31.1921775826431,44.6302397811777));
#24210=CARTESIAN_POINT('Ctrl Pts',(-33.7452000958586,31.792422621818,44.5931965181045));
#24211=CARTESIAN_POINT('Ctrl Pts',(-33.6352378535522,32.3327734634876,44.5561532550313));
#24212=CARTESIAN_POINT('Ctrl Pts',(-33.5252756112458,32.8731243051572,44.519109991958));
#24213=CARTESIAN_POINT('Ctrl Pts',(-33.1209952525124,33.3535809493216,44.4820667288848));
#24214=CARTESIAN_POINT('Ctrl Pts',(-32.6073932773895,33.554289040776,44.4450234658115));
#24215=CARTESIAN_POINT('Ctrl Pts',(-32.0937913022666,33.7549971322304,44.4079802027383));
#24216=CARTESIAN_POINT('Ctrl Pts',(-31.4708677107543,33.6759566709748,44.370936939665));
#24217=CARTESIAN_POINT('Ctrl Pts',(-31.0236689606658,33.3533361435062,44.3338936765918));
#24218=CARTESIAN_POINT('Ctrl Pts',(-30.5996319917973,33.0474251128168,44.2987689965978));
#24219=CARTESIAN_POINT('Ctrl Pts',(-30.3335886032366,32.522512110404,44.2636443166038));
#24220=CARTESIAN_POINT('Ctrl Pts',(-30.3314442636938,31.9994792812594,44.2285196366098));
#24221=CARTESIAN_POINT('Origin',(-32.,32.,48.));
#24222=CARTESIAN_POINT('',(-30.3342156580691,32.0015219727962,43.5285196366098));
#24223=CARTESIAN_POINT('',(-30.3367054458351,32.0000809143127,43.7214803633902));
#24224=CARTESIAN_POINT('',(-30.334,32.,48.));
#24225=CARTESIAN_POINT('Ctrl Pts',(-30.3367054458351,32.0000809143127,43.7214803633902));
#24226=CARTESIAN_POINT('Ctrl Pts',(-30.3365871091324,32.2731888506978,43.7396733728552));
#24227=CARTESIAN_POINT('Ctrl Pts',(-30.4000931468668,32.5462449571753,43.7578663823202));
#24228=CARTESIAN_POINT('Ctrl Pts',(-30.5275247652971,32.7852121099577,43.7760593917851));
#24229=CARTESIAN_POINT('Ctrl Pts',(-30.7869916212039,33.2717793886379,43.8131026548584));
#24230=CARTESIAN_POINT('Ctrl Pts',(-31.3114817803501,33.6170203467136,43.8501459179317));
#24231=CARTESIAN_POINT('Ctrl Pts',(-31.8609913898654,33.6629545937273,43.8871891810049));
#24232=CARTESIAN_POINT('Ctrl Pts',(-32.4105009993806,33.7088888407409,43.9242324440781));
#24233=CARTESIAN_POINT('Ctrl Pts',(-32.9850300592647,33.4555163766925,43.9612757071513));
#24234=CARTESIAN_POINT('Ctrl Pts',(-33.3216771869561,33.0187790672924,43.9983189702246));
#24235=CARTESIAN_POINT('Ctrl Pts',(-33.6583243146476,32.5820417578923,44.0353622332978));
#24236=CARTESIAN_POINT('Ctrl Pts',(-33.7570895101463,31.9619396031405,44.0724054963711));
#24237=CARTESIAN_POINT('Ctrl Pts',(-33.5727783555304,31.442227986679,44.1094487594444));
#24238=CARTESIAN_POINT('Ctrl Pts',(-33.3884672009146,30.9225163702175,44.1464920225176));
#24239=CARTESIAN_POINT('Ctrl Pts',(-32.9210796961843,30.5031952920463,44.1835352855908));
#24240=CARTESIAN_POINT('Ctrl Pts',(-32.3844898291976,30.376143803867,44.220578548664));
#24241=CARTESIAN_POINT('Ctrl Pts',(-31.8478999622109,30.2490923156877,44.2576218117373));
#24242=CARTESIAN_POINT('Ctrl Pts',(-31.2421077329678,30.4143104175003,44.2946650748106));
#24243=CARTESIAN_POINT('Ctrl Pts',(-30.8443203808,30.796195201771,44.3317083378838));
#24244=CARTESIAN_POINT('Ctrl Pts',(-30.5229828116778,31.1046864788154,44.361632346386));
#24245=CARTESIAN_POINT('Ctrl Pts',(-30.337381098238,31.5545659673038,44.3915563548881));
#24246=CARTESIAN_POINT('Ctrl Pts',(-30.333294480282,32.0014513626233,44.4214803633902));
#24247=CARTESIAN_POINT('Ctrl Pts',(-30.3314442636938,31.9994792812594,44.2285196366098));
#24248=CARTESIAN_POINT('Ctrl Pts',(-30.3313271354078,31.9709101402436,44.2266010535305));
#24249=CARTESIAN_POINT('Ctrl Pts',(-30.3319973688349,31.9423466088594,44.2246824704513));
#24250=CARTESIAN_POINT('Ctrl Pts',(-30.3334722232713,31.9138246840243,44.2227638873721));
#24251=CARTESIAN_POINT('Ctrl Pts',(-30.36194814463,31.3631343456928,44.1857206242988));
#24252=CARTESIAN_POINT('Ctrl Pts',(-30.6903738960118,30.8279542627113,44.1486773612256));
#24253=CARTESIAN_POINT('Ctrl Pts',(-31.1684636343982,30.5531799391802,44.1116340981524));
#24254=CARTESIAN_POINT('Ctrl Pts',(-31.6465533727846,30.2784056156492,44.0745908350791));
#24255=CARTESIAN_POINT('Ctrl Pts',(-32.2743070981754,30.2640370515686,44.0375475720059));
#24256=CARTESIAN_POINT('Ctrl Pts',(-32.7644681096866,30.5166492239095,44.0005043089326));
#24257=CARTESIAN_POINT('Ctrl Pts',(-33.2546291211977,30.7692613962504,43.9634610458594));
#24258=CARTESIAN_POINT('Ctrl Pts',(-33.6071974188292,31.2888543050128,43.9264177827861));
#24259=CARTESIAN_POINT('Ctrl Pts',(-33.6608396613031,31.8376650526052,43.8893745197129));
#24260=CARTESIAN_POINT('Ctrl Pts',(-33.7144819037769,32.3864758001977,43.8523312566396));
#24261=CARTESIAN_POINT('Ctrl Pts',(-33.4691980910932,32.9645043866202,43.8152879935664));
#24262=CARTESIAN_POINT('Ctrl Pts',(-33.0372287659473,33.307248064791,43.7782447304932));
#24263=CARTESIAN_POINT('Ctrl Pts',(-32.6052594408015,33.6499917429618,43.7412014674199));
#24264=CARTESIAN_POINT('Ctrl Pts',(-31.9866046031935,33.757450512881,43.7041582043467));
#24265=CARTESIAN_POINT('Ctrl Pts',(-31.4643573522818,33.5804518244296,43.6671149412734));
#24266=CARTESIAN_POINT('Ctrl Pts',(-30.94211010137,33.4034531359782,43.6300716782002));
#24267=CARTESIAN_POINT('Ctrl Pts',(-30.5162704371545,32.9419969891563,43.593028415127));
#24268=CARTESIAN_POINT('Ctrl Pts',(-30.3817002809903,32.4072432139639,43.5559851520537));
#24269=CARTESIAN_POINT('Ctrl Pts',(-30.3484415235646,32.2750798383797,43.5468299802391));
#24270=CARTESIAN_POINT('Ctrl Pts',(-30.3329741425732,32.1384392838872,43.5376748084244));
#24271=CARTESIAN_POINT('Ctrl Pts',(-30.3342156580691,32.0015219727962,43.5285196366098));
#24272=CARTESIAN_POINT('Origin',(-32.,32.,48.));
#24273=CARTESIAN_POINT('',(-30.3366133324916,31.9995845730415,42.8285196366098));
#24274=CARTESIAN_POINT('',(-30.3335914213191,31.9985061360497,43.0214803633902));
#24275=CARTESIAN_POINT('',(-30.334,32.,48.));
#24276=CARTESIAN_POINT('Ctrl Pts',(-30.3335914213191,31.9985061360497,43.0214803633902));
#24277=CARTESIAN_POINT('Ctrl Pts',(-30.3376271892743,32.435776657828,43.050747127749));
#24278=CARTESIAN_POINT('Ctrl Pts',(-30.5143062601661,32.8759335579088,43.0800138921079));
#24279=CARTESIAN_POINT('Ctrl Pts',(-30.82319727105,33.1831638556262,43.1092806564668));
#24280=CARTESIAN_POINT('Ctrl Pts',(-31.2141639948336,33.5720285966297,43.14632391954));
#24281=CARTESIAN_POINT('Ctrl Pts',(-31.8169374352255,33.7479417146696,43.1833671826133));
#24282=CARTESIAN_POINT('Ctrl Pts',(-32.3556917358311,33.6304063187777,43.2204104456866));
#24283=CARTESIAN_POINT('Ctrl Pts',(-32.8944460364368,33.5128709228859,43.2574537087598));
#24284=CARTESIAN_POINT('Ctrl Pts',(-33.3691811972561,33.1018870130622,43.294496971833));
#24285=CARTESIAN_POINT('Ctrl Pts',(-33.5626609820717,32.585518598986,43.3315402349062));
#24286=CARTESIAN_POINT('Ctrl Pts',(-33.7561407668874,32.0691501849098,43.3685834979795));
#24287=CARTESIAN_POINT('Ctrl Pts',(-33.6683651756993,31.447397266581,43.4056267610527));
#24288=CARTESIAN_POINT('Ctrl Pts',(-33.3394998434811,31.0047706076013,43.442670024126));
#24289=CARTESIAN_POINT('Ctrl Pts',(-33.0106345112629,30.5621439486216,43.4797132871992));
#24290=CARTESIAN_POINT('Ctrl Pts',(-32.4406794380146,30.2986435489909,43.5167565502724));
#24291=CARTESIAN_POINT('Ctrl Pts',(-31.8904429746054,30.3348457630668,43.5537998133457));
#24292=CARTESIAN_POINT('Ctrl Pts',(-31.3402065111961,30.3710479771428,43.5908430764189));
#24293=CARTESIAN_POINT('Ctrl Pts',(-30.8096886576259,30.7069528049254,43.6278863394922));
#24294=CARTESIAN_POINT('Ctrl Pts',(-30.5416515071744,31.1888520184591,43.6649296025654));
#24295=CARTESIAN_POINT('Ctrl Pts',(-30.4052550927318,31.4340766999556,43.6837798561737));
#24296=CARTESIAN_POINT('Ctrl Pts',(-30.3368280575922,31.7171066283268,43.7026301097819));
#24297=CARTESIAN_POINT('Ctrl Pts',(-30.3367054458351,32.0000809143127,43.7214803633902));
#24298=CARTESIAN_POINT('Ctrl Pts',(-30.3342156580691,32.0015219727962,43.5285196366098));
#24299=CARTESIAN_POINT('Ctrl Pts',(-30.3379975092617,31.5844503389818,43.5006315453512));
#24300=CARTESIAN_POINT('Ctrl Pts',(-30.4968224279369,31.1648106605338,43.4727434540926));
#24301=CARTESIAN_POINT('Ctrl Pts',(-30.7800935628365,30.8613300297991,43.444855362834));
#24302=CARTESIAN_POINT('Ctrl Pts',(-31.1563576489599,30.4582220243893,43.4078120997608));
#24303=CARTESIAN_POINT('Ctrl Pts',(-31.7521864693196,30.2600574171324,43.3707688366875));
#24304=CARTESIAN_POINT('Ctrl Pts',(-32.2949319865817,30.3575152552835,43.3337255736143));
#24305=CARTESIAN_POINT('Ctrl Pts',(-32.8376775038437,30.4549730934347,43.296682310541));
#24306=CARTESIAN_POINT('Ctrl Pts',(-33.3273397180079,30.8480533769938,43.2596390474678));
#24307=CARTESIAN_POINT('Ctrl Pts',(-33.5398518547276,31.3568847045873,43.2225957843945));
#24308=CARTESIAN_POINT('Ctrl Pts',(-33.7523639914472,31.8657160321808,43.1855525213213));
#24309=CARTESIAN_POINT('Ctrl Pts',(-33.6877260507221,32.4902984038087,43.1485092582481));
#24310=CARTESIAN_POINT('Ctrl Pts',(-33.3755160041951,32.9448263029854,43.1114659951748));
#24311=CARTESIAN_POINT('Ctrl Pts',(-33.0633059576681,33.3993542021622,43.0744227321016));
#24312=CARTESIAN_POINT('Ctrl Pts',(-32.5035238053391,33.6838276288878,43.0373794690283));
#24313=CARTESIAN_POINT('Ctrl Pts',(-31.9523228239278,33.6680731051537,43.0003362059551));
#24314=CARTESIAN_POINT('Ctrl Pts',(-31.4011218425165,33.6523185814197,42.9632929428818));
#24315=CARTESIAN_POINT('Ctrl Pts',(-30.8585020320229,33.3363361072259,42.9262496798086));
#24316=CARTESIAN_POINT('Ctrl Pts',(-30.5727632772645,32.864717510685,42.8892064167354));
#24317=CARTESIAN_POINT('Ctrl Pts',(-30.4167244230102,32.6071716782637,42.8689774900269));
#24318=CARTESIAN_POINT('Ctrl Pts',(-30.3372909516162,32.3032130626764,42.8487485633183));
#24319=CARTESIAN_POINT('Ctrl Pts',(-30.3366133324916,31.9995845730415,42.8285196366098));
#24320=CARTESIAN_POINT('Origin',(-32.,32.,48.));
#24321=CARTESIAN_POINT('',(-30.3326930047543,31.9986962112692,42.1285196366098));
#24322=CARTESIAN_POINT('',(-30.3317921991812,32.000855278924,42.3214803633902));
#24323=CARTESIAN_POINT('',(-30.334,32.,48.));
#24324=CARTESIAN_POINT('Ctrl Pts',(-30.3317921991812,32.000855278924,42.3214803633902));
#24325=CARTESIAN_POINT('Ctrl Pts',(-30.331484649223,32.049981083659,42.3247776195697));
#24326=CARTESIAN_POINT('Ctrl Pts',(-30.3334666242309,32.0990817223638,42.3280748757492));
#24327=CARTESIAN_POINT('Ctrl Pts',(-30.3378188894502,32.1479713507645,42.3313721319287));
#24328=CARTESIAN_POINT('Ctrl Pts',(-30.3867147279015,32.6972254177245,42.368415395002));
#24329=CARTESIAN_POINT('Ctrl Pts',(-30.734778204715,33.219846689238,42.4054586580752));
#24330=CARTESIAN_POINT('Ctrl Pts',(-31.2227371783014,33.476686743959,42.4425019211484));
#24331=CARTESIAN_POINT('Ctrl Pts',(-31.7106961518878,33.7335267986801,42.4795451842217));
#24332=CARTESIAN_POINT('Ctrl Pts',(-32.3385506222471,33.7245856366086,42.5165884472949));
#24333=CARTESIAN_POINT('Ctrl Pts',(-32.8189978800188,33.4539545644561,42.5536317103681));
#24334=CARTESIAN_POINT('Ctrl Pts',(-33.2994451377906,33.1833234923036,42.5906749734414));
#24335=CARTESIAN_POINT('Ctrl Pts',(-33.6324851829748,32.6510025100702,42.6277182365147));
#24336=CARTESIAN_POINT('Ctrl Pts',(-33.6657206503217,32.100578873737,42.6647614995879));
#24337=CARTESIAN_POINT('Ctrl Pts',(-33.6989561176687,31.5501552374038,42.7018047626611));
#24338=CARTESIAN_POINT('Ctrl Pts',(-33.4323870071784,30.9816289469708,42.7388480257344));
#24339=CARTESIAN_POINT('Ctrl Pts',(-32.9879939218415,30.6551545194728,42.7758912888076));
#24340=CARTESIAN_POINT('Ctrl Pts',(-32.5436008365046,30.3286800919748,42.8129345518808));
#24341=CARTESIAN_POINT('Ctrl Pts',(-31.9213837763209,30.2442575274118,42.8499778149541));
#24342=CARTESIAN_POINT('Ctrl Pts',(-31.4060658823589,30.4405181491037,42.8870210780273));
#24343=CARTESIAN_POINT('Ctrl Pts',(-30.8907479883968,30.6367787707956,42.9240643411006));
#24344=CARTESIAN_POINT('Ctrl Pts',(-30.4823292606563,31.1137225787423,42.9611076041738));
#24345=CARTESIAN_POINT('Ctrl Pts',(-30.3676999003737,31.6531026646991,42.9981508672471));
#24346=CARTESIAN_POINT('Ctrl Pts',(-30.3436357386635,31.7663348207516,43.0059273659614));
#24347=CARTESIAN_POINT('Ctrl Pts',(-30.3325190737261,31.8823185859417,43.0137038646758));
#24348=CARTESIAN_POINT('Ctrl Pts',(-30.3335914213191,31.9985061360497,43.0214803633902));
#24349=CARTESIAN_POINT('Ctrl Pts',(-30.3366133324916,31.9995845730415,42.8285196366098));
#24350=CARTESIAN_POINT('Ctrl Pts',(-30.3360500937171,31.7472077846831,42.8117053002451));
#24351=CARTESIAN_POINT('Ctrl Pts',(-30.3898990963236,31.4950590796035,42.7948909638804));
#24352=CARTESIAN_POINT('Ctrl Pts',(-30.4993953032921,31.2699817889122,42.7780766275156));
#24353=CARTESIAN_POINT('Ctrl Pts',(-30.740623783101,30.7741193825682,42.7410333644424));
#24354=CARTESIAN_POINT('Ctrl Pts',(-31.2519384417417,30.4096492887681,42.7039901013691));
#24355=CARTESIAN_POINT('Ctrl Pts',(-31.7993644708408,30.3433508944012,42.6669468382959));
#24356=CARTESIAN_POINT('Ctrl Pts',(-32.3467904999399,30.2770525000343,42.6299035752227));
#24357=CARTESIAN_POINT('Ctrl Pts',(-32.9303278994973,30.5089258051006,42.5928603121494));
#24358=CARTESIAN_POINT('Ctrl Pts',(-33.2829531058532,30.9328671429222,42.5558170490762));
#24359=CARTESIAN_POINT('Ctrl Pts',(-33.6355783122092,31.3568084807439,42.518773786003));
#24360=CARTESIAN_POINT('Ctrl Pts',(-33.7572913253637,31.972817851321,42.4817305229297));
#24361=CARTESIAN_POINT('Ctrl Pts',(-33.5923969576212,32.4990121121331,42.4446872598564));
#24362=CARTESIAN_POINT('Ctrl Pts',(-33.4275025898788,33.0252063729452,42.4076439967832));
#24363=CARTESIAN_POINT('Ctrl Pts',(-32.9760008412393,33.4615855239924,42.3706007337099));
#24364=CARTESIAN_POINT('Ctrl Pts',(-32.444496409946,33.6084660091537,42.3335574706367));
#24365=CARTESIAN_POINT('Ctrl Pts',(-31.9129919786527,33.755346494315,42.2965142075635));
#24366=CARTESIAN_POINT('Ctrl Pts',(-31.3014848647057,33.6127283135904,42.2594709444903));
#24367=CARTESIAN_POINT('Ctrl Pts',(-30.8897975141205,33.245870442855,42.222427681417));
#24368=CARTESIAN_POINT('Ctrl Pts',(-30.5419092076928,32.9358644075266,42.1911249998146));
#24369=CARTESIAN_POINT('Ctrl Pts',(-30.3367074574263,32.4657341253069,42.1598223182122));
#24370=CARTESIAN_POINT('Ctrl Pts',(-30.3326930047543,31.9986962112692,42.1285196366098));
#24371=CARTESIAN_POINT('Origin',(-32.,32.,48.));
#24372=CARTESIAN_POINT('',(-30.3325261571163,32.001210199007,41.4285196366098));
#24373=CARTESIAN_POINT('',(-30.3361589164137,32.0009454232939,41.6214803633902));
#24374=CARTESIAN_POINT('',(-30.334,32.,48.));
#24375=CARTESIAN_POINT('',(-33.2690708798524,33.0793586530485,41.));
#24376=CARTESIAN_POINT('Ctrl Pts',(-30.3325261571163,32.001210199007,41.4285196366098));
#24377=CARTESIAN_POINT('Ctrl Pts',(-30.3364619003144,31.5283280072703,41.3968095469596));
#24378=CARTESIAN_POINT('Ctrl Pts',(-30.5476791715277,31.0524653264148,41.3650994573094));
#24379=CARTESIAN_POINT('Ctrl Pts',(-30.9035244685572,30.7421792451538,41.3333893676592));
#24380=CARTESIAN_POINT('Ctrl Pts',(-31.3192177414759,30.3797075819416,41.2963461045859));
#24381=CARTESIAN_POINT('Ctrl Pts',(-31.9322786735049,30.243191197321,41.2593028415127));
#24382=CARTESIAN_POINT('Ctrl Pts',(-32.4621353555657,30.3962172700897,41.2222595784394));
#24383=CARTESIAN_POINT('Ctrl Pts',(-32.9919920376265,30.5492433428584,41.1852163153662));
#24384=CARTESIAN_POINT('Ctrl Pts',(-33.4386444697191,30.9918118730164,41.148173052293));
#24385=CARTESIAN_POINT('Ctrl Pts',(-33.5976357473726,31.5188493258702,41.1111297892197));
#24386=CARTESIAN_POINT('Ctrl Pts',(-33.7566270250261,32.0458867787241,41.0740865261465));
#24387=CARTESIAN_POINT('Ctrl Pts',(-33.6279571482407,32.6573931542737,41.0370432630732));
#24388=CARTESIAN_POINT('Ctrl Pts',(-33.2690708798524,33.0793586530485,41.));
#24389=CARTESIAN_POINT('',(-30.7285328989217,33.0812099237989,41.));
#24390=CARTESIAN_POINT('Origin',(-32.,32.,41.));
#24391=CARTESIAN_POINT('Ctrl Pts',(-30.728531577822,33.0812109444531,41.));
#24392=CARTESIAN_POINT('Ctrl Pts',(-31.0793196648972,33.4926490838295,41.0363148168372));
#24393=CARTESIAN_POINT('Ctrl Pts',(-31.6491071451624,33.71867271397,41.0726296336745));
#24394=CARTESIAN_POINT('Ctrl Pts',(-32.1864002116813,33.6582000435223,41.1089444505117));
#24395=CARTESIAN_POINT('Ctrl Pts',(-32.734470948199,33.5965143395801,41.145987713585));
#24396=CARTESIAN_POINT('Ctrl Pts',(-33.2487305721424,33.2367232829171,41.1830309766582));
#24397=CARTESIAN_POINT('Ctrl Pts',(-33.4941904525548,32.7430255098163,41.2200742397314));
#24398=CARTESIAN_POINT('Ctrl Pts',(-33.7396503329672,32.2493277367155,41.2571175028047));
#24399=CARTESIAN_POINT('Ctrl Pts',(-33.7163104698485,31.621723247177,41.2941607658779));
#24400=CARTESIAN_POINT('Ctrl Pts',(-33.434682746762,31.1476214758446,41.3312040289512));
#24401=CARTESIAN_POINT('Ctrl Pts',(-33.1530550236755,30.6735197045122,41.3682472920244));
#24402=CARTESIAN_POINT('Ctrl Pts',(-32.6131394406212,30.352920651386,41.4052905550976));
#24403=CARTESIAN_POINT('Ctrl Pts',(-32.0620834325308,30.3324171571387,41.4423338181709));
#24404=CARTESIAN_POINT('Ctrl Pts',(-31.5110274244403,30.3119136628915,41.4793770812441));
#24405=CARTESIAN_POINT('Ctrl Pts',(-30.9488309913136,30.5915057275232,41.5164203443174));
#24406=CARTESIAN_POINT('Ctrl Pts',(-30.6327092444556,31.0433098742836,41.5534636073906));
#24407=CARTESIAN_POINT('Ctrl Pts',(-30.4392275877983,31.3198356611636,41.5761358593905));
#24408=CARTESIAN_POINT('Ctrl Pts',(-30.3379261613561,31.6608725508196,41.5988081113903));
#24409=CARTESIAN_POINT('Ctrl Pts',(-30.3361589164137,32.0009454232939,41.6214803633902));
#24410=CARTESIAN_POINT('Origin',(-32.,32.,39.4540747194623));
#24411=CARTESIAN_POINT('',(-29.9467153330669,32.0018314293989,53.7459252805377));
#24412=CARTESIAN_POINT('',(-29.9453611728806,31.9981689810755,53.8040747194623));
#24413=CARTESIAN_POINT('',(-29.94525,32.0000000000002,39.4540747194623));
#24414=CARTESIAN_POINT('',(-32.3836679988468,34.0186125009919,54.));
#24415=CARTESIAN_POINT('Ctrl Pts',(-29.9453611728806,31.9981689810755,53.8040747194623));
#24416=CARTESIAN_POINT('Ctrl Pts',(-29.9506279893844,32.5196386238579,53.832339883235));
#24417=CARTESIAN_POINT('Ctrl Pts',(-30.4182837037984,33.7322194813403,53.8976483100809));
#24418=CARTESIAN_POINT('Ctrl Pts',(-31.7124802469751,34.146181938655,53.9629567369268));
#24419=CARTESIAN_POINT('Ctrl Pts',(-32.3836679988468,34.0186125009919,54.));
#24420=CARTESIAN_POINT('',(-33.3415658188825,33.5612633204521,54.));
#24421=CARTESIAN_POINT('Origin',(-32.,32.,54.));
#24422=CARTESIAN_POINT('Ctrl Pts',(-29.9467153330669,32.0018314293989,53.7459252805377));
#24423=CARTESIAN_POINT('Ctrl Pts',(-29.9450489223381,32.2111833794062,53.7572587737813));
#24424=CARTESIAN_POINT('Ctrl Pts',(-30.0707451594838,33.1027824480144,53.8056355300982));
#24425=CARTESIAN_POINT('Ctrl Pts',(-31.3453228671131,34.3305891564746,53.8903271032523));
#24426=CARTESIAN_POINT('Ctrl Pts',(-32.8352371619566,33.9952106642201,53.9636851831628));
#24427=CARTESIAN_POINT('Ctrl Pts',(-33.3415672325378,33.5612648174638,54.));
#24428=CARTESIAN_POINT('Origin',(-32.,32.,39.4540747194623));
#24429=CARTESIAN_POINT('',(-29.9479916519948,31.9988943668812,53.0459252805377));
#24430=CARTESIAN_POINT('',(-29.9421906513588,32.0007573773506,53.1040747194623));
#24431=CARTESIAN_POINT('',(-29.94525,32.0000000000002,39.4540747194623));
#24432=CARTESIAN_POINT('Ctrl Pts',(-29.9421906513588,32.0007573773506,53.1040747194623));
#24433=CARTESIAN_POINT('Ctrl Pts',(-29.9419903991083,32.0429235489439,53.1063703750556));
#24434=CARTESIAN_POINT('Ctrl Pts',(-29.9622810371399,32.7652974030863,53.1457092937221));
#24435=CARTESIAN_POINT('Ctrl Pts',(-30.8113288145004,34.117796910195,53.2220914754619));
#24436=CARTESIAN_POINT('Ctrl Pts',(-33.1343255579885,34.1473076805079,53.3332212646816));
#24437=CARTESIAN_POINT('Ctrl Pts',(-34.4195104110039,32.2117840240242,53.4443510539014));
#24438=CARTESIAN_POINT('Ctrl Pts',(-33.4897707576895,30.0821245375598,53.5554808431211));
#24439=CARTESIAN_POINT('Ctrl Pts',(-31.1978269251376,29.7083052230924,53.6666106323408));
#24440=CARTESIAN_POINT('Ctrl Pts',(-30.0344356528229,30.992528820682,53.7494752577879));
#24441=CARTESIAN_POINT('Ctrl Pts',(-29.9437254972964,31.8362200766428,53.7952966201617));
#24442=CARTESIAN_POINT('Ctrl Pts',(-29.9453611728806,31.9981689810755,53.8040747194623));
#24443=CARTESIAN_POINT('Ctrl Pts',(-29.9479916519948,31.9988943668812,53.0459252805377));
#24444=CARTESIAN_POINT('Ctrl Pts',(-29.9500185408881,32.4134550879906,53.0683325286752));
#24445=CARTESIAN_POINT('Ctrl Pts',(-30.2732453084617,33.516265749558,53.127783039886));
#24446=CARTESIAN_POINT('Ctrl Pts',(-32.0730427769752,34.4274726540847,53.2242768141699));
#24447=CARTESIAN_POINT('Ctrl Pts',(-34.0790038841791,33.2553327473947,53.3354066033897));
#24448=CARTESIAN_POINT('Ctrl Pts',(-34.182240985042,30.9342477393896,53.4465363926094));
#24449=CARTESIAN_POINT('Ctrl Pts',(-32.288398343005,29.5886824305611,53.5576661818291));
#24450=CARTESIAN_POINT('Ctrl Pts',(-30.3505279832561,30.3618200065023,53.6574624778052));
#24451=CARTESIAN_POINT('Ctrl Pts',(-29.950495547636,31.5269213260117,53.7202155107081));
#24452=CARTESIAN_POINT('Ctrl Pts',(-29.9467153330669,32.0018314293989,53.7459252805377));
#24453=CARTESIAN_POINT('Origin',(-32.,32.,39.4540747194623));
#24454=CARTESIAN_POINT('',(-29.9426288446654,31.9988731525755,52.3459252805377));
#24455=CARTESIAN_POINT('',(-29.9475562773048,32.0013942151196,52.4040747194623));
#24456=CARTESIAN_POINT('',(-29.94525,32.0000000000002,39.4540747194623));
#24457=CARTESIAN_POINT('Ctrl Pts',(-29.9475562773048,32.0013942151196,52.4040747194623));
#24458=CARTESIAN_POINT('Ctrl Pts',(-29.9460125610086,32.2486122196956,52.4174441299495));
#24459=CARTESIAN_POINT('Ctrl Pts',(-30.1017872573193,33.1789290640202,52.4678568035099));
#24460=CARTESIAN_POINT('Ctrl Pts',(-31.4859339899109,34.3735521292407,52.5553127401435));
#24461=CARTESIAN_POINT('Ctrl Pts',(-33.7152268428034,33.7193027479294,52.6664425293632));
#24462=CARTESIAN_POINT('Ctrl Pts',(-34.3747678520742,31.4915687675265,52.777572318583));
#24463=CARTESIAN_POINT('Ctrl Pts',(-32.8609368582137,29.729140329846,52.8887021078027));
#24464=CARTESIAN_POINT('Ctrl Pts',(-30.6067538535749,30.0384637365273,52.9975362414292));
#24465=CARTESIAN_POINT('Ctrl Pts',(-29.945221718656,31.3625198369552,53.0693271119824));
#24466=CARTESIAN_POINT('Ctrl Pts',(-29.9421906513588,32.0007573773506,53.1040747194623));
#24467=CARTESIAN_POINT('Ctrl Pts',(-29.9426288446654,31.9988731525755,52.3459252805377));
#24468=CARTESIAN_POINT('Ctrl Pts',(-29.9466921151103,32.6141860878724,52.3794062835691));
#24469=CARTESIAN_POINT('Ctrl Pts',(-30.5667600306827,33.917382824163,52.4499305496737));
#24470=CARTESIAN_POINT('Ctrl Pts',(-32.7830045631024,34.2988945540426,52.5574980788516));
#24471=CARTESIAN_POINT('Ctrl Pts',(-34.3560464259567,32.5891179074725,52.6686278680713));
#24472=CARTESIAN_POINT('Ctrl Pts',(-33.7728594492291,30.3401856422308,52.7797576572911));
#24473=CARTESIAN_POINT('Ctrl Pts',(-31.5671721178615,29.6103000479543,52.8908874465108));
#24474=CARTESIAN_POINT('Ctrl Pts',(-30.1224675846331,30.7736324025542,52.979609987593));
#24475=CARTESIAN_POINT('Ctrl Pts',(-29.9466677243116,31.7281106959594,53.0312892656019));
#24476=CARTESIAN_POINT('Ctrl Pts',(-29.9479916519948,31.9988943668812,53.0459252805377));
#24477=CARTESIAN_POINT('Origin',(-32.,32.,39.4540747194623));
#24478=CARTESIAN_POINT('',(-29.9445979340372,32.0018240974026,51.6459252805377));
#24479=CARTESIAN_POINT('',(-29.9472436463387,31.9984585483392,51.7040747194623));
#24480=CARTESIAN_POINT('',(-29.94525,32.0000000000002,39.4540747194623));
#24481=CARTESIAN_POINT('Ctrl Pts',(-29.9472436463387,31.9984585483392,51.7040747194623));
#24482=CARTESIAN_POINT('Ctrl Pts',(-29.9503946737569,32.450271766422,51.7285178848434));
#24483=CARTESIAN_POINT('Ctrl Pts',(-30.3199519290529,33.5914867339453,51.7900043132976));
#24484=CARTESIAN_POINT('Ctrl Pts',(-32.2059544077473,34.4198337491439,51.8885340048253));
#24485=CARTESIAN_POINT('Ctrl Pts',(-34.1446539107159,33.1395051684107,51.9996637940449));
#24486=CARTESIAN_POINT('Ctrl Pts',(-34.1205894982053,30.816313858696,52.1107935832648));
#24487=CARTESIAN_POINT('Ctrl Pts',(-32.1557844039238,29.5764191824004,52.2219233724843));
#24488=CARTESIAN_POINT('Ctrl Pts',(-30.3019343182528,30.4368848986496,52.3196837512169));
#24489=CARTESIAN_POINT('Ctrl Pts',(-29.9502898093531,31.5636335073777,52.3804008668763));
#24490=CARTESIAN_POINT('Ctrl Pts',(-29.9475562773048,32.0013942151196,52.4040747194623));
#24491=CARTESIAN_POINT('Ctrl Pts',(-29.9445979340372,32.0018240974026,51.6459252805377));
#24492=CARTESIAN_POINT('Ctrl Pts',(-29.9433235785776,32.1402143164981,51.6534367753897));
#24493=CARTESIAN_POINT('Ctrl Pts',(-30.019149581319,32.9596933491072,51.697991533315));
#24494=CARTESIAN_POINT('Ctrl Pts',(-31.1194585135859,34.2633294087954,51.7795895543135));
#24495=CARTESIAN_POINT('Ctrl Pts',(-33.423850742076,33.9673998993839,51.8907193435332));
#24496=CARTESIAN_POINT('Ctrl Pts',(-34.4251502183154,31.8709273485123,52.001849132753));
#24497=CARTESIAN_POINT('Ctrl Pts',(-33.2069785027727,29.8925806669829,52.1129789219727));
#24498=CARTESIAN_POINT('Ctrl Pts',(-30.8841931736715,29.8429213477129,52.2241087111924));
#24499=CARTESIAN_POINT('Ctrl Pts',(-29.9747293817875,31.1875940441121,52.3017574973808));
#24500=CARTESIAN_POINT('Ctrl Pts',(-29.9421965270932,31.9334060373702,52.3423630204959));
#24501=CARTESIAN_POINT('Ctrl Pts',(-29.9426288446654,31.9988731525755,52.3459252805377));
#24502=CARTESIAN_POINT('Origin',(-32.,32.,39.4540747194623));
#24503=CARTESIAN_POINT('',(-29.948590975573,31.9999806721044,50.9459252805377));
#24504=CARTESIAN_POINT('',(-29.942011007514,31.9994845671788,51.0040747194623));
#24505=CARTESIAN_POINT('',(-29.94525,32.0000000000002,39.4540747194623));
#24506=CARTESIAN_POINT('Ctrl Pts',(-29.942011007514,31.9994845671788,51.0040747194623));
#24507=CARTESIAN_POINT('Ctrl Pts',(-29.9442070892614,32.6516937390639,51.0395916397372));
#24508=CARTESIAN_POINT('Ctrl Pts',(-30.6316982717036,33.9881256658593,51.1121518230854));
#24509=CARTESIAN_POINT('Ctrl Pts',(-32.907797512765,34.2525355120973,51.2217552695069));
#24510=CARTESIAN_POINT('Ctrl Pts',(-34.3847873801667,32.4591314690988,51.3328850587265));
#24511=CARTESIAN_POINT('Ctrl Pts',(-33.6792457006084,30.2455352853812,51.4440148479464));
#24512=CARTESIAN_POINT('Ctrl Pts',(-31.4368765636913,29.6376061806665,51.5551446371659));
#24513=CARTESIAN_POINT('Ctrl Pts',(-30.0897291860077,30.8498858532132,51.6418312610047));
#24514=CARTESIAN_POINT('Ctrl Pts',(-29.9456193373476,31.765555378978,51.6914746217701));
#24515=CARTESIAN_POINT('Ctrl Pts',(-29.9472436463387,31.9984585483392,51.7040747194623));
#24516=CARTESIAN_POINT('Ctrl Pts',(-29.948590975573,31.9999806721044,50.9459252805377));
#24517=CARTESIAN_POINT('Ctrl Pts',(-29.9486198486256,32.3440804588562,50.9645105302836));
#24518=CARTESIAN_POINT('Ctrl Pts',(-30.1938071650696,33.3740627456927,51.0201390431028));
#24519=CARTESIAN_POINT('Ctrl Pts',(-31.8232699686781,34.4221436399707,51.1128108189951));
#24520=CARTESIAN_POINT('Ctrl Pts',(-33.9390244099684,33.4622577248198,51.2239406082149));
#24521=CARTESIAN_POINT('Ctrl Pts',(-34.2802047391973,31.1641293976194,51.3350703974346));
#24522=CARTESIAN_POINT('Ctrl Pts',(-32.5345664187102,29.6309807807203,51.4462001866543));
#24523=CARTESIAN_POINT('Ctrl Pts',(-30.4507580914472,30.2230151239904,51.549818481022));
#24524=CARTESIAN_POINT('Ctrl Pts',(-29.9496081178695,31.4577369409946,51.6163935123165));
#24525=CARTESIAN_POINT('Ctrl Pts',(-29.9445979340372,32.0018240974026,51.6459252805377));
#24526=CARTESIAN_POINT('Origin',(-32.,32.,39.4540747194623));
#24527=CARTESIAN_POINT('',(-29.9445270010734,31.9981860521306,50.2459252805377));
#24528=CARTESIAN_POINT('',(-29.9457313135825,32.001868508926,50.3040747194623));
#24529=CARTESIAN_POINT('',(-29.94525,32.0000000000002,39.4540747194623));
#24530=CARTESIAN_POINT('Ctrl Pts',(-29.9457313135825,32.001868508926,50.3040747194623));
#24531=CARTESIAN_POINT('Ctrl Pts',(-29.9441559642374,32.1780164363184,50.3136221315579));
#24532=CARTESIAN_POINT('Ctrl Pts',(-30.0455183200277,33.0358200312748,50.3602128067267));
#24533=CARTESIAN_POINT('Ctrl Pts',(-31.2448019703849,34.3081786093532,50.4438467449688));
#24534=CARTESIAN_POINT('Ctrl Pts',(-33.5295162861532,33.8864231993434,50.5549765341884));
#24535=CARTESIAN_POINT('Ctrl Pts',(-34.4144338837356,31.738233734696,50.6661063234082));
#24536=CARTESIAN_POINT('Ctrl Pts',(-33.0896877743921,29.8296099173301,50.7772361126279));
#24537=CARTESIAN_POINT('Ctrl Pts',(-30.7676712310498,29.9073035666993,50.8883659018476));
#24538=CARTESIAN_POINT('Ctrl Pts',(-29.9551340465651,31.2632801821069,50.9639787707925));
#24539=CARTESIAN_POINT('Ctrl Pts',(-29.9419166307062,31.9714558201818,51.002548376664));
#24540=CARTESIAN_POINT('Ctrl Pts',(-29.942011007514,31.9994845671788,51.0040747194623));
#24541=CARTESIAN_POINT('Ctrl Pts',(-29.9445270010734,31.9981860521306,50.2459252805377));
#24542=CARTESIAN_POINT('Ctrl Pts',(-29.9495493798654,32.544568869371,50.2755842851775));
#24543=CARTESIAN_POINT('Ctrl Pts',(-30.4542942488099,33.7815642628783,50.3422865528905));
#24544=CARTESIAN_POINT('Ctrl Pts',(-32.5426800327657,34.3671737786953,50.4460320836768));
#24545=CARTESIAN_POINT('Ctrl Pts',(-34.2830552217384,32.828053241641,50.5571618728965));
#24546=CARTESIAN_POINT('Ctrl Pts',(-33.9340030304806,30.5311073577035,50.6682916621162));
#24547=CARTESIAN_POINT('Ctrl Pts',(-31.8149722391133,29.5784760905123,50.779421451336));
#24548=CARTESIAN_POINT('Ctrl Pts',(-30.1913422173688,30.6306870609017,50.8719659908098));
#24549=CARTESIAN_POINT('Ctrl Pts',(-29.948562300188,31.6582366257969,50.9274672672103));
#24550=CARTESIAN_POINT('Ctrl Pts',(-29.948590975573,31.9999806721044,50.9459252805377));
#24551=CARTESIAN_POINT('Origin',(-32.,32.,39.4540747194623));
#24552=CARTESIAN_POINT('',(-29.942679646097,32.0011604784324,49.5459252805377));
#24553=CARTESIAN_POINT('',(-29.9484130486988,31.9993739458711,49.6040747194623));
#24554=CARTESIAN_POINT('',(-29.94525,32.0000000000002,39.4540747194623));
#24555=CARTESIAN_POINT('Ctrl Pts',(-29.9484130486988,31.9993739458711,49.6040747194623));
#24556=CARTESIAN_POINT('Ctrl Pts',(-29.9494558079608,32.381085353687,49.6246958864518));
#24557=CARTESIAN_POINT('Ctrl Pts',(-30.2348077288734,33.4499404032741,49.6823603165144));
#24558=CARTESIAN_POINT('Ctrl Pts',(-31.9562582891885,34.4281884645445,49.7770680096504));
#24559=CARTESIAN_POINT('Ctrl Pts',(-34.0162363552789,33.3538107387165,49.8881977988702));
#24560=CARTESIAN_POINT('Ctrl Pts',(-34.2309767741905,31.040440106281,49.9993275880898));
#24561=CARTESIAN_POINT('Ctrl Pts',(-32.4039514432991,29.6052482825838,50.1104573773096));
#24562=CARTESIAN_POINT('Ctrl Pts',(-30.3959590957835,30.2967181551523,50.2120397544338));
#24563=CARTESIAN_POINT('Ctrl Pts',(-29.9502682048781,31.4945753164748,50.2765788684846));
#24564=CARTESIAN_POINT('Ctrl Pts',(-29.9457313135825,32.001868508926,50.3040747194623));
#24565=CARTESIAN_POINT('Ctrl Pts',(-29.942679646097,32.0011604784324,49.5459252805377));
#24566=CARTESIAN_POINT('Ctrl Pts',(-29.9422212291737,32.0689703493988,49.5496147769981));
#24567=CARTESIAN_POINT('Ctrl Pts',(-29.9760269532423,32.817141878103,49.5903475365318));
#24568=CARTESIAN_POINT('Ctrl Pts',(-30.8915903093585,34.1608890008963,49.6681235591386));
#24569=CARTESIAN_POINT('Ctrl Pts',(-33.2141918809262,34.1032715927325,49.7792533483584));
#24570=CARTESIAN_POINT('Ctrl Pts',(-34.4255782104328,32.1207628319306,49.8903831375781));
#24571=CARTESIAN_POINT('Ctrl Pts',(-33.4171016660518,30.0277332369641,50.0015129267978));
#24572=CARTESIAN_POINT('Ctrl Pts',(-31.1117090447276,29.7397007951857,50.1126427160176));
#24573=CARTESIAN_POINT('Ctrl Pts',(-30.0175818447045,31.0450604521428,50.1941135005975));
#24574=CARTESIAN_POINT('Ctrl Pts',(-29.9432765699345,31.862152089592,50.2385410221043));
#24575=CARTESIAN_POINT('Ctrl Pts',(-29.9445270010734,31.9981860521306,50.2459252805377));
#24576=CARTESIAN_POINT('Origin',(-32.,32.,39.4540747194623));
#24577=CARTESIAN_POINT('',(-29.9480290143483,32.0010746754496,48.8459252805377));
#24578=CARTESIAN_POINT('',(-29.9434378972346,31.9984640574522,48.9040747194623));
#24579=CARTESIAN_POINT('',(-29.94525,32.0000000000002,39.4540747194623));
#24580=CARTESIAN_POINT('Ctrl Pts',(-29.9434378972346,31.9984640574522,48.9040747194623));
#24581=CARTESIAN_POINT('Ctrl Pts',(-29.948302105761,32.5815526445705,48.9357696413457));
#24582=CARTESIAN_POINT('Ctrl Pts',(-30.5126875679984,33.8543562281369,49.0045078263022));
#24583=CARTESIAN_POINT('Ctrl Pts',(-32.6715753542565,34.3338806953585,49.110289274332));
#24584=CARTESIAN_POINT('Ctrl Pts',(-34.3249986620041,32.7017077584658,49.2214190635518));
#24585=CARTESIAN_POINT('Ctrl Pts',(-33.8506084078462,30.4273394907288,49.3325488527714));
#24586=CARTESIAN_POINT('Ctrl Pts',(-31.6825614078399,29.5922530662839,49.4436786419912));
#24587=CARTESIAN_POINT('Ctrl Pts',(-30.1534240551937,30.7067805031385,49.5341872642215));
#24588=CARTESIAN_POINT('Ctrl Pts',(-29.9475826256291,31.6953901112685,49.5876526233785));
#24589=CARTESIAN_POINT('Ctrl Pts',(-29.9484130486988,31.9993739458711,49.6040747194623));
#24590=CARTESIAN_POINT('Ctrl Pts',(-29.9480290143483,32.0010746754496,48.8459252805377));
#24591=CARTESIAN_POINT('Ctrl Pts',(-29.9467335107896,32.2742244015351,48.860688531892));
#24592=CARTESIAN_POINT('Ctrl Pts',(-30.1246039063867,33.2311300215956,48.9124950463196));
#24593=CARTESIAN_POINT('Ctrl Pts',(-31.5753615017921,34.3911703122827,49.0013448238203));
#24594=CARTESIAN_POINT('Ctrl Pts',(-33.7785362981989,33.6537297096236,49.1124746130401));
#24595=CARTESIAN_POINT('Ctrl Pts',(-34.354013961917,31.4028136106688,49.2236044022597));
#24596=CARTESIAN_POINT('Ctrl Pts',(-32.7751235759071,29.6984360190133,49.3347341914796));
#24597=CARTESIAN_POINT('Ctrl Pts',(-30.5628189733967,30.0870788403981,49.4421744842387));
#24598=CARTESIAN_POINT('Ctrl Pts',(-29.9468238243703,31.3881460374325,49.5125715139249));
#24599=CARTESIAN_POINT('Ctrl Pts',(-29.942679646097,32.0011604784324,49.5459252805377));
#24600=CARTESIAN_POINT('Origin',(-32.,32.,39.4540747194623));
#24601=CARTESIAN_POINT('',(-29.9465981926003,31.9982546442336,48.1459252805377));
#24602=CARTESIAN_POINT('',(-29.9436300851387,32.0016034367965,48.2040747194623));
#24603=CARTESIAN_POINT('',(-29.94525,32.0000000000002,39.4540747194623));
#24604=CARTESIAN_POINT('Ctrl Pts',(-29.9436300851387,32.0016034367965,48.2040747194624));
#24605=CARTESIAN_POINT('Ctrl Pts',(-29.9427254430368,32.1069589624514,48.2098001331663));
#24606=CARTESIAN_POINT('Ctrl Pts',(-29.9979858700552,32.8930102198204,48.2525688099435));
#24607=CARTESIAN_POINT('Ctrl Pts',(-31.0116628500012,34.2183782893241,48.3323807497939));
#24608=CARTESIAN_POINT('Ctrl Pts',(-33.3276175991793,34.0335791272928,48.4435105390137));
#24609=CARTESIAN_POINT('Ctrl Pts',(-34.4285511190019,31.9876704012107,48.5546403282334));
#24610=CARTESIAN_POINT('Ctrl Pts',(-33.3069009912542,29.9530455902315,48.6657701174531));
#24611=CARTESIAN_POINT('Ctrl Pts',(-30.9891892490617,29.7917712567763,48.7768999066728));
#24612=CARTESIAN_POINT('Ctrl Pts',(-29.9937470981767,31.1210534634512,48.8563347740093));
#24613=CARTESIAN_POINT('Ctrl Pts',(-29.9426170891911,31.9000711123825,48.8987263782724));
#24614=CARTESIAN_POINT('Ctrl Pts',(-29.9434378972346,31.9984640574522,48.9040747194623));
#24615=CARTESIAN_POINT('Ctrl Pts',(-29.9465981926003,31.9982546442336,48.1459252805377));
#24616=CARTESIAN_POINT('Ctrl Pts',(-29.9504520483336,32.4754533968064,48.1717622867859));
#24617=CARTESIAN_POINT('Ctrl Pts',(-30.3537536488506,33.6427001277731,48.2346425561073));
#24618=CARTESIAN_POINT('Ctrl Pts',(-32.2966122867217,34.4104013084688,48.3345660885019));
#24619=CARTESIAN_POINT('Ctrl Pts',(-34.1859029191172,33.0582257531821,48.4456958777217));
#24620=CARTESIAN_POINT('Ctrl Pts',(-34.0746789050666,30.7375734645635,48.5568256669414));
#24621=CARTESIAN_POINT('Ctrl Pts',(-32.064731256055,29.5722802507307,48.6679554561612));
#24622=CARTESIAN_POINT('Ctrl Pts',(-30.2704276691999,30.4884531134176,48.7643219940265));
#24623=CARTESIAN_POINT('Ctrl Pts',(-29.9499841280138,31.5888498238801,48.8236452688188));
#24624=CARTESIAN_POINT('Ctrl Pts',(-29.9480290143483,32.0010746754496,48.8459252805377));
#24625=CARTESIAN_POINT('Origin',(-32.,32.,39.4540747194623));
#24626=CARTESIAN_POINT('',(-29.9418536204177,31.9999545509509,47.4459252805377));
#24627=CARTESIAN_POINT('',(-29.9484710368218,32.0005167771498,47.5040747194623));
#24628=CARTESIAN_POINT('',(-29.94525,32.0000000000002,39.4540747194623));
#24629=CARTESIAN_POINT('Ctrl Pts',(-29.9484710368218,32.0005167771498,47.5040747194623));
#24630=CARTESIAN_POINT('Ctrl Pts',(-29.9477709447121,32.3115024180602,47.5208738880602));
#24631=CARTESIAN_POINT('Ctrl Pts',(-30.1602326581268,33.307323880596,47.5747163197312));
#24632=CARTESIAN_POINT('Ctrl Pts',(-31.7070250959598,34.4108459640165,47.6656020144756));
#24633=CARTESIAN_POINT('Ctrl Pts',(-33.8664811925721,33.5537890829796,47.7767318036953));
#24634=CARTESIAN_POINT('Ctrl Pts',(-34.317753942888,31.2747212833408,47.8878615929151));
#24635=CARTESIAN_POINT('Ctrl Pts',(-32.6478434196678,29.6594206998682,47.9989913821348));
#24636=CARTESIAN_POINT('Ctrl Pts',(-30.5016137267794,30.1590535721108,48.1043957576505));
#24637=CARTESIAN_POINT('Ctrl Pts',(-29.9485784515881,31.4253117217724,48.1727568700931));
#24638=CARTESIAN_POINT('Ctrl Pts',(-29.9436300851387,32.0016034367965,48.2040747194624));
#24639=CARTESIAN_POINT('Ctrl Pts',(-29.9418541045178,31.9999545574289,47.4459252805377));
#24640=CARTESIAN_POINT('Ctrl Pts',(-29.9420746139188,32.6776207454055,47.4828360416798));
#24641=CARTESIAN_POINT('Ctrl Pts',(-30.6782139520197,34.0357963423805,47.556790065895));
#24642=CARTESIAN_POINT('Ctrl Pts',(-32.9916833736669,34.2168846165047,47.6677873531836));
#24643=CARTESIAN_POINT('Ctrl Pts',(-34.4003366076938,32.3693203030807,47.7789171424033));
#24644=CARTESIAN_POINT('Ctrl Pts',(-33.6122278089259,30.1837580533892,47.890046931623));
#24645=CARTESIAN_POINT('Ctrl Pts',(-31.3486256033116,29.6604007369121,48.0011767208428));
#24646=CARTESIAN_POINT('Ctrl Pts',(-30.0688312378708,30.9020862296657,48.0864695038143));
#24647=CARTESIAN_POINT('Ctrl Pts',(-29.944926663914,31.7912797444886,48.1347190237126));
#24648=CARTESIAN_POINT('Ctrl Pts',(-29.9465981926003,31.9982546442336,48.1459252805377));
#24649=CARTESIAN_POINT('Origin',(-32.,32.,39.4540747194623));
#24650=CARTESIAN_POINT('',(-29.9464657716568,32.0017741341583,46.7459252805377));
#24651=CARTESIAN_POINT('',(-29.9455243558603,31.9981230673818,46.8040747194623));
#24652=CARTESIAN_POINT('',(-29.94525,32.0000000000002,39.4540747194623));
#24653=CARTESIAN_POINT('Ctrl Pts',(-29.9455243558603,31.9981230673818,46.8040747194623));
#24654=CARTESIAN_POINT('Ctrl Pts',(-29.950184034218,32.5122411663057,46.831947642954));
#24655=CARTESIAN_POINT('Ctrl Pts',(-30.4058569233675,33.7169899346219,46.896863829519));
#24656=CARTESIAN_POINT('Ctrl Pts',(-32.4282459959531,34.3905267042144,46.9988232791572));
#24657=CARTESIAN_POINT('Ctrl Pts',(-34.2406047664085,32.9368579600769,47.109953068377));
#24658=CARTESIAN_POINT('Ctrl Pts',(-34.0023863529936,30.6257869706786,47.2210828575967));
#24659=CARTESIAN_POINT('Ctrl Pts',(-31.9316056642948,29.5723808429954,47.3322126468164));
#24660=CARTESIAN_POINT('Ctrl Pts',(-30.2269905365809,30.5640931932684,47.4265432674383));
#24661=CARTESIAN_POINT('Ctrl Pts',(-29.949314693502,31.6257587849068,47.4838306249869));
#24662=CARTESIAN_POINT('Ctrl Pts',(-29.9484710368218,32.0005167771498,47.5040747194623));
#24663=CARTESIAN_POINT('Ctrl Pts',(-29.9464657716568,32.0017741341583,46.7459252805377));
#24664=CARTESIAN_POINT('Ctrl Pts',(-29.9447990356357,32.2038215525088,46.7568665335004));
#24665=CARTESIAN_POINT('Ctrl Pts',(-30.0649944313522,33.0879912801528,46.8048510495363));
#24666=CARTESIAN_POINT('Ctrl Pts',(-31.3319469323119,34.3348915210894,46.8898788286455));
#24667=CARTESIAN_POINT('Ctrl Pts',(-33.5992261538594,33.8277004747262,47.0010086178653));
#24668=CARTESIAN_POINT('Ctrl Pts',(-34.4029109422803,31.64781777448,47.1121384070849));
#24669=CARTESIAN_POINT('Ctrl Pts',(-33.0074776948103,29.7902484277724,47.2232681963048));
#24670=CARTESIAN_POINT('Ctrl Pts',(-30.6900117866906,29.9550197562096,47.3343979855244));
#24671=CARTESIAN_POINT('Ctrl Pts',(-29.9429588184216,31.3149910696256,47.4086170136021));
#24672=CARTESIAN_POINT('Ctrl Pts',(-29.9418533129351,31.9975218772071,47.4457927786065));
#24673=CARTESIAN_POINT('Ctrl Pts',(-29.9418541045178,31.9999545574289,47.4459252805377));
#24674=CARTESIAN_POINT('Origin',(-32.,32.,39.4540747194623));
#24675=CARTESIAN_POINT('',(-29.9481039578725,31.9989927018527,46.0459252805377));
#24676=CARTESIAN_POINT('',(-29.9420942235994,32.000637386216,46.1040747194623));
#24677=CARTESIAN_POINT('',(-29.94525,32.0000000000002,39.4540747194623));
#24678=CARTESIAN_POINT('Ctrl Pts',(-29.9420942235994,32.000637386216,46.1040747194623));
#24679=CARTESIAN_POINT('Ctrl Pts',(-29.9419518628081,32.0355942172137,46.1059781347746));
#24680=CARTESIAN_POINT('Ctrl Pts',(-29.9585993453337,32.7507240077201,46.1449248131603));
#24681=CARTESIAN_POINT('Ctrl Pts',(-30.7889831810305,34.1051011426497,46.2209147546192));
#24682=CARTESIAN_POINT('Ctrl Pts',(-33.1116688972156,34.1592139355736,46.3320445438388));
#24683=CARTESIAN_POINT('Ctrl Pts',(-34.4169672942162,32.2372375503608,46.4431743330586));
#24684=CARTESIAN_POINT('Ctrl Pts',(-33.510283434469,30.0981439317918,46.5543041222783));
#24685=CARTESIAN_POINT('Ctrl Pts',(-31.2214045538376,29.6996083620767,46.665433911498));
#24686=CARTESIAN_POINT('Ctrl Pts',(-30.0404503314131,30.9782872400902,46.7486907772261));
#24687=CARTESIAN_POINT('Ctrl Pts',(-29.9439912969799,31.8289754875258,46.7949043798808));
#24688=CARTESIAN_POINT('Ctrl Pts',(-29.9455243558603,31.9981230673818,46.8040747194623));
#24689=CARTESIAN_POINT('Ctrl Pts',(-29.9481039578725,31.9989927018527,46.0459252805377));
#24690=CARTESIAN_POINT('Ctrl Pts',(-29.9499107896978,32.4063516871941,46.0679402883943));
#24691=CARTESIAN_POINT('Ctrl Pts',(-30.2646015420902,33.5017208474256,46.1269985593241));
#24692=CARTESIAN_POINT('Ctrl Pts',(-32.0474055290543,34.4281198554267,46.2231000933271));
#24693=CARTESIAN_POINT('Ctrl Pts',(-34.0656174727299,33.2771991907512,46.3342298825469));
#24694=CARTESIAN_POINT('Ctrl Pts',(-34.1933987060518,30.9573996773486,46.4453596717666));
#24695=CARTESIAN_POINT('Ctrl Pts',(-32.3138052300136,29.5917766727069,46.5564894609864));
#24696=CARTESIAN_POINT('Ctrl Pts',(-30.3603507968393,30.3475933452302,46.6566779972433));
#24697=CARTESIAN_POINT('Ctrl Pts',(-29.9504420219658,31.5197595262729,46.7198232704271));
#24698=CARTESIAN_POINT('Ctrl Pts',(-29.9464657716568,32.0017741341583,46.7459252805377));
#24699=CARTESIAN_POINT('Origin',(-32.,32.,39.4540747194623));
#24700=CARTESIAN_POINT('',(-29.9427892494762,31.998771523558,45.3459252805377));
#24701=CARTESIAN_POINT('',(-29.9474011894601,32.0014721641163,45.4040747194623));
#24702=CARTESIAN_POINT('',(-29.94525,32.0000000000002,39.4540747194623));
#24703=CARTESIAN_POINT('Ctrl Pts',(-29.9474011894601,32.0014721641163,45.4040747194623));
#24704=CARTESIAN_POINT('Ctrl Pts',(-29.9458114267949,32.2413915495899,45.4170518896686));
#24705=CARTESIAN_POINT('Ctrl Pts',(-30.0955923589444,33.1642375601095,45.4670723229481));
#24706=CARTESIAN_POINT('Ctrl Pts',(-31.4608924203777,34.3679897749369,45.5541360193008));
#24707=CARTESIAN_POINT('Ctrl Pts',(-33.6969732872408,33.7373238670447,45.6652658085205));
#24708=CARTESIAN_POINT('Ctrl Pts',(-34.38000260453,31.5166779965259,45.7763955977402));
#24709=CARTESIAN_POINT('Ctrl Pts',(-32.8848793482069,29.7383631821778,45.88752538696));
#24710=CARTESIAN_POINT('Ctrl Pts',(-30.6194030558709,30.0248809034601,45.9967517608674));
#24711=CARTESIAN_POINT('Ctrl Pts',(-29.9447224133088,31.3552828429994,46.0689348717014));
#24712=CARTESIAN_POINT('Ctrl Pts',(-29.9420942235994,32.000637386216,46.1040747194623));
#24713=CARTESIAN_POINT('Ctrl Pts',(-29.9427892494762,31.998771523558,45.3459252805377));
#24714=CARTESIAN_POINT('Ctrl Pts',(-29.9470895693626,32.6070006515059,45.3790140432882));
#24715=CARTESIAN_POINT('Ctrl Pts',(-30.5546547810877,33.9036143174968,45.4491460691119));
#24716=CARTESIAN_POINT('Ctrl Pts',(-32.7586800023163,34.3070366209898,45.5563213580088));
#24717=CARTESIAN_POINT('Ctrl Pts',(-34.3496925356383,32.6139693025454,45.6674511472286));
#24718=CARTESIAN_POINT('Ctrl Pts',(-33.7902919416986,30.3590039366313,45.7785809364482));
#24719=CARTESIAN_POINT('Ctrl Pts',(-31.592435577624,29.605860372051,45.889710725668));
#24720=CARTESIAN_POINT('Ctrl Pts',(-30.129085316663,30.7589475750754,45.9788255070311));
#24721=CARTESIAN_POINT('Ctrl Pts',(-29.9468705479196,31.7209144546682,46.030897025321));
#24722=CARTESIAN_POINT('Ctrl Pts',(-29.9481039578725,31.9989927018527,46.0459252805377));
#24723=CARTESIAN_POINT('Origin',(-32.,32.,39.4540747194623));
#24724=CARTESIAN_POINT('',(-29.9443798519565,32.0017900284217,44.6459252805377));
#24725=CARTESIAN_POINT('',(-29.9474073584817,31.9985307398231,44.7040747194623));
#24726=CARTESIAN_POINT('',(-29.94525,32.0000000000002,39.4540747194623));
#24727=CARTESIAN_POINT('Ctrl Pts',(-29.9474073584817,31.9985307398231,44.7040747194623));
#24728=CARTESIAN_POINT('Ctrl Pts',(-29.9503473261682,32.443182900618,44.7281256445624));
#24729=CARTESIAN_POINT('Ctrl Pts',(-30.3107091275678,33.5770299650323,44.7892198327357));
#24730=CARTESIAN_POINT('Ctrl Pts',(-32.1803845625496,34.421874060765,44.8873572839825));
#24731=CARTESIAN_POINT('Ctrl Pts',(-34.1324988240748,33.1620935082564,44.9984870732021));
#24732=CARTESIAN_POINT('Ctrl Pts',(-34.1329732877935,30.8387775793711,45.109616862422));
#24733=CARTESIAN_POINT('Ctrl Pts',(-32.1813737296557,29.5781998169125,45.2207466516415));
#24734=CARTESIAN_POINT('Ctrl Pts',(-30.311064361793,30.4224106561746,45.3188992706551));
#24735=CARTESIAN_POINT('Ctrl Pts',(-29.9503493958354,31.5565429445996,45.3800086265953));
#24736=CARTESIAN_POINT('Ctrl Pts',(-29.9474011894601,32.0014721641163,45.4040747194623));
#24737=CARTESIAN_POINT('Ctrl Pts',(-29.9443798519565,32.0017900284217,44.6459252805377));
#24738=CARTESIAN_POINT('Ctrl Pts',(-29.9431807315765,32.1329178683255,44.6530445351087));
#24739=CARTESIAN_POINT('Ctrl Pts',(-30.0143464509196,32.9450400966092,44.6972070527531));
#24740=CARTESIAN_POINT('Ctrl Pts',(-31.0956022868993,34.2539028579429,44.7784128334708));
#24741=CARTESIAN_POINT('Ctrl Pts',(-33.4029915943473,33.9823289088073,44.8895426226903));
#24742=CARTESIAN_POINT('Ctrl Pts',(-34.4263782094584,31.8965490397939,45.0006724119102));
#24743=CARTESIAN_POINT('Ctrl Pts',(-33.2291698002495,29.9054463676817,45.1118022011298));
#24744=CARTESIAN_POINT('Ctrl Pts',(-30.9070385196435,29.8312564653792,45.2229319903496));
#24745=CARTESIAN_POINT('Ctrl Pts',(-29.9787574033648,31.1729920942033,45.3009730168189));
#24746=CARTESIAN_POINT('Ctrl Pts',(-29.9422753101516,31.926080915543,45.3419707802149));
#24747=CARTESIAN_POINT('Ctrl Pts',(-29.9427892494762,31.998771523558,45.3459252805377));
#24748=CARTESIAN_POINT('Origin',(-32.,32.,39.4540747194623));
#24749=CARTESIAN_POINT('',(-29.9485867435952,32.0000997951286,43.9459252805377));
#24750=CARTESIAN_POINT('',(-29.9420978996548,31.9993577750107,44.0040747194623));
#24751=CARTESIAN_POINT('',(-29.94525,32.0000000000002,39.4540747194623));
#24752=CARTESIAN_POINT('Ctrl Pts',(-29.9420978996548,31.9993577750107,44.0040747194623));
#24753=CARTESIAN_POINT('Ctrl Pts',(-29.9447426065428,32.6444368300436,44.0391993994563));
#24754=CARTESIAN_POINT('Ctrl Pts',(-30.6189110400326,33.9745949612775,44.1113673425235));
#24755=CARTESIAN_POINT('Ctrl Pts',(-32.883955539011,34.2619980463476,44.2205785486641));
#24756=CARTESIAN_POINT('Ctrl Pts',(-34.3798049995887,32.4842940434725,44.3317083378838));
#24757=CARTESIAN_POINT('Ctrl Pts',(-33.6976827324532,30.2633693839683,44.4428381271035));
#24758=CARTESIAN_POINT('Ctrl Pts',(-31.4618596391792,29.6317902312781,44.5539679163232));
#24759=CARTESIAN_POINT('Ctrl Pts',(-30.0958300942565,30.8351943211461,44.6410467804429));
#24760=CARTESIAN_POINT('Ctrl Pts',(-29.9458191844862,31.7583291205725,44.6910823814892));
#24761=CARTESIAN_POINT('Ctrl Pts',(-29.9474073584817,31.9985307398231,44.7040747194623));
#24762=CARTESIAN_POINT('Ctrl Pts',(-29.9485867435952,32.0000997951286,43.9459252805377));
#24763=CARTESIAN_POINT('Ctrl Pts',(-29.9484407938114,32.3369356488425,43.9641182900026));
#24764=CARTESIAN_POINT('Ctrl Pts',(-30.1862446142337,33.3594177249809,44.0193545625408));
#24765=CARTESIAN_POINT('Ctrl Pts',(-31.7976970844419,34.4201419063721,44.1116340981524));
#24766=CARTESIAN_POINT('Ctrl Pts',(-33.9234718487822,33.4826561851773,44.2227638873721));
#24767=CARTESIAN_POINT('Ctrl Pts',(-34.2889060362689,31.1882596020868,44.3338936765918));
#24768=CARTESIAN_POINT('Ctrl Pts',(-32.5595582415307,29.6367590281872,44.4450234658115));
#24769=CARTESIAN_POINT('Ctrl Pts',(-30.4617017157523,30.2089087790966,44.5490340004602));
#24770=CARTESIAN_POINT('Ctrl Pts',(-29.9494200549846,31.4506269035521,44.6160012720355));
#24771=CARTESIAN_POINT('Ctrl Pts',(-29.9443798519565,32.0017900284217,44.6459252805377));
#24772=CARTESIAN_POINT('Origin',(-32.,32.,39.4540747194623));
#24773=CARTESIAN_POINT('',(-29.9447460822062,31.9981575528504,43.2459252805377));
#24774=CARTESIAN_POINT('',(-29.9455159804426,32.0018771150079,43.3040747194623));
#24775=CARTESIAN_POINT('',(-29.94525,32.0000000000002,39.4540747194623));
#24776=CARTESIAN_POINT('Ctrl Pts',(-29.9455159804426,32.0018771150079,43.3040747194623));
#24777=CARTESIAN_POINT('Ctrl Pts',(-29.9439847655777,32.1707431684077,43.3132298912769));
#24778=CARTESIAN_POINT('Ctrl Pts',(-30.0402482414051,33.0211453613684,43.3594283261648));
#24779=CARTESIAN_POINT('Ctrl Pts',(-31.2204650545239,34.3000734386756,43.442670024126));
#24780=CARTESIAN_POINT('Ctrl Pts',(-33.5095065207455,33.9024727649217,43.5537998133457));
#24781=CARTESIAN_POINT('Ctrl Pts',(-34.4170639891342,31.7637496473617,43.6649296025654));
#24782=CARTESIAN_POINT('Ctrl Pts',(-33.1125507066162,29.841240290916,43.7760593917852));
#24783=CARTESIAN_POINT('Ctrl Pts',(-30.7898430825224,29.8944044092436,43.8871891810048));
#24784=CARTESIAN_POINT('Ctrl Pts',(-29.9587402818909,31.2487125411017,43.9631942902306));
#24785=CARTESIAN_POINT('Ctrl Pts',(-29.9419534402637,31.9641222152855,44.0021561363831));
#24786=CARTESIAN_POINT('Ctrl Pts',(-29.9420978996548,31.9993577750107,44.0040747194623));
#24787=CARTESIAN_POINT('Ctrl Pts',(-29.9447460822062,31.9981575528504,43.2459252805377));
#24788=CARTESIAN_POINT('Ctrl Pts',(-29.9497235697248,32.5374622374985,43.2751920448966));
#24789=CARTESIAN_POINT('Ctrl Pts',(-30.4434354700877,33.7674364415726,43.3415020723286));
#24790=CARTESIAN_POINT('Ctrl Pts',(-32.5176476120498,34.372773539922,43.4448553628341));
#24791=CARTESIAN_POINT('Ctrl Pts',(-34.2741819548352,32.8521207391232,43.5559851520537));
#24792=CARTESIAN_POINT('Ctrl Pts',(-33.9494096331178,30.5516162812554,43.6671149412735));
#24793=CARTESIAN_POINT('Ctrl Pts',(-31.8405587566049,29.5766568944465,43.7782447304931));
#24794=CARTESIAN_POINT('Ctrl Pts',(-30.1989775173142,30.6160471049063,43.871181510248));
#24795=CARTESIAN_POINT('Ctrl Pts',(-29.9487379659889,31.6510953448708,43.9270750269294));
#24796=CARTESIAN_POINT('Ctrl Pts',(-29.9485867435952,32.0000997951286,43.9459252805377));
#24797=CARTESIAN_POINT('Origin',(-32.,32.,39.4540747194623));
#24798=CARTESIAN_POINT('',(-29.94252702357,32.0010548525627,42.5459252805377));
#24799=CARTESIAN_POINT('',(-29.9484731362167,31.9994876359286,42.6040747194623));
#24800=CARTESIAN_POINT('',(-29.94525,32.0000000000002,39.4540747194623));
#24801=CARTESIAN_POINT('Ctrl Pts',(-29.9484731362167,31.9994876359286,42.6040747194623));
#24802=CARTESIAN_POINT('Ctrl Pts',(-29.9493088732493,32.3739658106449,42.6243036461709));
#24803=CARTESIAN_POINT('Ctrl Pts',(-30.2266782317794,33.4353421391061,42.6815758359526));
#24804=CARTESIAN_POINT('Ctrl Pts',(-31.9306141425706,34.4275909928101,42.7758912888076));
#24805=CARTESIAN_POINT('Ctrl Pts',(-34.0018249063725,33.3750307763075,42.8870210780274));
#24806=CARTESIAN_POINT('Ctrl Pts',(-34.2409872269693,31.0640572563152,42.998150867247));
#24807=CARTESIAN_POINT('Ctrl Pts',(-32.4292223388168,29.6096484100191,43.1092806564668));
#24808=CARTESIAN_POINT('Ctrl Pts',(-30.4062574409955,30.2824591750793,43.2112552738719));
#24809=CARTESIAN_POINT('Ctrl Pts',(-29.9501803014138,31.4874845942514,43.2761866282037));
#24810=CARTESIAN_POINT('Ctrl Pts',(-29.9455159804426,32.0018771150079,43.3040747194623));
#24811=CARTESIAN_POINT('Ctrl Pts',(-29.94252702357,32.0010548525627,42.5459252805377));
#24812=CARTESIAN_POINT('Ctrl Pts',(-29.9421477088781,32.0616438365238,42.5492225367172));
#24813=CARTESIAN_POINT('Ctrl Pts',(-29.9720545786143,32.8025444028162,42.58956305597));
#24814=CARTESIAN_POINT('Ctrl Pts',(-30.8688288986318,34.1490612499125,42.6669468382959));
#24815=CARTESIAN_POINT('Ctrl Pts',(-33.1919092821327,34.1159786819058,42.7780766275156));
#24816=CARTESIAN_POINT('Ctrl Pts',(-34.4241674445136,32.1463750716222,42.8892064167354));
#24817=CARTESIAN_POINT('Ctrl Pts',(-33.4378537354262,30.0428107344064,43.0003362059551));
#24818=CARTESIAN_POINT('Ctrl Pts',(-31.1356319387654,29.7304447118329,43.1114659951747));
#24819=CARTESIAN_POINT('Ctrl Pts',(-30.0224447689381,31.0304040223966,43.1933290200357));
#24820=CARTESIAN_POINT('Ctrl Pts',(-29.943423509447,31.8548584120434,43.2381487818233));
#24821=CARTESIAN_POINT('Ctrl Pts',(-29.9447460822062,31.9981575528504,43.2459252805377));
#24822=CARTESIAN_POINT('Origin',(-32.,32.,39.4540747194623));
#24823=CARTESIAN_POINT('',(-29.9479126851747,32.0011660315207,41.8459252805377));
#24824=CARTESIAN_POINT('',(-29.9436380261218,31.9983919808556,41.9040747194623));
#24825=CARTESIAN_POINT('',(-29.94525,32.0000000000002,39.4540747194623));
#24826=CARTESIAN_POINT('Ctrl Pts',(-29.9436380261218,31.9983919808556,41.9040747194623));
#24827=CARTESIAN_POINT('Ctrl Pts',(-29.9485892245779,32.5744100804168,41.9353774010647));
#24828=CARTESIAN_POINT('Ctrl Pts',(-30.5011706211881,33.8404092621993,42.0037233457404));
#24829=CARTESIAN_POINT('Ctrl Pts',(-32.6468874612962,34.3408420864571,42.1091125534892));
#24830=CARTESIAN_POINT('Ctrl Pts',(-34.3174574817349,32.7262261309694,42.220242342709));
#24831=CARTESIAN_POINT('Ctrl Pts',(-33.8671156802116,30.446972972158,42.3313721319287));
#24832=CARTESIAN_POINT('Ctrl Pts',(-31.708009788722,29.5890347844302,42.4425019211484));
#24833=CARTESIAN_POINT('Ctrl Pts',(-30.1605085558978,30.6921088112584,42.5334027836596));
#24834=CARTESIAN_POINT('Ctrl Pts',(-29.9477784694269,31.6882204055088,42.5872603830976));
#24835=CARTESIAN_POINT('Ctrl Pts',(-29.9484731362167,31.9994876359286,42.6040747194623));
#24836=CARTESIAN_POINT('Ctrl Pts',(-29.9479126851747,32.0011660315207,41.8459252805377));
#24837=CARTESIAN_POINT('Ctrl Pts',(-29.9465311135547,32.2670233657638,41.8602962916111));
#24838=CARTESIAN_POINT('Ctrl Pts',(-30.1180449698071,33.2164556126041,41.9117105657577));
#24839=CARTESIAN_POINT('Ctrl Pts',(-31.5501372064992,34.3865418916543,42.0001681029775));
#24840=CARTESIAN_POINT('Ctrl Pts',(-33.7609665083167,33.6724274609132,42.1112978921974));
#24841=CARTESIAN_POINT('Ctrl Pts',(-34.3601920973369,31.4277075251964,42.2224276814169));
#24842=CARTESIAN_POINT('Ctrl Pts',(-32.7993885345327,29.7067525630187,42.3335574706368));
#24843=CARTESIAN_POINT('Ctrl Pts',(-30.5750127520012,30.0733388697254,42.4413900036769));
#24844=CARTESIAN_POINT('Ctrl Pts',(-29.9464091472235,31.3809525131846,42.5121792736439));
#24845=CARTESIAN_POINT('Ctrl Pts',(-29.94252702357,32.0010548525627,42.5459252805377));
#24846=CARTESIAN_POINT('Origin',(-32.,32.,39.4540747194623));
#24847=CARTESIAN_POINT('',(-29.9473238061977,31.9976393779993,41.1459252805377));
#24848=CARTESIAN_POINT('',(-29.9434322456991,32.0014925908821,41.2040747194623));
#24849=CARTESIAN_POINT('',(-29.94525,32.0000000000002,39.4540747194623));
#24850=CARTESIAN_POINT('',(-31.4698297828114,30.0148256743283,41.));
#24851=CARTESIAN_POINT('Ctrl Pts',(-31.4698297828114,30.0148256743283,41.));
#24852=CARTESIAN_POINT('Ctrl Pts',(-30.8097602092473,30.1911070339301,41.0370432630732));
#24853=CARTESIAN_POINT('Ctrl Pts',(-30.0750747235939,30.8871231756006,41.0856850232525));
#24854=CARTESIAN_POINT('Ctrl Pts',(-29.9457054452028,31.7833432379,41.1343267834317));
#24855=CARTESIAN_POINT('Ctrl Pts',(-29.9473238061977,31.9976393779993,41.1459252805377));
#24856=CARTESIAN_POINT('',(-32.5313020758336,30.0112666986537,41.));
#24857=CARTESIAN_POINT('Origin',(-32.,32.,41.));
#24858=CARTESIAN_POINT('Ctrl Pts',(-32.5313026984106,30.0112647410448,41.));
#24859=CARTESIAN_POINT('Ctrl Pts',(-31.8868328863034,29.8399813018842,41.0363148168372));
#24860=CARTESIAN_POINT('Ctrl Pts',(-30.5071217606431,30.1592363627283,41.1043397233247));
#24861=CARTESIAN_POINT('Ctrl Pts',(-29.94828636835,31.4182664903594,41.1723646298121));
#24862=CARTESIAN_POINT('Ctrl Pts',(-29.9434322456991,32.0014925908821,41.2040747194623));
#24863=CARTESIAN_POINT('Origin',(-32.,-32.,48.));
#24864=CARTESIAN_POINT('',(-30.3315194597827,-31.9993859147877,53.3285196366098));
#24865=CARTESIAN_POINT('',(-30.3351880693888,-31.9985150917772,53.5214803633902));
#24866=CARTESIAN_POINT('',(-30.334,-32.,48.));
#24867=CARTESIAN_POINT('',(-32.6750771856749,-33.5230977622534,54.));
#24868=CARTESIAN_POINT('Ctrl Pts',(-30.3351880693888,-31.9985150917772,
53.5214803633902));
#24869=CARTESIAN_POINT('Ctrl Pts',(-30.3338369362185,-31.8287716445104,
53.5328138566338));
#24870=CARTESIAN_POINT('Ctrl Pts',(-30.3577131426661,-31.6594109347466,
53.5441473498775));
#24871=CARTESIAN_POINT('Ctrl Pts',(-30.4083948376391,-31.4985170933091,
53.5554808431211));
#24872=CARTESIAN_POINT('Ctrl Pts',(-30.5740467967946,-30.9726392578427,
53.5925241061943));
#24873=CARTESIAN_POINT('Ctrl Pts',(-31.0260602491034,-30.5372124900351,
53.6295673692676));
#24874=CARTESIAN_POINT('Ctrl Pts',(-31.5578576005161,-30.3909994562276,
53.6666106323408));
#24875=CARTESIAN_POINT('Ctrl Pts',(-32.0896549519289,-30.2447864224201,
53.703653895414));
#24876=CARTESIAN_POINT('Ctrl Pts',(-32.7012362024457,-30.3877871226129,
53.7406971584873));
#24877=CARTESIAN_POINT('Ctrl Pts',(-33.1122249699019,-30.7555548361959,
53.7777404215605));
#24878=CARTESIAN_POINT('Ctrl Pts',(-33.5232137373581,-31.1233225497789,
53.8147836846338));
#24879=CARTESIAN_POINT('Ctrl Pts',(-33.7336100217538,-31.7158572767522,
53.851826947707));
#24880=CARTESIAN_POINT('Ctrl Pts',(-33.6481832146636,-32.2596853644512,
53.8888702107803));
#24881=CARTESIAN_POINT('Ctrl Pts',(-33.5627564075734,-32.8035134521501,
53.9259134738535));
#24882=CARTESIAN_POINT('Ctrl Pts',(-33.1815065089974,-33.2986349005747,
53.9629567369268));
#24883=CARTESIAN_POINT('Ctrl Pts',(-32.6750771856749,-33.5230977622534,
54.));
#24884=CARTESIAN_POINT('',(-30.334,-32.,54.));
#24885=CARTESIAN_POINT('Origin',(-32.,-32.,54.));
#24886=CARTESIAN_POINT('',(-30.334,-32.,55.));
#24887=CARTESIAN_POINT('',(-30.334,-32.,48.));
#24888=CARTESIAN_POINT('Origin',(-32.,-32.,55.));
#24889=CARTESIAN_POINT('',(-30.3853283529176,-32.4224677305593,54.));
#24890=CARTESIAN_POINT('Origin',(-32.,-32.,54.));
#24891=CARTESIAN_POINT('Ctrl Pts',(-30.3853267233299,-32.4224680762712,
54.));
#24892=CARTESIAN_POINT('Ctrl Pts',(-30.5228595190938,-32.9453624125461,
53.9636851831628));
#24893=CARTESIAN_POINT('Ctrl Pts',(-30.9381524233032,-33.3962238017523,
53.9273703663256));
#24894=CARTESIAN_POINT('Ctrl Pts',(-31.4484748430102,-33.5748624385682,
53.8910555494883));
#24895=CARTESIAN_POINT('Ctrl Pts',(-31.9690339230712,-33.7570844238332,
53.8540122864151));
#24896=CARTESIAN_POINT('Ctrl Pts',(-32.5884731882451,-33.6560529798102,
53.8169690233418));
#24897=CARTESIAN_POINT('Ctrl Pts',(-33.0238322933555,-33.3177477726804,
53.7799257602686));
#24898=CARTESIAN_POINT('Ctrl Pts',(-33.4591913984659,-32.9794425655507,
53.7428824971953));
#24899=CARTESIAN_POINT('Ctrl Pts',(-33.7104703435129,-32.4038635953142,
53.7058392341221));
#24900=CARTESIAN_POINT('Ctrl Pts',(-33.6624375968578,-31.8545189772709,
53.6687959710488));
#24901=CARTESIAN_POINT('Ctrl Pts',(-33.6144048502027,-31.3051743592277,
53.6317527079756));
#24902=CARTESIAN_POINT('Ctrl Pts',(-33.2670604118455,-30.7820640933777,
53.5947094449024));
#24903=CARTESIAN_POINT('Ctrl Pts',(-32.7794722575826,-30.5244968713596,
53.5576661818291));
#24904=CARTESIAN_POINT('Ctrl Pts',(-32.2918841033197,-30.2669296493415,
53.5206229187559));
#24905=CARTESIAN_POINT('Ctrl Pts',(-31.6640522331509,-30.2749054711554,
53.4835796556826));
#24906=CARTESIAN_POINT('Ctrl Pts',(-31.1832059423421,-30.5448068325208,
53.4465363926094));
#24907=CARTESIAN_POINT('Ctrl Pts',(-30.7023596515333,-30.8147081938862,
53.4094931295362));
#24908=CARTESIAN_POINT('Ctrl Pts',(-30.3684989400844,-31.3465350948031,
53.3724498664629));
#24909=CARTESIAN_POINT('Ctrl Pts',(-30.3344285679539,-31.8969101687342,
53.3354066033897));
#24910=CARTESIAN_POINT('Ctrl Pts',(-30.3323171492003,-31.9310181687335,
53.3331109477964));
#24911=CARTESIAN_POINT('Ctrl Pts',(-30.3313570944005,-31.9651974041764,
53.3308152922031));
#24912=CARTESIAN_POINT('Ctrl Pts',(-30.3315194597827,-31.9993859147877,
53.3285196366098));
#24913=CARTESIAN_POINT('Origin',(-32.,-32.,48.));
#24914=CARTESIAN_POINT('',(-30.3358699316178,-31.9988695644631,52.6285196366098));
#24915=CARTESIAN_POINT('',(-30.3362229116815,-32.0008964522951,52.8214803633902));
#24916=CARTESIAN_POINT('',(-30.334,-32.,48.));
#24917=CARTESIAN_POINT('Ctrl Pts',(-30.3362229116815,-32.0008964522951,
52.8214803633902));
#24918=CARTESIAN_POINT('Ctrl Pts',(-30.3378663217269,-31.664768858379,52.8438876115277));
#24919=CARTESIAN_POINT('Ctrl Pts',(-30.436643420233,-31.3277533378251,52.8662948596652));
#24920=CARTESIAN_POINT('Ctrl Pts',(-30.6259117017676,-31.0530980531767,
52.8887021078027));
#24921=CARTESIAN_POINT('Ctrl Pts',(-30.9388066499237,-30.5990428340239,
52.925745370876));
#24922=CARTESIAN_POINT('Ctrl Pts',(-31.499015022336,-30.3154188432304,52.9627886339492));
#24923=CARTESIAN_POINT('Ctrl Pts',(-32.0501928398437,-30.332002852775,52.9998318970224));
#24924=CARTESIAN_POINT('Ctrl Pts',(-32.6013706573514,-30.3485868623195,
53.0368751600957));
#24925=CARTESIAN_POINT('Ctrl Pts',(-33.1435179199545,-30.6653788722021,
53.073918423169));
#24926=CARTESIAN_POINT('Ctrl Pts',(-33.4285423983798,-31.1374324713373,
53.1109616862422));
#24927=CARTESIAN_POINT('Ctrl Pts',(-33.713566876805,-31.6094860704725,53.1480049493154));
#24928=CARTESIAN_POINT('Ctrl Pts',(-33.7414685710525,-32.2368012588603,
53.1850482123887));
#24929=CARTESIAN_POINT('Ctrl Pts',(-33.4994968073952,-32.7322905380902,
53.2220914754619));
#24930=CARTESIAN_POINT('Ctrl Pts',(-33.257525043738,-33.2277798173201,53.2591347385351));
#24931=CARTESIAN_POINT('Ctrl Pts',(-32.745679822176,-33.5914431873922,53.2961780016084));
#24932=CARTESIAN_POINT('Ctrl Pts',(-32.1981451023726,-33.6569325686885,
53.3332212646817));
#24933=CARTESIAN_POINT('Ctrl Pts',(-31.6506103825692,-33.7224219499848,
53.3702645277549));
#24934=CARTESIAN_POINT('Ctrl Pts',(-31.0673861645244,-33.4897373425053,
53.4073077908281));
#24935=CARTESIAN_POINT('Ctrl Pts',(-30.715419288503,-33.065230587203,53.4443510539014));
#24936=CARTESIAN_POINT('Ctrl Pts',(-30.4711376939722,-32.7706028988063,
53.470060823731));
#24937=CARTESIAN_POINT('Ctrl Pts',(-30.3382530840379,-32.3835742139296,
53.4957705935606));
#24938=CARTESIAN_POINT('Ctrl Pts',(-30.3351880693888,-31.9985150917772,
53.5214803633902));
#24939=CARTESIAN_POINT('Ctrl Pts',(-30.3315194597827,-31.9993859147877,
53.3285196366098));
#24940=CARTESIAN_POINT('Ctrl Pts',(-30.3339770621283,-32.5168716171368,
53.2937720291299));
#24941=CARTESIAN_POINT('Ctrl Pts',(-30.5935877940968,-33.0364823156352,
53.2590244216499));
#24942=CARTESIAN_POINT('Ctrl Pts',(-31.0099803338461,-33.3433519309553,
53.2242768141699));
#24943=CARTESIAN_POINT('Ctrl Pts',(-31.4538825046809,-33.6704953723,53.1872335510967));
#24944=CARTESIAN_POINT('Ctrl Pts',(-32.0759668791627,-33.7558590080441,
53.1501902880235));
#24945=CARTESIAN_POINT('Ctrl Pts',(-32.5915791638324,-33.5603767516504,
53.1131470249502));
#24946=CARTESIAN_POINT('Ctrl Pts',(-33.1071914485022,-33.3648944952568,
53.076103761877));
#24947=CARTESIAN_POINT('Ctrl Pts',(-33.5163316433599,-32.8885663467255,
53.0390604988037));
#24948=CARTESIAN_POINT('Ctrl Pts',(-33.6317752999571,-32.3493595803674,
53.0020172357305));
#24949=CARTESIAN_POINT('Ctrl Pts',(-33.7472189565544,-31.8101528140094,
52.9649739726572));
#24950=CARTESIAN_POINT('Ctrl Pts',(-33.5689660748913,-31.2080674298246,
52.927930709584));
#24951=CARTESIAN_POINT('Ctrl Pts',(-33.1785862852529,-30.8186133759292,
52.8908874465108));
#24952=CARTESIAN_POINT('Ctrl Pts',(-32.7882064956146,-30.4291593220338,
52.8538441834375));
#24953=CARTESIAN_POINT('Ctrl Pts',(-32.1856997980011,-30.2523365984278,
52.8168009203643));
#24954=CARTESIAN_POINT('Ctrl Pts',(-31.6467689404394,-30.3690588596417,
52.779757657291));
#24955=CARTESIAN_POINT('Ctrl Pts',(-31.1078380828777,-30.4857811208556,
52.7427143942178));
#24956=CARTESIAN_POINT('Ctrl Pts',(-30.6324830653677,-30.8960483668895,
52.7056711311446));
#24957=CARTESIAN_POINT('Ctrl Pts',(-30.4382242967739,-31.4121242602753,
52.6686278680713));
#24958=CARTESIAN_POINT('Ctrl Pts',(-30.3681137016859,-31.5983829720839,
52.6552584575841));
#24959=CARTESIAN_POINT('Ctrl Pts',(-30.3346182799052,-31.798424158668,52.641889047097));
#24960=CARTESIAN_POINT('Ctrl Pts',(-30.3358699316178,-31.9988695644631,
52.6285196366098));
#24961=CARTESIAN_POINT('Origin',(-32.,-32.,48.));
#24962=CARTESIAN_POINT('',(-30.3356164490944,-32.001249815539,51.9285196366098));
#24963=CARTESIAN_POINT('',(-30.3318747247521,-32.0009136526746,52.1214803633902));
#24964=CARTESIAN_POINT('',(-30.334,-32.,48.));
#24965=CARTESIAN_POINT('Ctrl Pts',(-30.3318747247521,-32.0009136526746,
52.1214803633902));
#24966=CARTESIAN_POINT('Ctrl Pts',(-30.335169241692,-31.5020153100613,52.1549613664216));
#24967=CARTESIAN_POINT('Ctrl Pts',(-30.5738487645137,-31.0003825576738,
52.188442369453));
#24968=CARTESIAN_POINT('Ctrl Pts',(-30.9647448300847,-30.6911882331788,
52.2219233724844));
#24969=CARTESIAN_POINT('Ctrl Pts',(-31.3972308514164,-30.3490967285641,
52.2589666355576));
#24970=CARTESIAN_POINT('Ctrl Pts',(-32.0160471392396,-30.2425716276057,
52.2960098986309));
#24971=CARTESIAN_POINT('Ctrl Pts',(-32.5380267876055,-30.4203581055947,
52.3330531617041));
#24972=CARTESIAN_POINT('Ctrl Pts',(-33.0600064359714,-30.5981445835838,
52.3700964247774));
#24973=CARTESIAN_POINT('Ctrl Pts',(-33.48514944488,-31.0602426405203,52.4071396878506));
#24974=CARTESIAN_POINT('Ctrl Pts',(-33.6189125362116,-31.5951989750851,
52.4441829509238));
#24975=CARTESIAN_POINT('Ctrl Pts',(-33.7526756275432,-32.1301553096499,
52.4812262139971));
#24976=CARTESIAN_POINT('Ctrl Pts',(-33.5950588012977,-32.7379699218431,
52.5182694770703));
#24977=CARTESIAN_POINT('Ctrl Pts',(-33.2181869446231,-33.1405096183543,
52.5553127401436));
#24978=CARTESIAN_POINT('Ctrl Pts',(-32.8413150879486,-33.5430493148655,
52.5923560032168));
#24979=CARTESIAN_POINT('Ctrl Pts',(-32.2451882008448,-33.7403140956948,
52.62939926629));
#24980=CARTESIAN_POINT('Ctrl Pts',(-31.7025901559714,-33.6420377012477,
52.6664425293633));
#24981=CARTESIAN_POINT('Ctrl Pts',(-31.159992111098,-33.5437613068006,52.7034857924365));
#24982=CARTESIAN_POINT('Ctrl Pts',(-30.6709229084549,-33.149943737077,52.7405290555098));
#24983=CARTESIAN_POINT('Ctrl Pts',(-30.4591790690833,-32.6407917284592,
52.777572318583));
#24984=CARTESIAN_POINT('Ctrl Pts',(-30.3755178109089,-32.4396227226955,
52.7922083335188));
#24985=CARTESIAN_POINT('Ctrl Pts',(-30.3351494655438,-32.2204490030893,
52.8068443484545));
#24986=CARTESIAN_POINT('Ctrl Pts',(-30.3362229116815,-32.0008964522951,
52.8214803633902));
#24987=CARTESIAN_POINT('Ctrl Pts',(-30.3358699316178,-31.9988695644631,
52.6285196366098));
#24988=CARTESIAN_POINT('Ctrl Pts',(-30.3380862909825,-32.3538078014858,
52.6048457840237));
#24989=CARTESIAN_POINT('Ctrl Pts',(-30.4492537442715,-32.7100134869809,
52.5811719314377));
#24990=CARTESIAN_POINT('Ctrl Pts',(-30.659000109678,-32.9932070252068,52.5574980788516));
#24991=CARTESIAN_POINT('Ctrl Pts',(-30.9871972108535,-33.4363293560148,
52.5204548157783));
#24992=CARTESIAN_POINT('Ctrl Pts',(-31.5567539328823,-33.7006894768929,
52.4834115527051));
#24993=CARTESIAN_POINT('Ctrl Pts',(-32.1070443434056,-33.6653175609879,
52.4463682896319));
#24994=CARTESIAN_POINT('Ctrl Pts',(-32.6573347539289,-33.6299456450829,
52.4093250265586));
#24995=CARTESIAN_POINT('Ctrl Pts',(-33.1883588529469,-33.2948416923949,
52.3722817634853));
#24996=CARTESIAN_POINT('Ctrl Pts',(-33.4571228237319,-32.8133474894917,
52.3352385004121));
#24997=CARTESIAN_POINT('Ctrl Pts',(-33.7258867945169,-32.3318532865884,
52.2981952373388));
#24998=CARTESIAN_POINT('Ctrl Pts',(-33.7323906370689,-31.7039688334699,
52.2611519742656));
#24999=CARTESIAN_POINT('Ctrl Pts',(-33.4736582628434,-31.2170106337195,
52.2241087111924));
#25000=CARTESIAN_POINT('Ctrl Pts',(-33.2149258886179,-30.7300524339691,
52.1870654481192));
#25001=CARTESIAN_POINT('Ctrl Pts',(-32.6909572976149,-30.3840204875868,
52.1500221850459));
#25002=CARTESIAN_POINT('Ctrl Pts',(-32.1415176585263,-30.3372571458491,
52.1129789219727));
#25003=CARTESIAN_POINT('Ctrl Pts',(-31.5920780194377,-30.2904938041115,
52.0759356588994));
#25004=CARTESIAN_POINT('Ctrl Pts',(-31.0171673322635,-30.5429990670185,
52.0388923958262));
#25005=CARTESIAN_POINT('Ctrl Pts',(-30.6798616189464,-30.9792278909246,
52.001849132753));
#25006=CARTESIAN_POINT('Ctrl Pts',(-30.4572889120474,-31.2670754616322,
51.9774059673719));
#25007=CARTESIAN_POINT('Ctrl Pts',(-30.3381713154789,-31.6349177435823,
51.9529628019908));
#25008=CARTESIAN_POINT('Ctrl Pts',(-30.3356164490944,-32.001249815539,51.9285196366098));
#25009=CARTESIAN_POINT('Origin',(-32.,-32.,48.));
#25010=CARTESIAN_POINT('',(-30.3313738033598,-32.0004179151157,51.2285196366098));
#25011=CARTESIAN_POINT('',(-30.3334712707803,-31.9985210140748,51.4214803633902));
#25012=CARTESIAN_POINT('',(-30.334,-32.,48.));
#25013=CARTESIAN_POINT('Ctrl Pts',(-30.3334712707803,-31.9985210140748,
51.4214803633902));
#25014=CARTESIAN_POINT('Ctrl Pts',(-30.3324380179584,-31.8863136363627,
51.4289918582422));
#25015=CARTESIAN_POINT('Ctrl Pts',(-30.342802950118,-31.7742960662403,51.4365033530942));
#25016=CARTESIAN_POINT('Ctrl Pts',(-30.3652659897465,-31.6647594964407,
51.4440148479463));
#25017=CARTESIAN_POINT('Ctrl Pts',(-30.476043445203,-31.1245751455012,51.4810581110195));
#25018=CARTESIAN_POINT('Ctrl Pts',(-30.8810483331414,-30.6447290215782,
51.5181013740928));
#25019=CARTESIAN_POINT('Ctrl Pts',(-31.394952612285,-30.4447961102396,51.555144637166));
#25020=CARTESIAN_POINT('Ctrl Pts',(-31.9088568914286,-30.244863198901,51.5921879002393));
#25021=CARTESIAN_POINT('Ctrl Pts',(-32.5316605617774,-30.3248435001467,
51.6292311633125));
#25022=CARTESIAN_POINT('Ctrl Pts',(-32.9783720419871,-30.6481384595887,
51.6662744263857));
#25023=CARTESIAN_POINT('Ctrl Pts',(-33.4250835221967,-30.9714334190306,
51.703317689459));
#25024=CARTESIAN_POINT('Ctrl Pts',(-33.6957028122672,-31.5380430366686,
51.7403609525323));
#25025=CARTESIAN_POINT('Ctrl Pts',(-33.6663959900684,-32.0886898281663,
51.7774042156055));
#25026=CARTESIAN_POINT('Ctrl Pts',(-33.6370891678696,-32.639336619664,51.8144474786788));
#25027=CARTESIAN_POINT('Ctrl Pts',(-33.3078562334017,-33.1740205850213,
51.8514907417519));
#25028=CARTESIAN_POINT('Ctrl Pts',(-32.8293523969697,-33.4480732322182,
51.8885340048252));
#25029=CARTESIAN_POINT('Ctrl Pts',(-32.3508485605377,-33.7221258794152,
51.9255772678984));
#25030=CARTESIAN_POINT('Ctrl Pts',(-31.7230738221416,-33.7355472084518,
51.9626205309717));
#25031=CARTESIAN_POINT('Ctrl Pts',(-31.2332944888314,-33.4821957091113,
51.9996637940449));
#25032=CARTESIAN_POINT('Ctrl Pts',(-30.7435151555213,-33.2288442097708,
52.0367070571182));
#25033=CARTESIAN_POINT('Ctrl Pts',(-30.3917312272969,-32.7087198820532,
52.0737503201914));
#25034=CARTESIAN_POINT('Ctrl Pts',(-30.3389171406048,-32.1598287640589,
52.1107935832647));
#25035=CARTESIAN_POINT('Ctrl Pts',(-30.3338382815881,-32.1070447289945,
52.1143558433065));
#25036=CARTESIAN_POINT('Ctrl Pts',(-30.3315241998278,-32.0539946678751,
52.1179181033483));
#25037=CARTESIAN_POINT('Ctrl Pts',(-30.3318747247521,-32.0009136526746,
52.1214803633902));
#25038=CARTESIAN_POINT('Ctrl Pts',(-30.3356164490944,-32.001249815539,51.9285196366098));
#25039=CARTESIAN_POINT('Ctrl Pts',(-30.3342994524806,-32.1900886922754,
51.9159195389176));
#25040=CARTESIAN_POINT('Ctrl Pts',(-30.363956124187,-32.3785262679839,51.9033194412254));
#25041=CARTESIAN_POINT('Ctrl Pts',(-30.4263819138854,-32.5553981981287,
51.8907193435332));
#25042=CARTESIAN_POINT('Ctrl Pts',(-30.6099086616014,-33.0753872965215,
51.8536760804599));
#25043=CARTESIAN_POINT('Ctrl Pts',(-31.0766628964935,-33.4954131084019,
51.8166328173867));
#25044=CARTESIAN_POINT('Ctrl Pts',(-31.6130604137941,-33.6232740986022,
51.7795895543135));
#25045=CARTESIAN_POINT('Ctrl Pts',(-32.1494579310947,-33.7511350888025,
51.7425462912403));
#25046=CARTESIAN_POINT('Ctrl Pts',(-32.7554987308038,-33.5868312573226,
51.705503028167));
#25047=CARTESIAN_POINT('Ctrl Pts',(-33.1538618279575,-33.2055471471265,
51.6684597650937));
#25048=CARTESIAN_POINT('Ctrl Pts',(-33.5522249251112,-32.8242630369304,
51.6314165020205));
#25049=CARTESIAN_POINT('Ctrl Pts',(-33.7429103197094,-32.2259986480181,
51.5943732389473));
#25050=CARTESIAN_POINT('Ctrl Pts',(-33.6386614097067,-31.6845165205096,
51.557329975874));
#25051=CARTESIAN_POINT('Ctrl Pts',(-33.5344124997039,-31.1430343930012,
51.5202867128008));
#25052=CARTESIAN_POINT('Ctrl Pts',(-33.1352292851002,-30.6583345268966,
51.4832434497276));
#25053=CARTESIAN_POINT('Ctrl Pts',(-32.6237758401273,-30.4522129528976,
51.4462001866543));
#25054=CARTESIAN_POINT('Ctrl Pts',(-32.1123223951544,-30.2460913788987,
51.4091569235811));
#25055=CARTESIAN_POINT('Ctrl Pts',(-31.4885987198123,-30.3185480970053,
51.3721136605078));
#25056=CARTESIAN_POINT('Ctrl Pts',(-31.0380173860832,-30.6364273058174,
51.3350703974346));
#25057=CARTESIAN_POINT('Ctrl Pts',(-30.6060019538632,-30.9412085151324,
51.2995534771597));
#25058=CARTESIAN_POINT('Ctrl Pts',(-30.3331543957474,-31.4716039545601,
51.2640365568847));
#25059=CARTESIAN_POINT('Ctrl Pts',(-30.3313738033598,-32.0004179151157,
51.2285196366098));
#25060=CARTESIAN_POINT('Origin',(-32.,-32.,48.));
#25061=CARTESIAN_POINT('',(-30.3343902432864,-31.9984850050443,50.5285196366098));
#25062=CARTESIAN_POINT('',(-30.3367088458252,-32.0000156711401,50.7214803633902));
#25063=CARTESIAN_POINT('',(-30.334,-32.,48.));
#25064=CARTESIAN_POINT('Ctrl Pts',(-30.3367088458252,-32.0000156711401,
50.7214803633902));
#25065=CARTESIAN_POINT('Ctrl Pts',(-30.336732256219,-31.7210181018388,50.7400656131361));
#25066=CARTESIAN_POINT('Ctrl Pts',(-30.4031501299701,-31.4420100581718,
50.758650862882));
#25067=CARTESIAN_POINT('Ctrl Pts',(-30.5359003021068,-31.1992793533566,
50.7772361126279));
#25068=CARTESIAN_POINT('Ctrl Pts',(-30.8004918258534,-30.7154797016245,
50.8142793757012));
#25069=CARTESIAN_POINT('Ctrl Pts',(-31.3285991827343,-30.3757976728916,
50.8513226387744));
#25070=CARTESIAN_POINT('Ctrl Pts',(-31.8785633097738,-30.3356699216755,
50.8883659018477));
#25071=CARTESIAN_POINT('Ctrl Pts',(-32.4285274368133,-30.2955421704594,
50.9254091649209));
#25072=CARTESIAN_POINT('Ctrl Pts',(-33.0003483340113,-30.5549686967602,
50.9624524279941));
#25073=CARTESIAN_POINT('Ctrl Pts',(-33.3323638593996,-30.9952373287875,
50.9994956910674));
#25074=CARTESIAN_POINT('Ctrl Pts',(-33.664379384788,-31.4355059608149,51.0365389541406));
#25075=CARTESIAN_POINT('Ctrl Pts',(-33.7565895383665,-32.0566166985689,
51.0735822172139));
#25076=CARTESIAN_POINT('Ctrl Pts',(-33.5667994538073,-32.5743526363588,
51.1106254802872));
#25077=CARTESIAN_POINT('Ctrl Pts',(-33.3770093692481,-33.0920885741487,
51.1476687433604));
#25078=CARTESIAN_POINT('Ctrl Pts',(-32.905219046551,-33.5064497119744,51.1847120064336));
#25079=CARTESIAN_POINT('Ctrl Pts',(-32.3673171792835,-33.6278266398027,
51.2217552695068));
#25080=CARTESIAN_POINT('Ctrl Pts',(-31.8294153120161,-33.7492035676309,
51.25879853258));
#25081=CARTESIAN_POINT('Ctrl Pts',(-31.2254019001782,-33.5775962854617,
51.2958417956533));
#25082=CARTESIAN_POINT('Ctrl Pts',(-30.8316702057467,-33.191531355399,51.3328850587266));
#25083=CARTESIAN_POINT('Ctrl Pts',(-30.5177779571533,-32.8837512332643,
51.3624168269478));
#25084=CARTESIAN_POINT('Ctrl Pts',(-30.3375335491216,-32.4396691925109,
51.391948595169));
#25085=CARTESIAN_POINT('Ctrl Pts',(-30.3334712707803,-31.9985210140748,
51.4214803633902));
#25086=CARTESIAN_POINT('Ctrl Pts',(-30.3313738033598,-32.0004179151157,
51.2285196366098));
#25087=CARTESIAN_POINT('Ctrl Pts',(-30.3312972822441,-32.0231437419637,
51.2269932938115));
#25088=CARTESIAN_POINT('Ctrl Pts',(-30.3317213833894,-32.0458666480444,
51.2254669510132));
#25089=CARTESIAN_POINT('Ctrl Pts',(-30.3326549881033,-32.0685686010849,
51.2239406082149));
#25090=CARTESIAN_POINT('Ctrl Pts',(-30.3553129159683,-32.6195289880228,
51.1868973451416));
#25091=CARTESIAN_POINT('Ctrl Pts',(-30.6780677638144,-33.1581480623809,
51.1498540820684));
#25092=CARTESIAN_POINT('Ctrl Pts',(-31.1532286633698,-33.4379566562543,
51.1128108189951));
#25093=CARTESIAN_POINT('Ctrl Pts',(-31.6283895629253,-33.7177652501277,
51.0757675559219));
#25094=CARTESIAN_POINT('Ctrl Pts',(-32.25595651419,-33.7387633635163,51.0387242928487));
#25095=CARTESIAN_POINT('Ctrl Pts',(-32.7487582830866,-33.4913423736006,
51.0016810297754));
#25096=CARTESIAN_POINT('Ctrl Pts',(-33.2415600519832,-33.243921383685,50.9646377667022));
#25097=CARTESIAN_POINT('Ctrl Pts',(-33.5995966385115,-32.7280812904652,
50.9275945036289));
#25098=CARTESIAN_POINT('Ctrl Pts',(-33.6590324420583,-32.1798677235672,
50.8905512405557));
#25099=CARTESIAN_POINT('Ctrl Pts',(-33.7184682456052,-31.6316541566692,
50.8535079774824));
#25100=CARTESIAN_POINT('Ctrl Pts',(-33.4793032661706,-31.0510671160931,
50.8164647144092));
#25101=CARTESIAN_POINT('Ctrl Pts',(-33.0509781015208,-30.7037800835068,
50.7794214513359));
#25102=CARTESIAN_POINT('Ctrl Pts',(-32.622652936871,-30.3564930509205,50.7423781882627));
#25103=CARTESIAN_POINT('Ctrl Pts',(-32.0051675870062,-30.2425060263241,
50.7053349251895));
#25104=CARTESIAN_POINT('Ctrl Pts',(-31.4810799998519,-30.4139788541026,
50.6682916621162));
#25105=CARTESIAN_POINT('Ctrl Pts',(-30.9569924126976,-30.5854516818812,
50.631248399043));
#25106=CARTESIAN_POINT('Ctrl Pts',(-30.5263025882539,-31.0423843620347,
50.5942051359698));
#25107=CARTESIAN_POINT('Ctrl Pts',(-30.3860918548667,-31.57568697774,50.5571618728965));
#25108=CARTESIAN_POINT('Ctrl Pts',(-30.3499543890818,-31.7131386874804,
50.5476144608009));
#25109=CARTESIAN_POINT('Ctrl Pts',(-30.3331129433613,-31.8556635190189,
50.5380670487054));
#25110=CARTESIAN_POINT('Ctrl Pts',(-30.3343902432864,-31.9984850050443,
50.5285196366098));
#25111=CARTESIAN_POINT('Origin',(-32.,-32.,48.));
#25112=CARTESIAN_POINT('',(-30.3365646054836,-32.0005076073409,49.8285196366098));
#25113=CARTESIAN_POINT('',(-30.3334137580317,-32.0014707566408,50.0214803633902));
#25114=CARTESIAN_POINT('',(-30.334,-32.,48.));
#25115=CARTESIAN_POINT('Ctrl Pts',(-30.3334137580317,-32.0014707566408,
50.0214803633902));
#25116=CARTESIAN_POINT('Ctrl Pts',(-30.337485924098,-31.5584612466466,50.05113936803));
#25117=CARTESIAN_POINT('Ctrl Pts',(-30.5194576447965,-31.1124969702324,
50.0807983726698));
#25118=CARTESIAN_POINT('Ctrl Pts',(-30.8357594969185,-30.8044726977954,
50.1104573773095));
#25119=CARTESIAN_POINT('Ctrl Pts',(-31.2308116188967,-30.419759040159,50.1475006403828));
#25120=CARTESIAN_POINT('Ctrl Pts',(-31.8354094477522,-30.2502222407132,
50.1845439034561));
#25121=CARTESIAN_POINT('Ctrl Pts',(-32.3728922952957,-30.3734414196097,
50.2215871665293));
#25122=CARTESIAN_POINT('Ctrl Pts',(-32.9103751428392,-30.4966605985061,
50.2586304296025));
#25123=CARTESIAN_POINT('Ctrl Pts',(-33.3807430090707,-30.9126357557449,
50.2956736926757));
#25124=CARTESIAN_POINT('Ctrl Pts',(-33.5687581088666,-31.4310189149042,
50.332716955749));
#25125=CARTESIAN_POINT('Ctrl Pts',(-33.7567732086625,-31.9494020740635,
50.3697602188222));
#25126=CARTESIAN_POINT('Ctrl Pts',(-33.6624355420228,-32.5701932351434,
50.4068034818955));
#25127=CARTESIAN_POINT('Ctrl Pts',(-33.3289135136764,-33.0093217289349,
50.4438467449688));
#25128=CARTESIAN_POINT('Ctrl Pts',(-32.99539148533,-33.4484502227263,50.480890008042));
#25129=CARTESIAN_POINT('Ctrl Pts',(-32.422685095277,-33.7059160492293,50.5179332711152));
#25130=CARTESIAN_POINT('Ctrl Pts',(-31.8728616822359,-33.6639042422839,
50.5549765341885));
#25131=CARTESIAN_POINT('Ctrl Pts',(-31.3230382691947,-33.6218924353386,
50.5920197972617));
#25132=CARTESIAN_POINT('Ctrl Pts',(-30.7960978331653,-33.280402994945,50.629063060335));
#25133=CARTESIAN_POINT('Ctrl Pts',(-30.5331654604567,-32.7956996373825,
50.6661063234082));
#25134=CARTESIAN_POINT('Ctrl Pts',(-30.402150834935,-32.5541803895775,50.6845643367355));
#25135=CARTESIAN_POINT('Ctrl Pts',(-30.3366855957013,-32.2771031960785,
50.7030223500629));
#25136=CARTESIAN_POINT('Ctrl Pts',(-30.3367088458252,-32.0000156711401,
50.7214803633902));
#25137=CARTESIAN_POINT('Ctrl Pts',(-30.3343902432864,-31.9984850050443,
50.5285196366098));
#25138=CARTESIAN_POINT('Ctrl Pts',(-30.3380687739757,-32.4098004753368,
50.5010237856321));
#25139=CARTESIAN_POINT('Ctrl Pts',(-30.4920238221381,-32.8235763920677,
50.4735279346544));
#25140=CARTESIAN_POINT('Ctrl Pts',(-30.7681349422019,-33.1257217778669,
50.4460320836768));
#25141=CARTESIAN_POINT('Ctrl Pts',(-31.140120405255,-33.5327814110317,50.4089888206035));
#25142=CARTESIAN_POINT('Ctrl Pts',(-31.733822973692,-33.7372281261045,50.3719455575303));
#25143=CARTESIAN_POINT('Ctrl Pts',(-32.2775675714139,-33.6455082148342,
50.3349022944571));
#25144=CARTESIAN_POINT('Ctrl Pts',(-32.8213121691358,-33.553788303564,50.2978590313838));
#25145=CARTESIAN_POINT('Ctrl Pts',(-33.3150987961427,-33.1659017659506,
50.2608157683106));
#25146=CARTESIAN_POINT('Ctrl Pts',(-33.5329733693628,-32.6593433783788,
50.2237725052373));
#25147=CARTESIAN_POINT('Ctrl Pts',(-33.7508479425829,-32.1527849908071,
50.1867292421641));
#25148=CARTESIAN_POINT('Ctrl Pts',(-33.6928104620162,-31.5275547532769,
50.1496859790908));
#25149=CARTESIAN_POINT('Ctrl Pts',(-33.3854185640749,-31.0697546323123,
50.1126427160176));
#25150=CARTESIAN_POINT('Ctrl Pts',(-33.0780266661335,-30.6119545113477,
50.0755994529444));
#25151=CARTESIAN_POINT('Ctrl Pts',(-32.5212803508175,-30.3215845069488,
50.0385561898711));
#25152=CARTESIAN_POINT('Ctrl Pts',(-31.9699437131843,-30.3315163586626,
50.0015129267979));
#25153=CARTESIAN_POINT('Ctrl Pts',(-31.418607075551,-30.3414482103765,49.9644696637246));
#25154=CARTESIAN_POINT('Ctrl Pts',(-30.8726801156006,-30.6516819182031,
49.9274264006514));
#25155=CARTESIAN_POINT('Ctrl Pts',(-30.5819760500406,-31.1202562196133,
49.8903831375781));
#25156=CARTESIAN_POINT('Ctrl Pts',(-30.4201475127281,-31.3811011915381,
49.8697619705887));
#25157=CARTESIAN_POINT('Ctrl Pts',(-30.3374100791124,-31.6910143802325,
49.8491408035992));
#25158=CARTESIAN_POINT('Ctrl Pts',(-30.3365646054836,-32.0005076073409,
49.8285196366098));
#25159=CARTESIAN_POINT('Origin',(-32.,-32.,48.));
#25160=CARTESIAN_POINT('',(-30.3325307315923,-32.0012453487269,49.1285196366098));
#25161=CARTESIAN_POINT('',(-30.3319159147668,-31.9990590791559,49.3214803633902));
#25162=CARTESIAN_POINT('',(-30.334,-32.,48.));
#25163=CARTESIAN_POINT('Ctrl Pts',(-30.3319159147668,-31.9990590791559,
49.3214803633902));
#25164=CARTESIAN_POINT('Ctrl Pts',(-30.3315442283774,-31.944078547628,49.3251698598506));
#25165=CARTESIAN_POINT('Ctrl Pts',(-30.334026958555,-31.8891319939439,49.3288593563111));
#25166=CARTESIAN_POINT('Ctrl Pts',(-30.3394745019395,-31.8344809690004,
49.3325488527715));
#25167=CARTESIAN_POINT('Ctrl Pts',(-30.3941688985489,-31.285774034079,49.3695921158447));
#25168=CARTESIAN_POINT('Ctrl Pts',(-30.7477328056741,-30.7668580248817,
49.4066353789179));
#25169=CARTESIAN_POINT('Ctrl Pts',(-31.2383772965352,-30.5151860935124,
49.4436786419912));
#25170=CARTESIAN_POINT('Ctrl Pts',(-31.7290217873962,-30.2635141621431,
49.4807219050644));
#25171=CARTESIAN_POINT('Ctrl Pts',(-32.356746861993,-30.2790863086019,49.5177651681377));
#25172=CARTESIAN_POINT('Ctrl Pts',(-32.8343089298875,-30.5547768031055,
49.554808431211));
#25173=CARTESIAN_POINT('Ctrl Pts',(-33.3118709977821,-30.8304672976092,
49.5918516942842));
#25174=CARTESIAN_POINT('Ctrl Pts',(-33.6392700589744,-31.3662761401577,
49.6288949573574));
#25175=CARTESIAN_POINT('Ctrl Pts',(-33.6666900783104,-31.9170201097035,
49.6659382204307));
#25176=CARTESIAN_POINT('Ctrl Pts',(-33.6941100976464,-32.4677640792492,
49.7029814835039));
#25177=CARTESIAN_POINT('Ctrl Pts',(-33.4215510751261,-33.0334431757922,
49.7400247465771));
#25178=CARTESIAN_POINT('Ctrl Pts',(-32.9737345415649,-33.3552057120214,
49.7770680096504));
#25179=CARTESIAN_POINT('Ctrl Pts',(-32.5259180080037,-33.6769682482507,
49.8141112727236));
#25180=CARTESIAN_POINT('Ctrl Pts',(-31.9028439634017,-33.7548142241662,
49.8511545357969));
#25181=CARTESIAN_POINT('Ctrl Pts',(-31.3896277120905,-33.5531217432913,
49.8881977988701));
#25182=CARTESIAN_POINT('Ctrl Pts',(-30.8764114607793,-33.3514292624164,
49.9252410619434));
#25183=CARTESIAN_POINT('Ctrl Pts',(-30.4730530027589,-32.870198324751,49.9622843250166));
#25184=CARTESIAN_POINT('Ctrl Pts',(-30.3641269812991,-32.3296375980049,
49.9993275880898));
#25185=CARTESIAN_POINT('Ctrl Pts',(-30.3424135082988,-32.2218814292955,
50.0067118465233));
#25186=CARTESIAN_POINT('Ctrl Pts',(-30.3323999031507,-32.1117676715239,
50.0140961049567));
#25187=CARTESIAN_POINT('Ctrl Pts',(-30.3334137580317,-32.0014707566408,
50.0214803633902));
#25188=CARTESIAN_POINT('Ctrl Pts',(-30.3365646054836,-32.0005076073409,
49.8285196366098));
#25189=CARTESIAN_POINT('Ctrl Pts',(-30.3358912949394,-32.246978988687,49.812097540526));
#25190=CARTESIAN_POINT('Ctrl Pts',(-30.3871543989708,-32.493184027659,49.7956754444422));
#25191=CARTESIAN_POINT('Ctrl Pts',(-30.4917685280704,-32.7141280479498,
49.7792533483584));
#25192=CARTESIAN_POINT('Ctrl Pts',(-30.7277462428298,-33.2125106798825,
49.7422100852852));
#25193=CARTESIAN_POINT('Ctrl Pts',(-31.2351828435182,-33.582361048754,49.7051668222119));
#25194=CARTESIAN_POINT('Ctrl Pts',(-31.7818780931209,-33.6544376311989,
49.6681235591387));
#25195=CARTESIAN_POINT('Ctrl Pts',(-32.3285733427237,-33.7265142136438,
49.6310802960654));
#25196=CARTESIAN_POINT('Ctrl Pts',(-32.9145272412408,-33.5008170096621,
49.5940370329922));
#25197=CARTESIAN_POINT('Ctrl Pts',(-33.2716104619136,-33.0806238360038,
49.5569937699189));
#25198=CARTESIAN_POINT('Ctrl Pts',(-33.6286936825864,-32.6604306623454,
49.5199505068457));
#25199=CARTESIAN_POINT('Ctrl Pts',(-33.7569062254148,-32.0457415190103,
49.4829072437725));
#25200=CARTESIAN_POINT('Ctrl Pts',(-33.5975787260042,-31.5178348249755,
49.4458639806993));
#25201=CARTESIAN_POINT('Ctrl Pts',(-33.4382512265936,-30.9899281309408,
49.408820717626));
#25202=CARTESIAN_POINT('Ctrl Pts',(-32.9913836849439,-30.5488038862063,
49.3717774545527));
#25203=CARTESIAN_POINT('Ctrl Pts',(-32.4614602650756,-30.3963181532661,
49.3347341914795));
#25204=CARTESIAN_POINT('Ctrl Pts',(-31.9315368452074,-30.2438324203258,
49.2976909284063));
#25205=CARTESIAN_POINT('Ctrl Pts',(-31.3185575471206,-30.3799851991798,
49.260647665333));
#25206=CARTESIAN_POINT('Ctrl Pts',(-30.903018373878,-30.7424737164821,49.2236044022598));
#25207=CARTESIAN_POINT('Ctrl Pts',(-30.5474751375992,-31.0526258004598,
49.1919094803765));
#25208=CARTESIAN_POINT('Ctrl Pts',(-30.3364746524795,-31.5284746512257,
49.1602145584931));
#25209=CARTESIAN_POINT('Ctrl Pts',(-30.3325307315923,-32.0012453487269,
49.1285196366098));
#25210=CARTESIAN_POINT('Origin',(-32.,-32.,48.));
#25211=CARTESIAN_POINT('',(-30.3326865583594,-31.9986999266502,48.4285196366098));
#25212=CARTESIAN_POINT('',(-30.3362532052763,-31.9991286485791,48.6214803633902));
#25213=CARTESIAN_POINT('',(-30.334,-32.,48.));
#25214=CARTESIAN_POINT('Ctrl Pts',(-30.3362532052763,-31.9991286485791,
48.6214803633902));
#25215=CARTESIAN_POINT('Ctrl Pts',(-30.3352028054858,-31.7776576899582,
48.6362436147445));
#25216=CARTESIAN_POINT('Ctrl Pts',(-30.3763004874845,-31.5565607348184,
48.6510068660988));
#25217=CARTESIAN_POINT('Ctrl Pts',(-30.461383908182,-31.3539334389316,48.6657701174531));
#25218=CARTESIAN_POINT('Ctrl Pts',(-30.6748712667882,-30.8455104603333,
48.7028133805264));
#25219=CARTESIAN_POINT('Ctrl Pts',(-31.1652862840003,-30.4533697050991,
48.7398566435996));
#25220=CARTESIAN_POINT('Ctrl Pts',(-31.7082177071069,-30.3569526565293,
48.7768999066728));
#25221=CARTESIAN_POINT('Ctrl Pts',(-32.2511491302134,-30.2605356079596,
48.8139431697461));
#25222=CARTESIAN_POINT('Ctrl Pts',(-32.8465969592144,-30.4598422660544,
48.8509864328193));
#25223=CARTESIAN_POINT('Ctrl Pts',(-33.2220874962403,-30.8636709847649,
48.8880296958926));
#25224=CARTESIAN_POINT('Ctrl Pts',(-33.5975780332662,-31.2674997034754,
48.9250729589658));
#25225=CARTESIAN_POINT('Ctrl Pts',(-33.7531112783172,-31.8758504828017,
48.962116222039));
#25226=CARTESIAN_POINT('Ctrl Pts',(-33.6175160618016,-32.4103453047687,
48.9991594851123));
#25227=CARTESIAN_POINT('Ctrl Pts',(-33.4819208452861,-32.9448401267356,
49.0362027481855));
#25228=CARTESIAN_POINT('Ctrl Pts',(-33.0551971672042,-33.4054789913434,
49.0732460112588));
#25229=CARTESIAN_POINT('Ctrl Pts',(-32.5326114688334,-33.5814760518576,
49.110289274332));
#25230=CARTESIAN_POINT('Ctrl Pts',(-32.0100257704625,-33.7574731123719,
49.1473325374053));
#25231=CARTESIAN_POINT('Ctrl Pts',(-31.3915780518028,-33.6488283687926,
49.1843758004785));
#25232=CARTESIAN_POINT('Ctrl Pts',(-30.9602666355197,-33.3052570666801,
49.2214190635517));
#25233=CARTESIAN_POINT('Ctrl Pts',(-30.5719136902701,-32.9959053499358,
49.2547728301646));
#25234=CARTESIAN_POINT('Ctrl Pts',(-30.3352760321209,-32.4960937928359,
49.2881265967774));
#25235=CARTESIAN_POINT('Ctrl Pts',(-30.3319159147668,-31.9990590791559,
49.3214803633902));
#25236=CARTESIAN_POINT('Ctrl Pts',(-30.3325307315923,-32.0012453487269,
49.1285196366098));
#25237=CARTESIAN_POINT('Ctrl Pts',(-30.3318652169521,-32.0810227655679,
49.1231712954199));
#25238=CARTESIAN_POINT('Ctrl Pts',(-30.337095571527,-32.1607125329826,49.11782295423));
#25239=CARTESIAN_POINT('Ctrl Pts',(-30.3485221706369,-32.239503697069,49.11247461304));
#25240=CARTESIAN_POINT('Ctrl Pts',(-30.4276641890369,-32.7852209046031,
49.0754313499668));
#25241=CARTESIAN_POINT('Ctrl Pts',(-30.8040472742353,-33.2878310639205,
49.0383880868936));
#25242=CARTESIAN_POINT('Ctrl Pts',(-31.3054405672976,-33.5173424914078,
49.0013448238203));
#25243=CARTESIAN_POINT('Ctrl Pts',(-31.8068338603599,-33.7468539188952,
48.9643015607471));
#25244=CARTESIAN_POINT('Ctrl Pts',(-32.4332373612862,-33.7032666145523,
48.9272582976738));
#25245=CARTESIAN_POINT('Ctrl Pts',(-32.8980122245841,-33.4065258925043,
48.8902150346006));
#25246=CARTESIAN_POINT('Ctrl Pts',(-33.3627870878821,-33.1097851704563,
48.8531717715273));
#25247=CARTESIAN_POINT('Ctrl Pts',(-33.6659333135516,-32.5598910307031,
48.8161285084541));
#25248=CARTESIAN_POINT('Ctrl Pts',(-33.6687328324683,-32.008472049919,48.7790852453809));
#25249=CARTESIAN_POINT('Ctrl Pts',(-33.6715323513851,-31.4570530691349,
48.7420419823076));
#25250=CARTESIAN_POINT('Ctrl Pts',(-33.373985163549,-30.9041092473198,48.7049987192344));
#25251=CARTESIAN_POINT('Ctrl Pts',(-32.9122472487315,-30.6026646791234,
48.6679554561611));
#25252=CARTESIAN_POINT('Ctrl Pts',(-32.450509333914,-30.3012201109269,48.6309121930879));
#25253=CARTESIAN_POINT('Ctrl Pts',(-31.824580692115,-30.2512747963491,48.5938689300147));
#25254=CARTESIAN_POINT('Ctrl Pts',(-31.3208828758651,-30.4756834405235,
48.5568256669414));
#25255=CARTESIAN_POINT('Ctrl Pts',(-30.8171850596151,-30.7000920846979,
48.5197824038682));
#25256=CARTESIAN_POINT('Ctrl Pts',(-30.4357180689142,-31.1988546876245,
48.4827391407949));
#25257=CARTESIAN_POINT('Ctrl Pts',(-30.3510391302884,-31.7437401866318,
48.4456958777217));
#25258=CARTESIAN_POINT('Ctrl Pts',(-30.3379511376165,-31.8279577917855,
48.4399704640177));
#25259=CARTESIAN_POINT('Ctrl Pts',(-30.3319530707094,-31.913277219964,48.4342450503138));
#25260=CARTESIAN_POINT('Ctrl Pts',(-30.3326865583594,-31.9986999266502,
48.4285196366098));
#25261=CARTESIAN_POINT('Origin',(-32.,-32.,48.));
#25262=CARTESIAN_POINT('',(-30.3366116224995,-31.9995809948969,47.7285196366098));
#25263=CARTESIAN_POINT('',(-30.3350930889229,-32.0014151418723,47.9214803633902));
#25264=CARTESIAN_POINT('',(-30.334,-32.,48.));
#25265=CARTESIAN_POINT('Ctrl Pts',(-30.3350930889229,-32.0014151418723,
47.9214803633902));
#25266=CARTESIAN_POINT('Ctrl Pts',(-30.3382178115278,-31.6145003654984,
47.9473173696384));
#25267=CARTESIAN_POINT('Ctrl Pts',(-30.4725789758866,-31.2256285393869,
47.9731543758866));
#25268=CARTESIAN_POINT('Ctrl Pts',(-30.719095189131,-30.9304092629306,47.9989913821348));
#25269=CARTESIAN_POINT('Ctrl Pts',(-31.0725326133941,-30.5071448484311,
48.036034645208));
#25270=CARTESIAN_POINT('Ctrl Pts',(-31.6565135579398,-30.2763906124344,
48.0730779082813));
#25271=CARTESIAN_POINT('Ctrl Pts',(-32.2038115090487,-30.3437384421199,
48.1101211713545));
#25272=CARTESIAN_POINT('Ctrl Pts',(-32.7511094601577,-30.4110862718055,
48.1471644344278));
#25273=CARTESIAN_POINT('Ctrl Pts',(-33.2617244178299,-30.7765361671732,
48.184207697501));
#25274=CARTESIAN_POINT('Ctrl Pts',(-33.5020017461289,-31.2728602376724,
48.2212509605742));
#25275=CARTESIAN_POINT('Ctrl Pts',(-33.7422790744279,-31.7691843081716,
48.2582942236475));
#25276=CARTESIAN_POINT('Ctrl Pts',(-33.7122187733536,-32.3963825538023,
48.2953374867207));
#25277=CARTESIAN_POINT('Ctrl Pts',(-33.4255762736826,-32.8674524582047,
48.3323807497939));
#25278=CARTESIAN_POINT('Ctrl Pts',(-33.1389337740115,-33.3385223626072,
48.3694240128672));
#25279=CARTESIAN_POINT('Ctrl Pts',(-32.5957090757435,-33.6534639257813,
48.4064672759404));
#25280=CARTESIAN_POINT('Ctrl Pts',(-32.0444788552928,-33.6681615961183,
48.4435105390136));
#25281=CARTESIAN_POINT('Ctrl Pts',(-31.4932486348422,-33.6828592664552,
48.4805538020869));
#25282=CARTESIAN_POINT('Ctrl Pts',(-30.9340128922089,-33.3973130439549,
48.5175970651602));
#25283=CARTESIAN_POINT('Ctrl Pts',(-30.6226748708923,-32.9421873317236,
48.5546403282334));
#25284=CARTESIAN_POINT('Ctrl Pts',(-30.4354177507577,-32.6684477807004,
48.5769203399523));
#25285=CARTESIAN_POINT('Ctrl Pts',(-30.3378384197443,-32.3333623099221,
48.5992003516713));
#25286=CARTESIAN_POINT('Ctrl Pts',(-30.3362532052763,-31.9991286485791,
48.6214803633902));
#25287=CARTESIAN_POINT('Ctrl Pts',(-30.3326865583594,-31.9986999266502,
48.4285196366098));
#25288=CARTESIAN_POINT('Ctrl Pts',(-30.3366987148472,-32.4659596914531,
48.3972017872405));
#25289=CARTESIAN_POINT('Ctrl Pts',(-30.5421229378924,-32.9363096098717,
48.3658839378713));
#25290=CARTESIAN_POINT('Ctrl Pts',(-30.8903064904358,-33.2463231349127,
48.334566088502));
#25291=CARTESIAN_POINT('Ctrl Pts',(-31.3021436757596,-33.6130121890985,
48.2975228254287));
#25292=CARTESIAN_POINT('Ctrl Pts',(-31.913708932958,-33.7553819023824,48.2604795623555));
#25293=CARTESIAN_POINT('Ctrl Pts',(-32.4451533164113,-33.6082846659331,
48.2234362992822));
#25294=CARTESIAN_POINT('Ctrl Pts',(-32.9765976998647,-33.4611874294839,
48.186393036209));
#25295=CARTESIAN_POINT('Ctrl Pts',(-33.4279212095732,-33.0246232433016,
48.1493497731358));
#25296=CARTESIAN_POINT('Ctrl Pts',(-33.5926006546939,-32.4983615118125,
48.1123065100625));
#25297=CARTESIAN_POINT('Ctrl Pts',(-33.7572800998147,-31.9720997803234,
48.0752632469893));
#25298=CARTESIAN_POINT('Ctrl Pts',(-33.6353154803478,-31.3561405035276,
48.038219983916));
#25299=CARTESIAN_POINT('Ctrl Pts',(-33.2825171448356,-30.9323433065866,
48.0011767208428));
#25300=CARTESIAN_POINT('Ctrl Pts',(-32.9297188093234,-30.5085461096457,
47.9641334577695));
#25301=CARTESIAN_POINT('Ctrl Pts',(-32.346086757766,-30.2769109925596,47.9270901946963));
#25302=CARTESIAN_POINT('Ctrl Pts',(-31.798687852343,-30.343432928918,47.8900469316231));
#25303=CARTESIAN_POINT('Ctrl Pts',(-31.2512889469199,-30.4099548652763,
47.8530036685498));
#25304=CARTESIAN_POINT('Ctrl Pts',(-30.7401231876313,-30.774633855079,47.8159604054766));
#25305=CARTESIAN_POINT('Ctrl Pts',(-30.4990972542467,-31.2705947699818,
47.7789171424033));
#25306=CARTESIAN_POINT('Ctrl Pts',(-30.3897916759726,-31.4955136981799,
47.7621179738055));
#25307=CARTESIAN_POINT('Ctrl Pts',(-30.33604398485,-31.7474325193236,47.7453188052077));
#25308=CARTESIAN_POINT('Ctrl Pts',(-30.3366116224995,-31.9995809948969,
47.7285196366098));
#25309=CARTESIAN_POINT('Origin',(-32.,-32.,48.));
#25310=CARTESIAN_POINT('',(-30.3342224410882,-32.0015218249211,47.0285196366098));
#25311=CARTESIAN_POINT('',(-30.3312461696345,-32.0000368502823,47.2214803633902));
#25312=CARTESIAN_POINT('',(-30.334,-32.,48.));
#25313=CARTESIAN_POINT('Ctrl Pts',(-30.3312465621464,-32.0000368450299,
47.2214803633902));
#25314=CARTESIAN_POINT('Ctrl Pts',(-30.3314253521056,-31.4505822201728,
47.2583911245323));
#25315=CARTESIAN_POINT('Ctrl Pts',(-30.6293231084363,-30.9009614593998,
47.2953018856743));
#25316=CARTESIAN_POINT('Ctrl Pts',(-31.089862141057,-30.601289680795,47.3322126468164));
#25317=CARTESIAN_POINT('Ctrl Pts',(-31.5520544127147,-30.3005421430306,
47.3692559098896));
#25318=CARTESIAN_POINT('Ctrl Pts',(-32.1780577530503,-30.2515413378172,
47.4062991729629));
#25319=CARTESIAN_POINT('Ctrl Pts',(-32.681416427888,-30.4767097679246,47.4433424360361));
#25320=CARTESIAN_POINT('Ctrl Pts',(-33.1847751027257,-30.701878198032,47.4803856991094));
#25321=CARTESIAN_POINT('Ctrl Pts',(-33.5654891120655,-31.2012158634602,
47.5174289621826));
#25322=CARTESIAN_POINT('Ctrl Pts',(-33.6493457895693,-31.7462285560549,
47.5544722252559));
#25323=CARTESIAN_POINT('Ctrl Pts',(-33.7332024670731,-32.2912412486497,
47.5915154883291));
#25324=CARTESIAN_POINT('Ctrl Pts',(-33.5202018127409,-32.8819289684111,
47.6285587514023));
#25325=CARTESIAN_POINT('Ctrl Pts',(-33.1078117710471,-33.2479962176471,
47.6656020144756));
#25326=CARTESIAN_POINT('Ctrl Pts',(-32.6954217293533,-33.6140634668831,
47.7026452775488));
#25327=CARTESIAN_POINT('Ctrl Pts',(-32.083642300298,-33.7555102455937,47.739688540622));
#25328=CARTESIAN_POINT('Ctrl Pts',(-31.552420433381,-33.6076112748041,47.7767318036953));
#25329=CARTESIAN_POINT('Ctrl Pts',(-31.021198566464,-33.4597123040145,47.8137750667685));
#25330=CARTESIAN_POINT('Ctrl Pts',(-30.5705342616853,-33.0224675837247,
47.8508183298418));
#25331=CARTESIAN_POINT('Ctrl Pts',(-30.4066490612863,-32.4959579270787,
47.887861592915));
#25332=CARTESIAN_POINT('Ctrl Pts',(-30.357070825107,-32.3366792366031,47.8990678497401));
#25333=CARTESIAN_POINT('Ctrl Pts',(-30.3337378063611,-32.1692312700957,
47.9102741065651));
#25334=CARTESIAN_POINT('Ctrl Pts',(-30.3350930889229,-32.0014151418723,
47.9214803633902));
#25335=CARTESIAN_POINT('Ctrl Pts',(-30.3366116224995,-31.9995809948969,
47.7285196366098));
#25336=CARTESIAN_POINT('Ctrl Pts',(-30.3372956629111,-32.303436363191,47.7082755421344));
#25337=CARTESIAN_POINT('Ctrl Pts',(-30.4168554613542,-32.6076252315785,
47.688031447659));
#25338=CARTESIAN_POINT('Ctrl Pts',(-30.5731165724514,-32.8653003674879,
47.6677873531836));
#25339=CARTESIAN_POINT('Ctrl Pts',(-30.8590479315214,-33.3368022100883,
47.6307440901104));
#25340=CARTESIAN_POINT('Ctrl Pts',(-31.4017967571419,-33.6525630552862,
47.5937008270371));
#25341=CARTESIAN_POINT('Ctrl Pts',(-31.9530041296421,-33.6680924524609,
47.5566575639639));
#25342=CARTESIAN_POINT('Ctrl Pts',(-32.5042115021423,-33.6836218496355,
47.5196143008906));
#25343=CARTESIAN_POINT('Ctrl Pts',(-33.0638774215221,-33.398919798787,47.4825710378174));
#25344=CARTESIAN_POINT('Ctrl Pts',(-33.3759017977354,-32.944264414651,47.4455277747442));
#25345=CARTESIAN_POINT('Ctrl Pts',(-33.6879261739487,-32.489609030515,47.4084845116709));
#25346=CARTESIAN_POINT('Ctrl Pts',(-33.7523090069954,-31.8650003130914,
47.3714412485976));
#25347=CARTESIAN_POINT('Ctrl Pts',(-33.5395890615749,-31.3562558246737,
47.3343979855244));
#25348=CARTESIAN_POINT('Ctrl Pts',(-33.3268691161543,-30.8475113362559,
47.2973547224511));
#25349=CARTESIAN_POINT('Ctrl Pts',(-32.8370463922665,-30.454631076844,47.2603114593779));
#25350=CARTESIAN_POINT('Ctrl Pts',(-32.2942611124092,-30.3573949228402,
47.2232681963047));
#25351=CARTESIAN_POINT('Ctrl Pts',(-31.751475832552,-30.2601587688364,47.1862249332315));
#25352=CARTESIAN_POINT('Ctrl Pts',(-31.1557279967253,-30.4585667202408,
47.1491816701582));
#25353=CARTESIAN_POINT('Ctrl Pts',(-30.7796285842955,-30.861828374313,47.112138407085));
#25354=CARTESIAN_POINT('Ctrl Pts',(-30.4966354222943,-31.165259559867,47.0842654835932));
#25355=CARTESIAN_POINT('Ctrl Pts',(-30.3380005280478,-31.5846726915372,
47.0563925601015));
#25356=CARTESIAN_POINT('Ctrl Pts',(-30.3342224410882,-32.0015218249211,
47.0285196366098));
#25357=CARTESIAN_POINT('Origin',(-32.,-32.,48.));
#25358=CARTESIAN_POINT('',(-30.3314412753146,-31.9994832045548,46.3285196366098));
#25359=CARTESIAN_POINT('',(-30.3349857214592,-31.9985615244857,46.5214803633902));
#25360=CARTESIAN_POINT('',(-30.334,-32.,48.));
#25361=CARTESIAN_POINT('Ctrl Pts',(-30.3349857214592,-31.9985615244857,
46.5214803633902));
#25362=CARTESIAN_POINT('Ctrl Pts',(-30.3336343248108,-31.8347406191154,
46.5324216163529));
#25363=CARTESIAN_POINT('Ctrl Pts',(-30.3558556414528,-31.6712783220273,
46.5433628693156));
#25364=CARTESIAN_POINT('Ctrl Pts',(-30.4031505005406,-31.5154247680614,
46.5543041222783));
#25365=CARTESIAN_POINT('Ctrl Pts',(-30.5632743833515,-30.987759040915,46.5913473853516));
#25366=CARTESIAN_POINT('Ctrl Pts',(-31.010807058637,-30.547309536914,46.6283906484248));
#25367=CARTESIAN_POINT('Ctrl Pts',(-31.5409600008313,-30.3956235608514,
46.665433911498));
#25368=CARTESIAN_POINT('Ctrl Pts',(-32.0711129430257,-30.2439375847887,
46.7024771745713));
#25369=CARTESIAN_POINT('Ctrl Pts',(-32.6838861521289,-30.3810151366644,
46.7395204376445));
#25370=CARTESIAN_POINT('Ctrl Pts',(-33.0988779302797,-30.7441302720122,
46.7765637007178));
#25371=CARTESIAN_POINT('Ctrl Pts',(-33.5138697084305,-31.10724540736,46.813606963791));
#25372=CARTESIAN_POINT('Ctrl Pts',(-33.7310800556289,-31.6963981261798,
46.8506502268642));
#25373=CARTESIAN_POINT('Ctrl Pts',(-33.651114694771,-32.2419953388874,46.8876934899375));
#25374=CARTESIAN_POINT('Ctrl Pts',(-33.5711493339131,-32.7875925515949,
46.9247367530107));
#25375=CARTESIAN_POINT('Ctrl Pts',(-33.1940082649989,-33.2896342581902,
46.961780016084));
#25376=CARTESIAN_POINT('Ctrl Pts',(-32.6922691962012,-33.518388895943,46.9988232791572));
#25377=CARTESIAN_POINT('Ctrl Pts',(-32.1905301274034,-33.7471435336958,
47.0358665422305));
#25378=CARTESIAN_POINT('Ctrl Pts',(-31.5641930587222,-33.7026111026061,
47.0729098053037));
#25379=CARTESIAN_POINT('Ctrl Pts',(-31.0998664366148,-33.4051694016735,
47.109953068377));
#25380=CARTESIAN_POINT('Ctrl Pts',(-30.6355398145073,-33.1077277007409,
47.1469963314502));
#25381=CARTESIAN_POINT('Ctrl Pts',(-30.3332236389736,-32.5573767299654,
47.1840395945234));
#25382=CARTESIAN_POINT('Ctrl Pts',(-30.3312561526966,-32.00595410942,47.2210828575967));
#25383=CARTESIAN_POINT('Ctrl Pts',(-30.3312491150949,-32.0039816978112,
47.2212153595279));
#25384=CARTESIAN_POINT('Ctrl Pts',(-30.3312459203277,-32.002009272491,47.221347861459));
#25385=CARTESIAN_POINT('Ctrl Pts',(-30.3312465621464,-32.0000368450299,
47.2214803633902));
#25386=CARTESIAN_POINT('Ctrl Pts',(-30.3342224410882,-32.0015218249211,
47.0285196366098));
#25387=CARTESIAN_POINT('Ctrl Pts',(-30.332979430451,-32.1386673994973,47.0193492970283));
#25388=CARTESIAN_POINT('Ctrl Pts',(-30.3484988156394,-32.2755354353916,
47.0101789574467));
#25389=CARTESIAN_POINT('Ctrl Pts',(-30.3818667414576,-32.4079041546572,
47.0010086178652));
#25390=CARTESIAN_POINT('Ctrl Pts',(-30.5166553000827,-32.9426029241892,
46.963965354792));
#25391=CARTESIAN_POINT('Ctrl Pts',(-30.9426834063659,-33.4038851065129,
46.9269220917188));
#25392=CARTESIAN_POINT('Ctrl Pts',(-31.4650029089132,-33.5806704761956,
46.8898788286455));
#25393=CARTESIAN_POINT('Ctrl Pts',(-31.9873224114606,-33.7574558458782,
46.8528355655723));
#25394=CARTESIAN_POINT('Ctrl Pts',(-32.6059333102722,-33.6497444029199,
46.815792302499));
#25395=CARTESIAN_POINT('Ctrl Pts',(-33.0377626123296,-33.3068243195772,
46.7787490394258));
#25396=CARTESIAN_POINT('Ctrl Pts',(-33.4695919143871,-32.9639042362345,
46.7417057763526));
#25397=CARTESIAN_POINT('Ctrl Pts',(-33.7146396196904,-32.3857755125076,
46.7046625132793));
#25398=CARTESIAN_POINT('Ctrl Pts',(-33.6607732270088,-31.8369867176014,
46.6676192502061));
#25399=CARTESIAN_POINT('Ctrl Pts',(-33.6069068343271,-31.2881979226952,
46.6305759871328));
#25400=CARTESIAN_POINT('Ctrl Pts',(-33.2541263436604,-30.7687490566096,
46.5935327240596));
#25401=CARTESIAN_POINT('Ctrl Pts',(-32.7638621946652,-30.5163371038714,
46.5564894609864));
#25402=CARTESIAN_POINT('Ctrl Pts',(-32.27359804567,-30.2639251511331,46.5194461979131));
#25403=CARTESIAN_POINT('Ctrl Pts',(-31.6458502383462,-30.2785501117421,
46.4824029348399));
#25404=CARTESIAN_POINT('Ctrl Pts',(-31.1678727655046,-30.5535196830241,
46.4453596717666));
#25405=CARTESIAN_POINT('Ctrl Pts',(-30.6898952926629,-30.8284892543062,
46.4083164086933));
#25406=CARTESIAN_POINT('Ctrl Pts',(-30.3616881543033,-31.3638034362614,
46.3712731456201));
#25407=CARTESIAN_POINT('Ctrl Pts',(-30.3334371573101,-31.9145053618474,
46.3342298825469));
#25408=CARTESIAN_POINT('Ctrl Pts',(-30.3319855200674,-31.9428023959298,
46.3323264672345));
#25409=CARTESIAN_POINT('Ctrl Pts',(-30.3313258485816,-31.9711400578387,
46.3304230519221));
#25410=CARTESIAN_POINT('Ctrl Pts',(-30.3314412753146,-31.9994832045548,
46.3285196366098));
#25411=CARTESIAN_POINT('Origin',(-32.,-32.,48.));
#25412=CARTESIAN_POINT('',(-30.3357441857247,-31.9988063630956,45.6285196366098));
#25413=CARTESIAN_POINT('',(-30.3363139698042,-32.0008167216185,45.8214803633902));
#25414=CARTESIAN_POINT('',(-30.334,-32.,48.));
#25415=CARTESIAN_POINT('Ctrl Pts',(-30.3363139698042,-32.0008167216185,
45.8214803633902));
#25416=CARTESIAN_POINT('Ctrl Pts',(-30.3377789567259,-31.6705283252898,
45.8434953712468));
#25417=CARTESIAN_POINT('Ctrl Pts',(-30.4328915698991,-31.3394622789351,
45.8655103791034));
#25418=CARTESIAN_POINT('Ctrl Pts',(-30.6159865406001,-31.0676651762742,
45.8875253869599));
#25419=CARTESIAN_POINT('Ctrl Pts',(-30.9240688820304,-30.6103293605433,
45.9245686500332));
#25420=CARTESIAN_POINT('Ctrl Pts',(-31.4812527432153,-30.3207997319075,
45.9616119131064));
#25421=CARTESIAN_POINT('Ctrl Pts',(-32.0325738104803,-30.3315634785216,
45.9986551761797));
#25422=CARTESIAN_POINT('Ctrl Pts',(-32.5838948777453,-30.3423272251357,
46.0356984392529));
#25423=CARTESIAN_POINT('Ctrl Pts',(-33.1293531510904,-30.6533843469997,
46.0727417023262));
#25424=CARTESIAN_POINT('Ctrl Pts',(-33.4193498822572,-31.1223967917855,
46.1097849653994));
#25425=CARTESIAN_POINT('Ctrl Pts',(-33.709346613424,-31.5914092365713,46.1468282284727));
#25426=CARTESIAN_POINT('Ctrl Pts',(-33.7438818024125,-32.218377004279,46.1838714915459));
#25427=CARTESIAN_POINT('Ctrl Pts',(-33.5071523340008,-32.7164030439968,
46.2209147546191));
#25428=CARTESIAN_POINT('Ctrl Pts',(-33.2704228655892,-33.2144290837145,
46.2579580176924));
#25429=CARTESIAN_POINT('Ctrl Pts',(-32.7624287397773,-33.5835133954422,
46.2950012807656));
#25430=CARTESIAN_POINT('Ctrl Pts',(-32.2156253140534,-33.6547649994097,
46.3320445438389));
#25431=CARTESIAN_POINT('Ctrl Pts',(-31.6688218883294,-33.7260166033772,
46.3690878069121));
#25432=CARTESIAN_POINT('Ctrl Pts',(-31.0832091626933,-33.4994354995844,
46.4061310699853));
#25433=CARTESIAN_POINT('Ctrl Pts',(-30.7267603450434,-33.078703972542,46.4431743330586));
#25434=CARTESIAN_POINT('Ctrl Pts',(-30.4755937395586,-32.7822414673095,
46.4692763431691));
#25435=CARTESIAN_POINT('Ctrl Pts',(-30.3382096821063,-32.3893810168113,
46.4953783532797));
#25436=CARTESIAN_POINT('Ctrl Pts',(-30.3349857214592,-31.9985615244857,
46.5214803633902));
#25437=CARTESIAN_POINT('Ctrl Pts',(-30.3314412753146,-31.9994832045548,
46.3285196366098));
#25438=CARTESIAN_POINT('Ctrl Pts',(-30.3335722226689,-32.522739403137,46.2933797888489));
#25439=CARTESIAN_POINT('Ctrl Pts',(-30.5998767445262,-33.0478649663095,
46.258239941088));
#25440=CARTESIAN_POINT('Ctrl Pts',(-31.0242217896239,-33.3537348063572,
46.2231000933272));
#25441=CARTESIAN_POINT('Ctrl Pts',(-31.471552274558,-33.6761726560644,46.1860568302539));
#25442=CARTESIAN_POINT('Ctrl Pts',(-32.0945081000531,-33.7549586862622,
46.1490135671807));
#25443=CARTESIAN_POINT('Ctrl Pts',(-32.6080280581999,-33.5540408367315,
46.1119703041074));
#25444=CARTESIAN_POINT('Ctrl Pts',(-33.1215480163468,-33.3531229872009,
46.0749270410342));
#25445=CARTESIAN_POINT('Ctrl Pts',(-33.5256321071454,-32.8725012579417,
46.0378837779609));
#25446=CARTESIAN_POINT('Ctrl Pts',(-33.6353736417011,-32.3321055462003,
46.0008405148877));
#25447=CARTESIAN_POINT('Ctrl Pts',(-33.7451151762568,-31.7917098344589,
45.9637972518145));
#25448=CARTESIAN_POINT('Ctrl Pts',(-33.5605141545695,-31.1915401402351,
45.9267539887412));
#25449=CARTESIAN_POINT('Ctrl Pts',(-33.166043003206,-30.8062308613212,45.889710725668));
#25450=CARTESIAN_POINT('Ctrl Pts',(-32.7715718518426,-30.4209215824073,
45.8526674625947));
#25451=CARTESIAN_POINT('Ctrl Pts',(-32.1672305708029,-30.2504727188033,
45.8156241995215));
#25452=CARTESIAN_POINT('Ctrl Pts',(-31.6295624533867,-30.3728807462738,
45.7785809364483));
#25453=CARTESIAN_POINT('Ctrl Pts',(-31.0918943359704,-30.4952887737443,
45.741537673375));
#25454=CARTESIAN_POINT('Ctrl Pts',(-30.6208993821775,-30.9105536922893,
45.7044944103018));
#25455=CARTESIAN_POINT('Ctrl Pts',(-30.4321023289999,-31.428652526863,45.6674511472285));
#25456=CARTESIAN_POINT('Ctrl Pts',(-30.3659620570514,-31.6101553482161,
45.6544739770223));
#25457=CARTESIAN_POINT('Ctrl Pts',(-30.3344551994185,-31.8042787086015,
45.641496806816));
#25458=CARTESIAN_POINT('Ctrl Pts',(-30.3357441857247,-31.9988063630956,
45.6285196366098));
#25459=CARTESIAN_POINT('Origin',(-32.,-32.,48.));
#25460=CARTESIAN_POINT('',(-30.3357491875936,-32.001191282378,44.9285196366098));
#25461=CARTESIAN_POINT('',(-30.3320047816524,-32.0009960539197,45.1214803633902));
#25462=CARTESIAN_POINT('',(-30.334,-32.,48.));
#25463=CARTESIAN_POINT('Ctrl Pts',(-30.3320047816524,-32.0009960539197,
45.1214803633902));
#25464=CARTESIAN_POINT('Ctrl Pts',(-30.3354914992898,-31.5078412923967,
45.1545691261407));
#25465=CARTESIAN_POINT('Ctrl Pts',(-30.5679112651413,-31.011830923742,45.1876578888911));
#25466=CARTESIAN_POINT('Ctrl Pts',(-30.9509788634419,-30.7021956486487,
45.2207466516416));
#25467=CARTESIAN_POINT('Ctrl Pts',(-31.3798275915038,-30.35555527897,45.2577899147148));
#25468=CARTESIAN_POINT('Ctrl Pts',(-31.9974842806421,-30.2425000916246,
45.2948331777881));
#25469=CARTESIAN_POINT('Ctrl Pts',(-32.5213125790108,-30.4147635273256,
45.3318764408613));
#25470=CARTESIAN_POINT('Ctrl Pts',(-33.0451408773795,-30.5870269630266,
45.3689197039346));
#25471=CARTESIAN_POINT('Ctrl Pts',(-33.4751407849788,-31.044609021774,45.4059629670078));
#25472=CARTESIAN_POINT('Ctrl Pts',(-33.6145466756685,-31.5781226346204,
45.4430062300811));
#25473=CARTESIAN_POINT('Ctrl Pts',(-33.7539525663583,-32.1116362474668,
45.4800494931543));
#25474=CARTESIAN_POINT('Ctrl Pts',(-33.6027644401386,-32.7210814144121,
45.5170927562275));
#25475=CARTESIAN_POINT('Ctrl Pts',(-33.2301651637841,-33.1275793316411,
45.5541360193008));
#25476=CARTESIAN_POINT('Ctrl Pts',(-32.8575658874295,-33.53407724887,45.591179282374));
#25477=CARTESIAN_POINT('Ctrl Pts',(-32.2635554609402,-33.7376279163826,
45.6282225454473));
#25478=CARTESIAN_POINT('Ctrl Pts',(-31.7199498345901,-33.6450876524325,
45.6652658085205));
#25479=CARTESIAN_POINT('Ctrl Pts',(-31.17634420824,-33.5525473884824,45.7023090715937));
#25480=CARTESIAN_POINT('Ctrl Pts',(-30.6831433820292,-33.1639161930697,
45.739352334667));
#25481=CARTESIAN_POINT('Ctrl Pts',(-30.4660333797617,-32.6570295939504,
45.7763955977402));
#25482=CARTESIAN_POINT('Ctrl Pts',(-30.3779530041826,-32.4513883910573,
45.7914238529569));
#25483=CARTESIAN_POINT('Ctrl Pts',(-30.3353139157731,-32.2262837460894,
45.8064521081735));
#25484=CARTESIAN_POINT('Ctrl Pts',(-30.3363139698042,-32.0008167216185,
45.8214803633902));
#25485=CARTESIAN_POINT('Ctrl Pts',(-30.3357441857247,-31.9988063630956,
45.6285196366098));
#25486=CARTESIAN_POINT('Ctrl Pts',(-30.338134603948,-32.3595568598412,45.6044535437428));
#25487=CARTESIAN_POINT('Ctrl Pts',(-30.4533148635796,-32.7216977848527,
45.5803874508758));
#25488=CARTESIAN_POINT('Ctrl Pts',(-30.6695651499702,-33.0073153188619,
45.5563213580088));
#25489=CARTESIAN_POINT('Ctrl Pts',(-31.0024241766806,-33.4469465256848,
45.5192780949355));
#25490=CARTESIAN_POINT('Ctrl Pts',(-31.5747413826638,-33.7052761887284,
45.4822348318623));
#25491=CARTESIAN_POINT('Ctrl Pts',(-32.1246275177226,-33.6640940549181,
45.4451915687891));
#25492=CARTESIAN_POINT('Ctrl Pts',(-32.6745136527815,-33.6229119211079,
45.4081483057158));
#25493=CARTESIAN_POINT('Ctrl Pts',(-33.2019687169161,-33.2822179904438,
45.3711050426426));
#25494=CARTESIAN_POINT('Ctrl Pts',(-33.4656321327844,-32.7979119582619,
45.3340617795693));
#25495=CARTESIAN_POINT('Ctrl Pts',(-33.7292955486528,-32.3136059260799,
45.2970185164961));
#25496=CARTESIAN_POINT('Ctrl Pts',(-33.7291673162548,-31.6856877923802,
45.2599752534229));
#25497=CARTESIAN_POINT('Ctrl Pts',(-33.4653061140406,-31.2014894903992,
45.2229319903496));
#25498=CARTESIAN_POINT('Ctrl Pts',(-33.2014449118263,-30.7172911884183,
45.1858887272764));
#25499=CARTESIAN_POINT('Ctrl Pts',(-32.6738507397958,-30.3768127181562,
45.1488454642031));
#25500=CARTESIAN_POINT('Ctrl Pts',(-32.1239478303099,-30.3358551814373,
45.1118022011299));
#25501=CARTESIAN_POINT('Ctrl Pts',(-31.5740449208239,-30.2948976447184,
45.0747589380567));
#25502=CARTESIAN_POINT('Ctrl Pts',(-31.0018332738826,-30.5534610415427,
45.0377156749834));
#25503=CARTESIAN_POINT('Ctrl Pts',(-30.6691538364378,-30.993228163525,45.0006724119102));
#25504=CARTESIAN_POINT('Ctrl Pts',(-30.4531564439696,-31.2787539308252,
44.9766214868101));
#25505=CARTESIAN_POINT('Ctrl Pts',(-30.338132925853,-31.6406654260182,44.9525705617099));
#25506=CARTESIAN_POINT('Ctrl Pts',(-30.3357491875936,-32.001191282378,44.9285196366098));
#25507=CARTESIAN_POINT('Origin',(-32.,-32.,48.));
#25508=CARTESIAN_POINT('',(-30.3314442558758,-32.000520718743,44.2285196366098));
#25509=CARTESIAN_POINT('',(-30.3332944489024,-31.9985486373494,44.4214803633902));
#25510=CARTESIAN_POINT('',(-30.334,-32.,48.));
#25511=CARTESIAN_POINT('Ctrl Pts',(-30.3332944489024,-31.9985486373494,
44.4214803633902));
#25512=CARTESIAN_POINT('Ctrl Pts',(-30.3323221970028,-31.8922296275463,
44.4285996179613));
#25513=CARTESIAN_POINT('Ctrl Pts',(-30.3416240090201,-31.786080088522,44.4357188725324));
#25514=CARTESIAN_POINT('Ctrl Pts',(-30.3618163562289,-31.6820442977201,
44.4428381271035));
#25515=CARTESIAN_POINT('Ctrl Pts',(-30.4668821917387,-31.1407200440053,
44.4798813901768));
#25516=CARTESIAN_POINT('Ctrl Pts',(-30.8667963414239,-30.6566230145736,
44.51692465325));
#25517=CARTESIAN_POINT('Ctrl Pts',(-31.3785602588332,-30.4512733851868,
44.5539679163232));
#25518=CARTESIAN_POINT('Ctrl Pts',(-31.8903241762424,-30.2459237557999,
44.5910111793965));
#25519=CARTESIAN_POINT('Ctrl Pts',(-32.5139378613757,-30.3193215264579,
44.6280544424697));
#25520=CARTESIAN_POINT('Ctrl Pts',(-32.9640390733202,-30.6378802752901,
44.665097705543));
#25521=CARTESIAN_POINT('Ctrl Pts',(-33.4141402852647,-30.9564390241223,
44.7021409686162));
#25522=CARTESIAN_POINT('Ctrl Pts',(-33.6907290240204,-31.5201587511287,
44.7391842316894));
#25523=CARTESIAN_POINT('Ctrl Pts',(-33.6672397824729,-32.0710843658744,
44.7762274947627));
#25524=CARTESIAN_POINT('Ctrl Pts',(-33.6437505409253,-32.6220099806201,
44.8132707578359));
#25525=CARTESIAN_POINT('Ctrl Pts',(-33.3201833190745,-33.160141483105,44.8503140209092));
#25526=CARTESIAN_POINT('Ctrl Pts',(-32.844600723169,-33.4392328156884,44.8873572839824));
#25527=CARTESIAN_POINT('Ctrl Pts',(-32.3690181272635,-33.7183241482719,
44.9244005470557));
#25528=CARTESIAN_POINT('Ctrl Pts',(-31.7414201573035,-33.738375310954,44.9614438101289));
#25529=CARTESIAN_POINT('Ctrl Pts',(-31.2489922413343,-33.4902110004143,
44.9984870732021));
#25530=CARTESIAN_POINT('Ctrl Pts',(-30.7565643253651,-33.2420466898746,
45.0355303362754));
#25531=CARTESIAN_POINT('Ctrl Pts',(-30.3993064633867,-32.7256669061132,
45.0725735993486));
#25532=CARTESIAN_POINT('Ctrl Pts',(-30.3406979158904,-32.1773642382264,
45.1096168624219));
#25533=CARTESIAN_POINT('Ctrl Pts',(-30.3344412446157,-32.1188309747596,
45.1135713627446));
#25534=CARTESIAN_POINT('Ctrl Pts',(-30.3315880774641,-32.0599339077866,
45.1175258630674));
#25535=CARTESIAN_POINT('Ctrl Pts',(-30.3320047816524,-32.0009960539197,
45.1214803633902));
#25536=CARTESIAN_POINT('Ctrl Pts',(-30.3357491875936,-32.001191282378,44.9285196366098));
#25537=CARTESIAN_POINT('Ctrl Pts',(-30.3344614893875,-32.1959477732146,
44.9155272986367));
#25538=CARTESIAN_POINT('Ctrl Pts',(-30.3660440285482,-32.3902999106566,
44.9025349606636));
#25539=CARTESIAN_POINT('Ctrl Pts',(-30.4323358190322,-32.5719878123685,
44.8895426226904));
#25540=CARTESIAN_POINT('Ctrl Pts',(-30.6213444670197,-33.0900094920897,
44.8524993596172));
#25541=CARTESIAN_POINT('Ctrl Pts',(-31.0925089909431,-33.5050820043918,
44.8154560965439));
#25542=CARTESIAN_POINT('Ctrl Pts',(-31.6302270594382,-33.6272704182821,
44.7784128334707));
#25543=CARTESIAN_POINT('Ctrl Pts',(-32.1679451279333,-33.7494588321725,
44.7413695703975));
#25544=CARTESIAN_POINT('Ctrl Pts',(-32.7722167410002,-33.5787631476509,
44.7043263073243));
#25545=CARTESIAN_POINT('Ctrl Pts',(-33.1665304850258,-33.1932927843964,
44.667283044251));
#25546=CARTESIAN_POINT('Ctrl Pts',(-33.5608442290514,-32.807822421142,44.6302397811778));
#25547=CARTESIAN_POINT('Ctrl Pts',(-33.7452001040358,-32.2075773791546,
44.5931965181045));
#25548=CARTESIAN_POINT('Ctrl Pts',(-33.6352378612141,-31.6672265349532,
44.5561532550313));
#25549=CARTESIAN_POINT('Ctrl Pts',(-33.5252756183925,-31.1268756907518,
44.519109991958));
#25550=CARTESIAN_POINT('Ctrl Pts',(-33.1209952577648,-30.6464190443362,
44.4820667288848));
#25551=CARTESIAN_POINT('Ctrl Pts',(-32.6073932802354,-30.4457109519414,
44.4450234658115));
#25552=CARTESIAN_POINT('Ctrl Pts',(-32.093791302706,-30.2450028595466,44.4079802027383));
#25553=CARTESIAN_POINT('Ctrl Pts',(-31.470867708275,-30.3240433211725,44.370936939665));
#25554=CARTESIAN_POINT('Ctrl Pts',(-31.0236689560912,-30.6466638501528,
44.3338936765918));
#25555=CARTESIAN_POINT('Ctrl Pts',(-30.5996319852359,-30.9525748822755,
44.2987689965978));
#25556=CARTESIAN_POINT('Ctrl Pts',(-30.3335885954286,-31.4774878871477,
44.2636443166038));
#25557=CARTESIAN_POINT('Ctrl Pts',(-30.3314442558758,-32.000520718743,44.2285196366098));
#25558=CARTESIAN_POINT('Origin',(-32.,-32.,48.));
#25559=CARTESIAN_POINT('',(-30.3342156502641,-31.9984780271966,43.5285196366098));
#25560=CARTESIAN_POINT('',(-30.3367054145197,-31.9999190856858,43.7214803633902));
#25561=CARTESIAN_POINT('',(-30.334,-32.,48.));
#25562=CARTESIAN_POINT('Ctrl Pts',(-30.3367054145197,-31.9999190856858,
43.7214803633902));
#25563=CARTESIAN_POINT('Ctrl Pts',(-30.3365870778148,-31.7268111441588,
43.7396733728552));
#25564=CARTESIAN_POINT('Ctrl Pts',(-30.4000931167448,-31.4537550325403,
43.7578663823202));
#25565=CARTESIAN_POINT('Ctrl Pts',(-30.5275247375743,-31.2147878752588,
43.7760593917852));
#25566=CARTESIAN_POINT('Ctrl Pts',(-30.7869915983661,-30.7282205874178,
43.8131026548584));
#25567=CARTESIAN_POINT('Ctrl Pts',(-31.3114817673872,-30.3829796228422,
43.8501459179316));
#25568=CARTESIAN_POINT('Ctrl Pts',(-31.8609913872482,-30.3370453749637,
43.8871891810049));
#25569=CARTESIAN_POINT('Ctrl Pts',(-32.4105010071092,-30.2911111270853,
43.9242324440781));
#25570=CARTESIAN_POINT('Ctrl Pts',(-32.9850300778102,-30.544483595904,43.9612757071514));
#25571=CARTESIAN_POINT('Ctrl Pts',(-33.3216772118398,-30.9812209135267,
43.9983189702246));
#25572=CARTESIAN_POINT('Ctrl Pts',(-33.6583243458694,-31.4179582311494,
44.0353622332979));
#25573=CARTESIAN_POINT('Ctrl Pts',(-33.7570895432276,-32.0380603975761,
44.0724054963711));
#25574=CARTESIAN_POINT('Ctrl Pts',(-33.5727783851417,-32.5577720238224,
44.1094487594443));
#25575=CARTESIAN_POINT('Ctrl Pts',(-33.3884672270558,-33.0774836500687,
44.1464920225176));
#25576=CARTESIAN_POINT('Ctrl Pts',(-32.9210797135258,-33.4968047361345,
44.1835352855908));
#25577=CARTESIAN_POINT('Ctrl Pts',(-32.3844898364365,-33.6238562267059,
44.2205785486641));
#25578=CARTESIAN_POINT('Ctrl Pts',(-31.8478999593472,-33.7509077172772,
44.2576218117373));
#25579=CARTESIAN_POINT('Ctrl Pts',(-31.2421077186987,-33.585689612354,44.2946650748106));
#25580=CARTESIAN_POINT('Ctrl Pts',(-30.8443203590416,-33.2038048208934,
44.3317083378838));
#25581=CARTESIAN_POINT('Ctrl Pts',(-30.5229827838695,-32.895313538041,44.3616323463859));
#25582=CARTESIAN_POINT('Ctrl Pts',(-30.3373810669353,-32.4454340410825,
44.3915563548881));
#25583=CARTESIAN_POINT('Ctrl Pts',(-30.3332944489024,-31.9985486373494,
44.4214803633902));
#25584=CARTESIAN_POINT('Ctrl Pts',(-30.3314442558758,-32.000520718743,44.2285196366098));
#25585=CARTESIAN_POINT('Ctrl Pts',(-30.3313271275893,-32.0290898598927,
44.2266010535306));
#25586=CARTESIAN_POINT('Ctrl Pts',(-30.3319973610194,-32.0576533914107,
44.2246824704513));
#25587=CARTESIAN_POINT('Ctrl Pts',(-30.3334722154628,-32.0861753163795,
44.2227638873721));
#25588=CARTESIAN_POINT('Ctrl Pts',(-30.3619481369549,-32.6368656572913,
44.1857206242989));
#25589=CARTESIAN_POINT('Ctrl Pts',(-30.6903738898756,-33.1720457427803,
44.1486773612256));
#25590=CARTESIAN_POINT('Ctrl Pts',(-31.1684636305021,-33.4468200675988,
44.1116340981523));
#25591=CARTESIAN_POINT('Ctrl Pts',(-31.6465533711285,-33.7215943924173,
44.0745908350791));
#25592=CARTESIAN_POINT('Ctrl Pts',(-32.2743070994606,-33.7359629565652,
44.0375475720059));
#25593=CARTESIAN_POINT('Ctrl Pts',(-32.7644681132684,-33.4833507830407,
44.0005043089326));
#25594=CARTESIAN_POINT('Ctrl Pts',(-33.2546291270762,-33.2307386095162,
43.9634610458594));
#25595=CARTESIAN_POINT('Ctrl Pts',(-33.6071974263597,-32.7111456983192,
43.9264177827861));
#25596=CARTESIAN_POINT('Ctrl Pts',(-33.6608396690849,-32.1623349481554,
43.8893745197129));
#25597=CARTESIAN_POINT('Ctrl Pts',(-33.7144819118102,-31.6135241979915,
43.8523312566396));
#25598=CARTESIAN_POINT('Ctrl Pts',(-33.4691980979772,-31.0354956088606,
43.8152879935664));
#25599=CARTESIAN_POINT('Ctrl Pts',(-33.0372287708073,-30.6927519290839,
43.7782447304932));
#25600=CARTESIAN_POINT('Ctrl Pts',(-32.6052594436374,-30.3500082493071,
43.7412014674199));
#25601=CARTESIAN_POINT('Ctrl Pts',(-31.9866046031307,-30.2425494788845,
43.7041582043467));
#25602=CARTESIAN_POINT('Ctrl Pts',(-31.464357349772,-30.4195481681652,43.6671149412734));
#25603=CARTESIAN_POINT('Ctrl Pts',(-30.9421100964133,-30.596546857446,43.6300716782002));
#25604=CARTESIAN_POINT('Ctrl Pts',(-30.5162704302025,-31.0580030064301,
43.593028415127));
#25605=CARTESIAN_POINT('Ctrl Pts',(-30.3817002734078,-31.5927567841279,
43.5559851520537));
#25606=CARTESIAN_POINT('Ctrl Pts',(-30.3484415158263,-31.7249201603314,
43.5468299802391));
#25607=CARTESIAN_POINT('Ctrl Pts',(-30.3329741347624,-31.8615607154642,
43.5376748084244));
#25608=CARTESIAN_POINT('Ctrl Pts',(-30.3342156502641,-31.9984780271966,
43.5285196366098));
#25609=CARTESIAN_POINT('Origin',(-32.,-32.,48.));
#25610=CARTESIAN_POINT('',(-30.3366133246983,-32.0004154269571,42.8285196366098));
#25611=CARTESIAN_POINT('',(-30.3335913899458,-32.0014938639798,43.0214803633902));
#25612=CARTESIAN_POINT('',(-30.334,-32.,48.));
#25613=CARTESIAN_POINT('Ctrl Pts',(-30.3335913899458,-32.0014938639798,
43.0214803633902));
#25614=CARTESIAN_POINT('Ctrl Pts',(-30.3376271579769,-31.5642233339688,
43.050747127749));
#25615=CARTESIAN_POINT('Ctrl Pts',(-30.5143062321943,-31.1240664255995,
43.0800138921079));
#25616=CARTESIAN_POINT('Ctrl Pts',(-30.8231972488936,-30.8168361220973,
43.1092806564668));
#25617=CARTESIAN_POINT('Ctrl Pts',(-31.2141639800378,-30.4279713737721,
43.14632391954));
#25618=CARTESIAN_POINT('Ctrl Pts',(-31.816937431779,-30.2520582524214,43.1833671826133));
#25619=CARTESIAN_POINT('Ctrl Pts',(-32.355691742528,-30.3695936505264,43.2204104456865));
#25620=CARTESIAN_POINT('Ctrl Pts',(-32.8944460532771,-30.4871290486314,
43.2574537087598));
#25621=CARTESIAN_POINT('Ctrl Pts',(-33.3691812230342,-30.8981129661922,
43.294496971833));
#25622=CARTESIAN_POINT('Ctrl Pts',(-33.5626610114924,-31.4144813899901,
43.3315402349062));
#25623=CARTESIAN_POINT('Ctrl Pts',(-33.7561407999506,-31.930849813788,43.3685834979795));
#25624=CARTESIAN_POINT('Ctrl Pts',(-33.6683652071101,-32.552602743823,43.4056267610527));
#25625=CARTESIAN_POINT('Ctrl Pts',(-33.3394998687003,-32.9952294111363,
43.442670024126));
#25626=CARTESIAN_POINT('Ctrl Pts',(-33.0106345302905,-33.4378560784496,
43.4797132871992));
#25627=CARTESIAN_POINT('Ctrl Pts',(-32.4406794463115,-33.7013564830411,
43.5167565502725));
#25628=CARTESIAN_POINT('Ctrl Pts',(-31.8904429725427,-33.6651542682835,
43.5537998133457));
#25629=CARTESIAN_POINT('Ctrl Pts',(-31.340206498774,-33.628952053526,43.5908430764189));
#25630=CARTESIAN_POINT('Ctrl Pts',(-30.8096886352155,-33.2930472194193,
43.6278863394922));
#25631=CARTESIAN_POINT('Ctrl Pts',(-30.5416514797176,-32.8111479968127,
43.6649296025654));
#25632=CARTESIAN_POINT('Ctrl Pts',(-30.405255062707,-32.5659233106992,43.6837798561737));
#25633=CARTESIAN_POINT('Ctrl Pts',(-30.3368280262791,-32.2828933769994,
43.7026301097819));
#25634=CARTESIAN_POINT('Ctrl Pts',(-30.3367054145197,-31.9999190856858,
43.7214803633902));
#25635=CARTESIAN_POINT('Ctrl Pts',(-30.3342156502641,-31.9984780271966,
43.5285196366098));
#25636=CARTESIAN_POINT('Ctrl Pts',(-30.3379975014744,-32.4155496629652,
43.5006315453512));
#25637=CARTESIAN_POINT('Ctrl Pts',(-30.4968224208937,-32.8351893433793,
43.4727434540926));
#25638=CARTESIAN_POINT('Ctrl Pts',(-30.7800935571206,-33.1386699755361,
43.444855362834));
#25639=CARTESIAN_POINT('Ctrl Pts',(-31.156357645007,-33.5417779828347,43.4078120997607));
#25640=CARTESIAN_POINT('Ctrl Pts',(-31.7521864681585,-33.7399425910204,
43.3707688366875));
#25641=CARTESIAN_POINT('Ctrl Pts',(-32.2949319879635,-33.6424847524125,
43.3337255736143));
#25642=CARTESIAN_POINT('Ctrl Pts',(-32.8376775077686,-33.5450269138045,
43.296682310541));
#25643=CARTESIAN_POINT('Ctrl Pts',(-33.3273397242272,-33.151946628403,43.2596390474678));
#25644=CARTESIAN_POINT('Ctrl Pts',(-33.5398518619426,-32.6431152984257,
43.2225957843945));
#25645=CARTESIAN_POINT('Ctrl Pts',(-33.7523639996579,-32.1342839684484,
43.1855525213213));
#25646=CARTESIAN_POINT('Ctrl Pts',(-33.6877260586298,-31.5097015938952,
43.1485092582481));
#25647=CARTESIAN_POINT('Ctrl Pts',(-33.37551601064,-31.0551736925882,43.1114659951748));
#25648=CARTESIAN_POINT('Ctrl Pts',(-33.0633059626503,-30.6006457912812,
43.0744227321016));
#25649=CARTESIAN_POINT('Ctrl Pts',(-32.5035238076987,-30.3161723632205,
43.0373794690283));
#25650=CARTESIAN_POINT('Ctrl Pts',(-31.9523228237046,-30.3319268870294,
43.0003362059551));
#25651=CARTESIAN_POINT('Ctrl Pts',(-31.4011218397105,-30.3476814108382,
42.9632929428818));
#25652=CARTESIAN_POINT('Ctrl Pts',(-30.8585020266738,-30.6636638865167,
42.9262496798086));
#25653=CARTESIAN_POINT('Ctrl Pts',(-30.5727632705769,-31.1352824852655,
42.8892064167354));
#25654=CARTESIAN_POINT('Ctrl Pts',(-30.4167244155916,-31.3928283188926,
42.8689774900268));
#25655=CARTESIAN_POINT('Ctrl Pts',(-30.3372909438258,-31.6967869359013,
42.8487485633183));
#25656=CARTESIAN_POINT('Ctrl Pts',(-30.3366133246983,-32.0004154269571,
42.8285196366098));
#25657=CARTESIAN_POINT('Origin',(-32.,-32.,48.));
#25658=CARTESIAN_POINT('',(-30.3326929969897,-32.0013037885424,42.1285196366098));
#25659=CARTESIAN_POINT('',(-30.3317921677919,-31.9991447210974,42.3214803633902));
#25660=CARTESIAN_POINT('',(-30.334,-32.,48.));
#25661=CARTESIAN_POINT('Ctrl Pts',(-30.3317921677919,-31.9991447210974,
42.3214803633902));
#25662=CARTESIAN_POINT('Ctrl Pts',(-30.3314846178305,-31.9500189154433,
42.3247776195697));
#25663=CARTESIAN_POINT('Ctrl Pts',(-30.3334665928779,-31.9009182758191,
42.3280748757492));
#25664=CARTESIAN_POINT('Ctrl Pts',(-30.3378188581809,-31.8520286465018,
42.3313721319287));
#25665=CARTESIAN_POINT('Ctrl Pts',(-30.3867146975717,-31.3027745692444,
42.368415395002));
#25666=CARTESIAN_POINT('Ctrl Pts',(-30.7347781808911,-30.7801532877911,
42.4054586580752));
#25667=CARTESIAN_POINT('Ctrl Pts',(-31.2227371636538,-30.5233132282111,
42.4425019211484));
#25668=CARTESIAN_POINT('Ctrl Pts',(-31.7106961464166,-30.266473168631,42.4795451842217));
#25669=CARTESIAN_POINT('Ctrl Pts',(-32.3385506286227,-30.2754143309243,
42.5165884472949));
#25670=CARTESIAN_POINT('Ctrl Pts',(-32.8189978954459,-30.5460454081846,
42.5536317103682));
#25671=CARTESIAN_POINT('Ctrl Pts',(-33.2994451622691,-30.8166764854448,
42.5906749734414));
#25672=CARTESIAN_POINT('Ctrl Pts',(-33.6324852137093,-31.348997477672,42.6277182365146));
#25673=CARTESIAN_POINT('Ctrl Pts',(-33.6657206816788,-31.8994211243615,
42.6647614995879));
#25674=CARTESIAN_POINT('Ctrl Pts',(-33.6989561496482,-32.4498447710511,
42.7018047626611));
#25675=CARTESIAN_POINT('Ctrl Pts',(-33.4323870341469,-33.018371072203,42.7388480257344));
#25676=CARTESIAN_POINT('Ctrl Pts',(-32.987993940445,-33.3448455058512,42.7758912888076));
#25677=CARTESIAN_POINT('Ctrl Pts',(-32.5436008467431,-33.6713199394994,
42.8129345518808));
#25678=CARTESIAN_POINT('Ctrl Pts',(-31.9213837748406,-33.7557425056438,
42.8499778149541));
#25679=CARTESIAN_POINT('Ctrl Pts',(-31.4060658711755,-33.559481880255,42.8870210780273));
#25680=CARTESIAN_POINT('Ctrl Pts',(-30.8907479675104,-33.3632212548662,
42.9240643411006));
#25681=CARTESIAN_POINT('Ctrl Pts',(-30.4823292320827,-32.8862774379442,
42.9611076041738));
#25682=CARTESIAN_POINT('Ctrl Pts',(-30.3676998696425,-32.3468973418332,
42.9981508672471));
#25683=CARTESIAN_POINT('Ctrl Pts',(-30.3436357074793,-32.2336651836491,
43.0059273659614));
#25684=CARTESIAN_POINT('Ctrl Pts',(-30.3325190423327,-32.1176814162753,
43.0137038646758));
#25685=CARTESIAN_POINT('Ctrl Pts',(-30.3335913899458,-32.0014938639798,
43.0214803633902));
#25686=CARTESIAN_POINT('Ctrl Pts',(-30.3366133246983,-32.0004154269571,
42.8285196366098));
#25687=CARTESIAN_POINT('Ctrl Pts',(-30.3360500859214,-32.2527922164965,
42.8117053002451));
#25688=CARTESIAN_POINT('Ctrl Pts',(-30.3898990887803,-32.5049409227568,
42.7948909638803));
#25689=CARTESIAN_POINT('Ctrl Pts',(-30.4993952962616,-32.7300182145042,
42.7780766275156));
#25690=CARTESIAN_POINT('Ctrl Pts',(-30.7406237772002,-33.2258806231749,
42.7410333644424));
#25691=CARTESIAN_POINT('Ctrl Pts',(-31.2519384382344,-33.5903507186974,
42.7039901013692));
#25692=CARTESIAN_POINT('Ctrl Pts',(-31.7993644698996,-33.6566491133687,
42.6669468382959));
#25693=CARTESIAN_POINT('Ctrl Pts',(-32.3467905015648,-33.7229475080399,
42.6299035752227));
#25694=CARTESIAN_POINT('Ctrl Pts',(-32.9303279038609,-33.4910742018599,
42.5928603121494));
#25695=CARTESIAN_POINT('Ctrl Pts',(-33.2829531118668,-33.0671328620635,
42.5558170490762));
#25696=CARTESIAN_POINT('Ctrl Pts',(-33.6355783198726,-32.6431915222671,
42.5187737860029));
#25697=CARTESIAN_POINT('Ctrl Pts',(-33.7572913335882,-32.0271821488543,
42.4817305229297));
#25698=CARTESIAN_POINT('Ctrl Pts',(-33.5923969650778,-31.5009878855554,
42.4446872598564));
#25699=CARTESIAN_POINT('Ctrl Pts',(-33.4275025965674,-30.9747936222564,
42.4076439967832));
#25700=CARTESIAN_POINT('Ctrl Pts',(-32.9760008458309,-30.5384144690715,
42.3706007337099));
#25701=CARTESIAN_POINT('Ctrl Pts',(-32.4444964120379,-30.3915339832607,
42.3335574706367));
#25702=CARTESIAN_POINT('Ctrl Pts',(-31.9129919782449,-30.24465349745,42.2965142075635));
#25703=CARTESIAN_POINT('Ctrl Pts',(-31.3014848613954,-30.3872716790136,
42.2594709444902));
#25704=CARTESIAN_POINT('Ctrl Pts',(-30.8897975089001,-30.7541295513978,
42.222427681417));
#25705=CARTESIAN_POINT('Ctrl Pts',(-30.5419092008583,-31.0641355881196,
42.1911249998146));
#25706=CARTESIAN_POINT('Ctrl Pts',(-30.3367074496864,-31.5342658723109,
42.1598223182122));
#25707=CARTESIAN_POINT('Ctrl Pts',(-30.3326929969897,-32.0013037885424,
42.1285196366098));
#25708=CARTESIAN_POINT('Origin',(-32.,-32.,48.));
#25709=CARTESIAN_POINT('',(-30.3325261502749,-31.9987897978733,41.4285196366098));
#25710=CARTESIAN_POINT('',(-30.336158884875,-31.9990545752999,41.6214803633902));
#25711=CARTESIAN_POINT('',(-30.334,-32.,48.));
#25712=CARTESIAN_POINT('',(-33.2690708798524,-30.9206413469515,41.));
#25713=CARTESIAN_POINT('Ctrl Pts',(-30.3325261502749,-31.9987897978733,
41.4285196366098));
#25714=CARTESIAN_POINT('Ctrl Pts',(-30.3364618898858,-32.4716719965804,
41.3968095469596));
#25715=CARTESIAN_POINT('Ctrl Pts',(-30.547679155389,-32.9475346897789,41.3650994573094));
#25716=CARTESIAN_POINT('Ctrl Pts',(-30.903524458539,-33.2578207687041,41.3333893676592));
#25717=CARTESIAN_POINT('Ctrl Pts',(-31.3192177386076,-33.6202924291878,
41.2963461045859));
#25718=CARTESIAN_POINT('Ctrl Pts',(-31.9322786939314,-33.7568087910484,
41.2593028415127));
#25719=CARTESIAN_POINT('Ctrl Pts',(-32.4621353665983,-33.6037827270274,
41.2222595784395));
#25720=CARTESIAN_POINT('Ctrl Pts',(-32.9919920392653,-33.4507566630064,
41.1852163153662));
#25721=CARTESIAN_POINT('Ctrl Pts',(-33.4386444292754,-33.0081881731037,
41.148173052293));
#25722=CARTESIAN_POINT('Ctrl Pts',(-33.5976357065192,-32.4811507187836,
41.1111297892197));
#25723=CARTESIAN_POINT('Ctrl Pts',(-33.7566269837631,-31.9541132644636,
41.0740865261465));
#25724=CARTESIAN_POINT('Ctrl Pts',(-33.6279571482407,-31.3426068457263,
41.0370432630732));
#25725=CARTESIAN_POINT('Ctrl Pts',(-33.2690708798524,-30.9206413469515,
41.));
#25726=CARTESIAN_POINT('',(-30.7285328693903,-30.9187901141545,41.));
#25727=CARTESIAN_POINT('Origin',(-32.,-32.,41.));
#25728=CARTESIAN_POINT('Ctrl Pts',(-30.7285315473809,-30.918789092831,41.));
#25729=CARTESIAN_POINT('Ctrl Pts',(-31.0793196250029,-30.5073509960358,
41.0363148168372));
#25730=CARTESIAN_POINT('Ctrl Pts',(-31.6491071295587,-30.2813272422374,
41.0726296336745));
#25731=CARTESIAN_POINT('Ctrl Pts',(-32.1864002131136,-30.3417998878807,
41.1089444505117));
#25732=CARTESIAN_POINT('Ctrl Pts',(-32.7344709670091,-30.403485566521,41.1459877135849));
#25733=CARTESIAN_POINT('Ctrl Pts',(-33.2487306007817,-30.7632767007414,
41.1830309766582));
#25734=CARTESIAN_POINT('Ctrl Pts',(-33.4941904839029,-31.2569744981691,
41.2200742397314));
#25735=CARTESIAN_POINT('Ctrl Pts',(-33.739650367024,-31.7506722955968,41.2571175028047));
#25736=CARTESIAN_POINT('Ctrl Pts',(-33.7163104994937,-32.378276756232,41.2941607658779));
#25737=CARTESIAN_POINT('Ctrl Pts',(-33.4346827711206,-32.8523785277167,
41.3312040289511));
#25738=CARTESIAN_POINT('Ctrl Pts',(-33.1530550427475,-33.3264802992015,
41.3682472920244));
#25739=CARTESIAN_POINT('Ctrl Pts',(-32.6131394535318,-33.6470793815359,
41.4052905550977));
#25740=CARTESIAN_POINT('Ctrl Pts',(-32.0620834355512,-33.6675828812401,
41.4423338181709));
#25741=CARTESIAN_POINT('Ctrl Pts',(-31.5110274175706,-33.6880863809443,
41.4793770812442));
#25742=CARTESIAN_POINT('Ctrl Pts',(-30.9488309708251,-33.4084942980185,
41.5164203443174));
#25743=CARTESIAN_POINT('Ctrl Pts',(-30.6327092175202,-32.9566901398629,
41.5534636073906));
#25744=CARTESIAN_POINT('Ctrl Pts',(-30.4392275569172,-32.6801643460085,
41.5761358593905));
#25745=CARTESIAN_POINT('Ctrl Pts',(-30.3379261292159,-32.3391274519624,
41.5988081113903));
#25746=CARTESIAN_POINT('Ctrl Pts',(-30.336158884875,-31.9990545752999,41.6214803633902));
#25747=CARTESIAN_POINT('Origin',(-32.,-32.,39.4540747194623));
#25748=CARTESIAN_POINT('',(-29.946715297465,-31.9981685983364,53.7459252805377));
#25749=CARTESIAN_POINT('',(-29.9453611647571,-32.0018310237742,53.8040747194623));
#25750=CARTESIAN_POINT('',(-29.94525,-31.9999999999998,39.4540747194623));
#25751=CARTESIAN_POINT('',(-32.3836679988468,-29.9813874990081,54.));
#25752=CARTESIAN_POINT('Ctrl Pts',(-29.9453611647571,-32.0018310237742,
53.8040747194623));
#25753=CARTESIAN_POINT('Ctrl Pts',(-29.950627974885,-31.4803614070367,53.832339883235));
#25754=CARTESIAN_POINT('Ctrl Pts',(-30.4182836665071,-30.2677806430719,
53.8976483100809));
#25755=CARTESIAN_POINT('Ctrl Pts',(-31.7124802469751,-29.853818061345,53.9629567369268));
#25756=CARTESIAN_POINT('Ctrl Pts',(-32.3836679988468,-29.9813874990081,
54.));
#25757=CARTESIAN_POINT('',(-33.3415658621448,-30.43873672012,54.));
#25758=CARTESIAN_POINT('Origin',(-32.,-32.,54.));
#25759=CARTESIAN_POINT('Ctrl Pts',(-29.946715297465,-31.9981685983364,53.7459252805377));
#25760=CARTESIAN_POINT('Ctrl Pts',(-29.9450488863716,-31.7888166485938,
53.7572587737813));
#25761=CARTESIAN_POINT('Ctrl Pts',(-30.0707451223458,-30.8972175670589,
53.8056355300982));
#25762=CARTESIAN_POINT('Ctrl Pts',(-31.3453228233254,-29.6694106382552,
53.8903271032523));
#25763=CARTESIAN_POINT('Ctrl Pts',(-32.8352372258873,-30.0047894254256,
53.9636851831628));
#25764=CARTESIAN_POINT('Ctrl Pts',(-33.3415672767799,-30.4387352221184,
54.));
#25765=CARTESIAN_POINT('Origin',(-32.,-32.,39.4540747194623));
#25766=CARTESIAN_POINT('',(-29.9479916133119,-32.0011056334653,53.0459252805377));
#25767=CARTESIAN_POINT('',(-29.94219064225,-31.9992426220948,53.1040747194623));
#25768=CARTESIAN_POINT('',(-29.94525,-31.9999999999998,39.4540747194623));
#25769=CARTESIAN_POINT('Ctrl Pts',(-29.94219064225,-31.9992426220948,53.1040747194623));
#25770=CARTESIAN_POINT('Ctrl Pts',(-29.9419903899876,-31.957076450319,53.1063703750556));
#25771=CARTESIAN_POINT('Ctrl Pts',(-29.9622810278528,-31.2347025931292,
53.1457092937222));
#25772=CARTESIAN_POINT('Ctrl Pts',(-30.811328806025,-29.8822030832705,53.2220914754619));
#25773=CARTESIAN_POINT('Ctrl Pts',(-33.1343255681424,-29.8526923031888,
53.3332212646816));
#25774=CARTESIAN_POINT('Ctrl Pts',(-34.4195104145668,-31.7882159864216,
53.4443510539014));
#25775=CARTESIAN_POINT('Ctrl Pts',(-33.4897707765082,-33.9178754505755,
53.555480843121));
#25776=CARTESIAN_POINT('Ctrl Pts',(-31.1978269047507,-34.2916948256168,
53.6666106323409));
#25777=CARTESIAN_POINT('Ctrl Pts',(-30.0344356552593,-33.0074711411215,
53.7494752577879));
#25778=CARTESIAN_POINT('Ctrl Pts',(-29.9437254911529,-32.1637799201182,
53.7952966201617));
#25779=CARTESIAN_POINT('Ctrl Pts',(-29.9453611647571,-32.0018310237742,
53.8040747194623));
#25780=CARTESIAN_POINT('Ctrl Pts',(-29.9479916133119,-32.0011056334653,
53.0459252805377));
#25781=CARTESIAN_POINT('Ctrl Pts',(-29.9500185021419,-31.5865449050144,
53.0683325286752));
#25782=CARTESIAN_POINT('Ctrl Pts',(-30.2732452755414,-30.4837342237769,
53.127783039886));
#25783=CARTESIAN_POINT('Ctrl Pts',(-32.0730427793273,-29.5725272947448,
53.2242768141699));
#25784=CARTESIAN_POINT('Ctrl Pts',(-34.0790039218848,-30.7446672388737,
53.3354066033898));
#25785=CARTESIAN_POINT('Ctrl Pts',(-34.1822410279863,-33.0657522628949,
53.4465363926093));
#25786=CARTESIAN_POINT('Ctrl Pts',(-32.2883983467057,-34.4113176464284,
53.5576661818292));
#25787=CARTESIAN_POINT('Ctrl Pts',(-30.3505279516326,-33.6381799778053,
53.6574624778052));
#25788=CARTESIAN_POINT('Ctrl Pts',(-29.9504955128613,-32.4730787011233,
53.7202155107081));
#25789=CARTESIAN_POINT('Ctrl Pts',(-29.946715297465,-31.9981685983364,53.7459252805377));
#25790=CARTESIAN_POINT('Origin',(-32.,-32.,39.4540747194623));
#25791=CARTESIAN_POINT('',(-29.942628805933,-32.0011268474386,52.3459252805377));
#25792=CARTESIAN_POINT('',(-29.9475562677021,-31.9986057848623,52.4040747194623));
#25793=CARTESIAN_POINT('',(-29.94525,-31.9999999999998,39.4540747194623));
#25794=CARTESIAN_POINT('Ctrl Pts',(-29.9475562677021,-31.9986057848623,
52.4040747194624));
#25795=CARTESIAN_POINT('Ctrl Pts',(-29.9460125514017,-31.7513877791255,
52.4174441299495));
#25796=CARTESIAN_POINT('Ctrl Pts',(-30.1017872484456,-30.8210709304397,
52.46785680351));
#25797=CARTESIAN_POINT('Ctrl Pts',(-31.4859339874079,-29.6264478597178,
52.5553127401435));
#25798=CARTESIAN_POINT('Ctrl Pts',(-33.7152268510116,-30.2806972438647,
52.6664425293633));
#25799=CARTESIAN_POINT('Ctrl Pts',(-34.3747678628917,-32.5084312351377,
52.777572318583));
#25800=CARTESIAN_POINT('Ctrl Pts',(-32.8609368628007,-34.2708596802663,
52.8887021078028));
#25801=CARTESIAN_POINT('Ctrl Pts',(-30.6067538461013,-33.961536273617,52.9975362414292));
#25802=CARTESIAN_POINT('Ctrl Pts',(-29.9452217097288,-32.6374801652532,
53.0693271119824));
#25803=CARTESIAN_POINT('Ctrl Pts',(-29.94219064225,-31.9992426220948,53.1040747194623));
#25804=CARTESIAN_POINT('Ctrl Pts',(-29.942628805933,-32.0011268474386,52.3459252805377));
#25805=CARTESIAN_POINT('Ctrl Pts',(-29.9466920764506,-31.3858139005692,
52.3794062835691));
#25806=CARTESIAN_POINT('Ctrl Pts',(-30.5667600036778,-30.0826171398043,
52.4499305496737));
#25807=CARTESIAN_POINT('Ctrl Pts',(-32.7830045778855,-29.7011054025381,
52.5574980788515));
#25808=CARTESIAN_POINT('Ctrl Pts',(-34.3560464702414,-31.4108820816923,
52.6686278680714));
#25809=CARTESIAN_POINT('Ctrl Pts',(-33.7728594827364,-33.6598143885419,
52.779757657291));
#25810=CARTESIAN_POINT('Ctrl Pts',(-31.5671721094895,-34.389699997922,52.8908874465108));
#25811=CARTESIAN_POINT('Ctrl Pts',(-30.1224675495405,-33.2263676194101,
52.979609987593));
#25812=CARTESIAN_POINT('Ctrl Pts',(-29.94666768567,-32.2718893091822,53.031289265602));
#25813=CARTESIAN_POINT('Ctrl Pts',(-29.9479916133119,-32.0011056334653,
53.0459252805377));
#25814=CARTESIAN_POINT('Origin',(-32.,-32.,39.4540747194623));
#25815=CARTESIAN_POINT('',(-29.9445978953396,-31.9981759025628,51.6459252805377));
#25816=CARTESIAN_POINT('',(-29.9472436367207,-32.0015414516679,51.7040747194623));
#25817=CARTESIAN_POINT('',(-29.94525,-31.9999999999998,39.4540747194623));
#25818=CARTESIAN_POINT('Ctrl Pts',(-29.9472436367207,-32.0015414516679,
51.7040747194623));
#25819=CARTESIAN_POINT('Ctrl Pts',(-29.9503946641538,-31.549728231468,51.7285178848434));
#25820=CARTESIAN_POINT('Ctrl Pts',(-30.3199519211819,-30.4085132585972,
51.7900043132977));
#25821=CARTESIAN_POINT('Ctrl Pts',(-32.2059544087099,-29.5801662395198,
51.8885340048252));
#25822=CARTESIAN_POINT('Ctrl Pts',(-34.1446539207691,-30.8604948262468,
51.9996637940449));
#25823=CARTESIAN_POINT('Ctrl Pts',(-34.1205895081331,-33.1836861468564,
52.1107935832646));
#25824=CARTESIAN_POINT('Ctrl Pts',(-32.1557844046688,-34.4235808289435,
52.2219233724844));
#25825=CARTESIAN_POINT('Ctrl Pts',(-30.3019343102738,-33.5631151086926,
52.3196837512169));
#25826=CARTESIAN_POINT('Ctrl Pts',(-29.9502897997577,-32.4363664946596,
52.3804008668763));
#25827=CARTESIAN_POINT('Ctrl Pts',(-29.9475562677021,-31.9986057848623,
52.4040747194624));
#25828=CARTESIAN_POINT('Ctrl Pts',(-29.9445978953396,-31.9981759025628,
51.6459252805377));
#25829=CARTESIAN_POINT('Ctrl Pts',(-29.943323539856,-31.8597856808618,51.6534367753897));
#25830=CARTESIAN_POINT('Ctrl Pts',(-30.0191495440249,-31.0403066328242,
51.697991533315));
#25831=CARTESIAN_POINT('Ctrl Pts',(-31.119458497007,-29.7366705485938,51.7795895543135));
#25832=CARTESIAN_POINT('Ctrl Pts',(-33.4238507688844,-30.0326000635722,
51.8907193435332));
#25833=CARTESIAN_POINT('Ctrl Pts',(-34.4251502639725,-32.1290726539236,
52.001849132753));
#25834=CARTESIAN_POINT('Ctrl Pts',(-33.2069785255006,-34.1074193726832,
52.1129789219726));
#25835=CARTESIAN_POINT('Ctrl Pts',(-30.8841931526569,-34.1570786929198,
52.2241087111924));
#25836=CARTESIAN_POINT('Ctrl Pts',(-29.9747293436638,-32.8124059711623,
52.3017574973807));
#25837=CARTESIAN_POINT('Ctrl Pts',(-29.942196488353,-32.0665939638752,52.3423630204958));
#25838=CARTESIAN_POINT('Ctrl Pts',(-29.942628805933,-32.0011268474386,52.3459252805377));
#25839=CARTESIAN_POINT('Origin',(-32.,-32.,39.4540747194623));
#25840=CARTESIAN_POINT('',(-29.9485909369504,-32.000019327896,50.9459252805377));
#25841=CARTESIAN_POINT('',(-29.9420109978713,-32.0005154328236,51.0040747194623));
#25842=CARTESIAN_POINT('',(-29.94525,-31.9999999999998,39.4540747194623));
#25843=CARTESIAN_POINT('Ctrl Pts',(-29.9420109978713,-32.0005154328236,
51.0040747194623));
#25844=CARTESIAN_POINT('Ctrl Pts',(-29.944207079629,-31.3483062578826,51.0395916397372));
#25845=CARTESIAN_POINT('Ctrl Pts',(-30.6316982652924,-30.0118743248253,
51.1121518230855));
#25846=CARTESIAN_POINT('Ctrl Pts',(-32.9077975170184,-29.7474644773485,
51.2217552695068));
#25847=CARTESIAN_POINT('Ctrl Pts',(-34.3847873913407,-31.54086852875,51.3328850587266));
#25848=CARTESIAN_POINT('Ctrl Pts',(-33.6792457084763,-33.7544647228394,
51.4440148479463));
#25849=CARTESIAN_POINT('Ctrl Pts',(-31.4368765610531,-34.3623938304022,
51.5551446371661));
#25850=CARTESIAN_POINT('Ctrl Pts',(-30.0897291770567,-33.150114152176,51.6418312610047));
#25851=CARTESIAN_POINT('Ctrl Pts',(-29.9456193277218,-32.2344446221205,
51.6914746217701));
#25852=CARTESIAN_POINT('Ctrl Pts',(-29.9472436367207,-32.0015414516679,
51.7040747194623));
#25853=CARTESIAN_POINT('Ctrl Pts',(-29.9485909369504,-32.000019327896,50.9459252805377));
#25854=CARTESIAN_POINT('Ctrl Pts',(-29.9486198100036,-31.6559195346657,
50.9645105302836));
#25855=CARTESIAN_POINT('Ctrl Pts',(-30.1938071310638,-30.6259372284373,
51.0201390431027));
#25856=CARTESIAN_POINT('Ctrl Pts',(-31.8232699653508,-29.5778563144268,
51.1128108189952));
#25857=CARTESIAN_POINT('Ctrl Pts',(-33.9390244464751,-30.5377422476497,
51.2239406082148));
#25858=CARTESIAN_POINT('Ctrl Pts',(-34.2802047821274,-32.8358706181179,
51.3350703974346));
#25859=CARTESIAN_POINT('Ctrl Pts',(-32.5345664287748,-34.3690192638818,
51.4462001866543));
#25860=CARTESIAN_POINT('Ctrl Pts',(-30.4507580622789,-33.7769849094658,
51.549818481022));
#25861=CARTESIAN_POINT('Ctrl Pts',(-29.9496080792662,-32.5422630692145,
51.6163935123165));
#25862=CARTESIAN_POINT('Ctrl Pts',(-29.9445978953396,-31.9981759025628,
51.6459252805377));
#25863=CARTESIAN_POINT('Origin',(-32.,-32.,39.4540747194623));
#25864=CARTESIAN_POINT('',(-29.9445269623743,-32.0018139479035,50.2459252805377));
#25865=CARTESIAN_POINT('',(-29.9457313039573,-31.9981314910653,50.3040747194623));
#25866=CARTESIAN_POINT('',(-29.94525,-31.9999999999998,39.4540747194623));
#25867=CARTESIAN_POINT('Ctrl Pts',(-29.9457313039573,-31.9981314910653,
50.3040747194623));
#25868=CARTESIAN_POINT('Ctrl Pts',(-29.9441559546048,-31.8219835628476,
50.3136221315579));
#25869=CARTESIAN_POINT('Ctrl Pts',(-30.04551831087,-30.9641799638719,50.3602128067267));
#25870=CARTESIAN_POINT('Ctrl Pts',(-31.2448019668464,-29.6918213798318,
50.4438467449688));
#25871=CARTESIAN_POINT('Ctrl Pts',(-33.5295162933197,-30.1135767918179,
50.5549765341885));
#25872=CARTESIAN_POINT('Ctrl Pts',(-34.4144338950484,-32.2617662665304,
50.6661063234082));
#25873=CARTESIAN_POINT('Ctrl Pts',(-33.0896877794978,-34.1703900928393,
50.7772361126279));
#25874=CARTESIAN_POINT('Ctrl Pts',(-30.7676712252758,-34.0926964431059,
50.8883659018477));
#25875=CARTESIAN_POINT('Ctrl Pts',(-29.9551340369839,-32.736719821345,50.9639787707924));
#25876=CARTESIAN_POINT('Ctrl Pts',(-29.9419166210631,-32.0285441799519,
51.002548376664));
#25877=CARTESIAN_POINT('Ctrl Pts',(-29.9420109978713,-32.0005154328236,
51.0040747194623));
#25878=CARTESIAN_POINT('Ctrl Pts',(-29.9445269623743,-32.0018139479035,
50.2459252805377));
#25879=CARTESIAN_POINT('Ctrl Pts',(-29.9495493412608,-31.4554311203763,
50.2755842851775));
#25880=CARTESIAN_POINT('Ctrl Pts',(-30.4542942197084,-30.2184357035796,
50.3422865528905));
#25881=CARTESIAN_POINT('Ctrl Pts',(-32.5426800429829,-29.6328261767372,
50.4460320836768));
#25882=CARTESIAN_POINT('Ctrl Pts',(-34.2830552647223,-31.1719467427689,
50.5571618728965));
#25883=CARTESIAN_POINT('Ctrl Pts',(-33.9340030668927,-33.4688926699519,
50.6682916621162));
#25884=CARTESIAN_POINT('Ctrl Pts',(-31.8149722356298,-34.4215239550785,
50.7794214513359));
#25885=CARTESIAN_POINT('Ctrl Pts',(-30.1913421833166,-33.3693129648789,
50.8719659908098));
#25886=CARTESIAN_POINT('Ctrl Pts',(-29.9485622615649,-32.3417633806376,
50.9274672672104));
#25887=CARTESIAN_POINT('Ctrl Pts',(-29.9485909369504,-32.000019327896,50.9459252805377));
#25888=CARTESIAN_POINT('Origin',(-32.,-32.,39.4540747194623));
#25889=CARTESIAN_POINT('',(-29.9426796073631,-31.9988395215457,49.5459252805377));
#25890=CARTESIAN_POINT('',(-29.9484130390861,-32.0006260541318,49.6040747194623));
#25891=CARTESIAN_POINT('',(-29.94525,-31.9999999999998,39.4540747194623));
#25892=CARTESIAN_POINT('Ctrl Pts',(-29.9484130390861,-32.0006260541318,
49.6040747194623));
#25893=CARTESIAN_POINT('Ctrl Pts',(-29.949455798353,-31.6189146445274,49.6246958864518));
#25894=CARTESIAN_POINT('Ctrl Pts',(-30.2348077206026,-30.5500595899322,
49.6823603165144));
#25895=CARTESIAN_POINT('Ctrl Pts',(-31.9562582889836,-29.5718115240782,
49.7770680096504));
#25896=CARTESIAN_POINT('Ctrl Pts',(-34.0162363647259,-30.6461892549403,
49.8881977988701));
#25897=CARTESIAN_POINT('Ctrl Pts',(-34.2309767846438,-32.9595598982149,
49.9993275880899));
#25898=CARTESIAN_POINT('Ctrl Pts',(-32.4039514451918,-34.3947517286369,
50.1104573773095));
#25899=CARTESIAN_POINT('Ctrl Pts',(-30.3959590882678,-33.7032818528283,
50.2120397544337));
#25900=CARTESIAN_POINT('Ctrl Pts',(-29.9502681952741,-32.5054246858934,
50.2765788684846));
#25901=CARTESIAN_POINT('Ctrl Pts',(-29.9457313039573,-31.9981314910653,
50.3040747194623));
#25902=CARTESIAN_POINT('Ctrl Pts',(-29.9426796073631,-31.9988395215457,
49.5459252805377));
#25903=CARTESIAN_POINT('Ctrl Pts',(-29.9422211904312,-31.9310296493027,
49.5496147769981));
#25904=CARTESIAN_POINT('Ctrl Pts',(-29.9760269151363,-31.1828581065124,
49.5903475365317));
#25905=CARTESIAN_POINT('Ctrl Pts',(-30.8915902884901,-29.8391109584199,
49.6681235591387));
#25906=CARTESIAN_POINT('Ctrl Pts',(-33.2141919037862,-29.8967283676685,
49.7792533483584));
#25907=CARTESIAN_POINT('Ctrl Pts',(-34.4255782561001,-31.8792371657958,
49.8903831375781));
#25908=CARTESIAN_POINT('Ctrl Pts',(-33.417101692732,-33.9722668001683,50.0015129267978));
#25909=CARTESIAN_POINT('Ctrl Pts',(-31.1117090280035,-34.2602992473698,
50.1126427160177));
#25910=CARTESIAN_POINT('Ctrl Pts',(-30.0175818073808,-32.9549395658362,
50.1941135005975));
#25911=CARTESIAN_POINT('Ctrl Pts',(-29.9432765312118,-32.1378479130034,
50.2385410221042));
#25912=CARTESIAN_POINT('Ctrl Pts',(-29.9445269623743,-32.0018139479035,
50.2459252805377));
#25913=CARTESIAN_POINT('Origin',(-32.,-32.,39.4540747194623));
#25914=CARTESIAN_POINT('',(-29.9480289757152,-31.9989253245302,48.8459252805377));
#25915=CARTESIAN_POINT('',(-29.9434378875985,-32.001535942555,48.9040747194623));
#25916=CARTESIAN_POINT('',(-29.94525,-31.9999999999998,39.4540747194623));
#25917=CARTESIAN_POINT('Ctrl Pts',(-29.9434378875985,-32.001535942555,48.9040747194623));
#25918=CARTESIAN_POINT('Ctrl Pts',(-29.9483020961478,-31.4184473527047,
48.9357696413456));
#25919=CARTESIAN_POINT('Ctrl Pts',(-30.5126875610296,-30.1456437631745,
49.0045078263023));
#25920=CARTESIAN_POINT('Ctrl Pts',(-32.6715753574031,-29.6661192937061,
49.110289274332));
#25921=CARTESIAN_POINT('Ctrl Pts',(-34.3249986728979,-31.2982922382464,
49.2214190635518));
#25922=CARTESIAN_POINT('Ctrl Pts',(-33.8506084165172,-33.5726605166398,
49.3325488527714));
#25923=CARTESIAN_POINT('Ctrl Pts',(-31.6825614063526,-34.4077469449976,
49.4436786419912));
#25924=CARTESIAN_POINT('Ctrl Pts',(-30.1534240465415,-33.2932195029209,
49.5341872642215));
#25925=CARTESIAN_POINT('Ctrl Pts',(-29.9475826160125,-32.3046098901588,
49.5876526233785));
#25926=CARTESIAN_POINT('Ctrl Pts',(-29.9484130390861,-32.0006260541318,
49.6040747194623));
#25927=CARTESIAN_POINT('Ctrl Pts',(-29.9480289757152,-31.9989253245302,
48.8459252805377));
#25928=CARTESIAN_POINT('Ctrl Pts',(-29.946733472132,-31.725775593302,48.860688531892));
#25929=CARTESIAN_POINT('Ctrl Pts',(-30.124603871078,-30.7688699552255,48.9124950463195));
#25930=CARTESIAN_POINT('Ctrl Pts',(-31.5753614937973,-29.6088296426979,
49.0013448238204));
#25931=CARTESIAN_POINT('Ctrl Pts',(-33.7785363316839,-30.346270259241,49.11247461304));
#25932=CARTESIAN_POINT('Ctrl Pts',(-34.3540140062368,-32.5971864005746,
49.2236044022598));
#25933=CARTESIAN_POINT('Ctrl Pts',(-32.7751235905007,-34.3015640243191,
49.3347341914795));
#25934=CARTESIAN_POINT('Ctrl Pts',(-30.5628189463383,-33.9129211956171,
49.4421744842388));
#25935=CARTESIAN_POINT('Ctrl Pts',(-29.9468237857144,-32.6118539740871,
49.5125715139248));
#25936=CARTESIAN_POINT('Ctrl Pts',(-29.9426796073631,-31.9988395215457,
49.5459252805377));
#25937=CARTESIAN_POINT('Origin',(-32.,-32.,39.4540747194623));
#25938=CARTESIAN_POINT('',(-29.9465981539402,-32.0017453557993,48.1459252805377));
#25939=CARTESIAN_POINT('',(-29.9436300755036,-31.998396563196,48.2040747194623));
#25940=CARTESIAN_POINT('',(-29.94525,-31.9999999999998,39.4540747194623));
#25941=CARTESIAN_POINT('Ctrl Pts',(-29.9436300755036,-31.998396563196,48.2040747194623));
#25942=CARTESIAN_POINT('Ctrl Pts',(-29.9427254333975,-31.8930410370475,
48.2098001331663));
#25943=CARTESIAN_POINT('Ctrl Pts',(-29.9979858606748,-31.1069897759954,
48.2525688099435));
#25944=CARTESIAN_POINT('Ctrl Pts',(-31.0116628453703,-29.7816217002818,
48.3323807497939));
#25945=CARTESIAN_POINT('Ctrl Pts',(-33.3276176053999,-29.9664208631788,
48.4435105390137));
#25946=CARTESIAN_POINT('Ctrl Pts',(-34.4285511303809,-32.0123295988471,
48.5546403282334));
#25947=CARTESIAN_POINT('Ctrl Pts',(-33.3069009973776,-34.0469544193595,
48.6657701174531));
#25948=CARTESIAN_POINT('Ctrl Pts',(-30.9891892443255,-34.2082287535704,
48.7768999066729));
#25949=CARTESIAN_POINT('Ctrl Pts',(-29.9937470887763,-32.8789465406671,
48.8563347740092));
#25950=CARTESIAN_POINT('Ctrl Pts',(-29.9426170795512,-32.0999288880857,
48.8987263782724));
#25951=CARTESIAN_POINT('Ctrl Pts',(-29.9434378875985,-32.001535942555,48.9040747194623));
#25952=CARTESIAN_POINT('Ctrl Pts',(-29.9465981539402,-32.0017453557993,
48.1459252805377));
#25953=CARTESIAN_POINT('Ctrl Pts',(-29.9504520097461,-31.5245465942421,
48.1717622867859));
#25954=CARTESIAN_POINT('Ctrl Pts',(-30.3537536178561,-30.3572998412992,
48.2346425561073));
#25955=CARTESIAN_POINT('Ctrl Pts',(-32.2966122923061,-29.5895986461497,
48.334566088502));
#25956=CARTESIAN_POINT('Ctrl Pts',(-34.1859029602719,-30.9417742268944,
48.4456958777216));
#25957=CARTESIAN_POINT('Ctrl Pts',(-34.0746789441273,-33.2624265592047,
48.5568256669415));
#25958=CARTESIAN_POINT('Ctrl Pts',(-32.0647312572736,-34.4277197949768,
48.6679554561611));
#25959=CARTESIAN_POINT('Ctrl Pts',(-30.2704276366367,-33.5115469150408,
48.7643219940266));
#25960=CARTESIAN_POINT('Ctrl Pts',(-29.9499840894175,-32.4111501838608,
48.8236452688188));
#25961=CARTESIAN_POINT('Ctrl Pts',(-29.9480289757152,-31.9989253245302,
48.8459252805377));
#25962=CARTESIAN_POINT('Origin',(-32.,-32.,39.4540747194623));
#25963=CARTESIAN_POINT('',(-29.9418535816666,-32.0000454490499,47.4459252805377));
#25964=CARTESIAN_POINT('',(-29.9484710272094,-31.9994832228478,47.5040747194623));
#25965=CARTESIAN_POINT('',(-29.94525,-31.9999999999998,39.4540747194623));
#25966=CARTESIAN_POINT('Ctrl Pts',(-29.9484710272094,-31.9994832228478,
47.5040747194623));
#25967=CARTESIAN_POINT('Ctrl Pts',(-29.9477709350964,-31.6884975804803,
47.5208738880602));
#25968=CARTESIAN_POINT('Ctrl Pts',(-30.1602326495066,-30.6926761132785,
47.5747163197313));
#25969=CARTESIAN_POINT('Ctrl Pts',(-31.707025094587,-29.5891540246876,47.6656020144756));
#25970=CARTESIAN_POINT('Ctrl Pts',(-33.8664812013175,-30.44621090974,47.7767318036953));
#25971=CARTESIAN_POINT('Ctrl Pts',(-34.3177539537478,-32.7252787200575,
47.887861592915));
#25972=CARTESIAN_POINT('Ctrl Pts',(-32.6478434227033,-34.3405793110984,
47.9989913821348));
#25973=CARTESIAN_POINT('Ctrl Pts',(-30.5016137197587,-33.840946436515,48.1043957576505));
#25974=CARTESIAN_POINT('Ctrl Pts',(-29.9485784419762,-32.5746882809203,
48.1727568700931));
#25975=CARTESIAN_POINT('Ctrl Pts',(-29.9436300755036,-31.998396563196,48.2040747194623));
#25976=CARTESIAN_POINT('Ctrl Pts',(-29.9418540657684,-32.0000454425719,
47.4459252805377));
#25977=CARTESIAN_POINT('Ctrl Pts',(-29.9420745751735,-31.3223792418367,
47.4828360416797));
#25978=CARTESIAN_POINT('Ctrl Pts',(-30.678213927134,-29.9642036192908,47.556790065895));
#25979=CARTESIAN_POINT('Ctrl Pts',(-32.9916833923377,-29.7831153417573,
47.6677873531836));
#25980=CARTESIAN_POINT('Ctrl Pts',(-34.4003366528858,-31.6306796899659,
47.7789171424033));
#25981=CARTESIAN_POINT('Ctrl Pts',(-33.6122278392798,-33.8162419808058,
47.890046931623));
#25982=CARTESIAN_POINT('Ctrl Pts',(-31.3486255910479,-34.3395993071363,
48.0011767208428));
#25983=CARTESIAN_POINT('Ctrl Pts',(-30.068831201512,-33.0979137910051,48.0864695038143));
#25984=CARTESIAN_POINT('Ctrl Pts',(-29.9449266252224,-32.208720259441,48.1347190237126));
#25985=CARTESIAN_POINT('Ctrl Pts',(-29.9465981539402,-32.0017453557993,
48.1459252805377));
#25986=CARTESIAN_POINT('Origin',(-32.,-32.,39.4540747194623));
#25987=CARTESIAN_POINT('',(-29.9464657329942,-31.9982258658083,46.7459252805377));
#25988=CARTESIAN_POINT('',(-29.945524346234,-32.001876932627,46.8040747194623));
#25989=CARTESIAN_POINT('',(-29.94525,-31.9999999999998,39.4540747194623));
#25990=CARTESIAN_POINT('Ctrl Pts',(-29.945524346234,-32.001876932627,46.8040747194623));
#25991=CARTESIAN_POINT('Ctrl Pts',(-29.9501840246136,-31.4877588312942,
46.831947642954));
#25992=CARTESIAN_POINT('Ctrl Pts',(-30.4058569158982,-30.2830100573331,
46.896863829519));
#25993=CARTESIAN_POINT('Ctrl Pts',(-32.4282459979597,-29.6094732845848,
46.9988232791572));
#25994=CARTESIAN_POINT('Ctrl Pts',(-34.2406047769068,-31.0631420355334,
47.109953068377));
#25995=CARTESIAN_POINT('Ctrl Pts',(-34.0023863623759,-33.3742130357603,
47.2210828575967));
#25996=CARTESIAN_POINT('Ctrl Pts',(-31.9316056639743,-34.4276191683791,
47.3322126468164));
#25997=CARTESIAN_POINT('Ctrl Pts',(-30.2269905282735,-33.4359068134596,
47.4265432674383));
#25998=CARTESIAN_POINT('Ctrl Pts',(-29.9493146838935,-32.3742412168468,
47.4838306249869));
#25999=CARTESIAN_POINT('Ctrl Pts',(-29.9484710272094,-31.9994832228478,
47.5040747194623));
#26000=CARTESIAN_POINT('Ctrl Pts',(-29.9464657329942,-31.9982258658082,
46.7459252805377));
#26001=CARTESIAN_POINT('Ctrl Pts',(-29.9447989969418,-31.7961784436538,
46.7568665335004));
#26002=CARTESIAN_POINT('Ctrl Pts',(-30.0649943949212,-30.9120086993632,
46.8048510495363));
#26003=CARTESIAN_POINT('Ctrl Pts',(-31.3319469197342,-29.6651084349508,
46.8898788286455));
#26004=CARTESIAN_POINT('Ctrl Pts',(-33.5992261839687,-30.172299490863,47.0010086178653));
#26005=CARTESIAN_POINT('Ctrl Pts',(-34.4029109875207,-32.3521822321507,
47.1121384070849));
#26006=CARTESIAN_POINT('Ctrl Pts',(-33.0074777137784,-34.2097516138314,
47.2232681963047));
#26007=CARTESIAN_POINT('Ctrl Pts',(-30.6900117620269,-34.0449802822919,
47.3343979855244));
#26008=CARTESIAN_POINT('Ctrl Pts',(-29.942958779693,-32.6850089432713,47.4086170136021));
#26009=CARTESIAN_POINT('Ctrl Pts',(-29.9418532741857,-32.0024781228395,
47.4457927786065));
#26010=CARTESIAN_POINT('Ctrl Pts',(-29.9418540657684,-32.0000454425719,
47.4459252805377));
#26011=CARTESIAN_POINT('Origin',(-32.,-32.,39.4540747194623));
#26012=CARTESIAN_POINT('',(-29.9481039192408,-32.0010072981663,46.0459252805377));
#26013=CARTESIAN_POINT('',(-29.9420942139572,-31.999362613781,46.1040747194623));
#26014=CARTESIAN_POINT('',(-29.94525,-31.9999999999998,39.4540747194623));
#26015=CARTESIAN_POINT('Ctrl Pts',(-29.9420942139572,-31.999362613781,46.1040747194623));
#26016=CARTESIAN_POINT('Ctrl Pts',(-29.9419518531651,-31.9644057826194,
46.1059781347747));
#26017=CARTESIAN_POINT('Ctrl Pts',(-29.9585993357687,-31.2492759887623,
46.1449248131603));
#26018=CARTESIAN_POINT('Ctrl Pts',(-30.7889831753562,-29.8948988474869,
46.2209147546191));
#26019=CARTESIAN_POINT('Ctrl Pts',(-33.1116689024243,-29.8407860543094,
46.3320445438389));
#26020=CARTESIAN_POINT('Ctrl Pts',(-34.4169673055408,-31.7627624485277,
46.4431743330586));
#26021=CARTESIAN_POINT('Ctrl Pts',(-33.5102834415455,-33.9018560771194,
46.5543041222783));
#26022=CARTESIAN_POINT('Ctrl Pts',(-31.2214045501895,-34.3003916487017,
46.665433911498));
#26023=CARTESIAN_POINT('Ctrl Pts',(-30.0404503222317,-33.0217127646971,
46.748690777226));
#26024=CARTESIAN_POINT('Ctrl Pts',(-29.9439912873465,-32.1710245132755,
46.7949043798808));
#26025=CARTESIAN_POINT('Ctrl Pts',(-29.945524346234,-32.001876932627,46.8040747194623));
#26026=CARTESIAN_POINT('Ctrl Pts',(-29.9481039192408,-32.0010072981663,
46.0459252805377));
#26027=CARTESIAN_POINT('Ctrl Pts',(-29.9499107511001,-31.5936483051554,
46.0679402883943));
#26028=CARTESIAN_POINT('Ctrl Pts',(-30.2646015094173,-30.498279124301,46.1269985593241));
#26029=CARTESIAN_POINT('Ctrl Pts',(-32.0474055299468,-29.5718800988582,
46.2231000933271));
#26030=CARTESIAN_POINT('Ctrl Pts',(-34.06561751162,-30.7228007852025,46.3342298825469));
#26031=CARTESIAN_POINT('Ctrl Pts',(-34.1933987473477,-33.0426003422808,
46.4453596717667));
#26032=CARTESIAN_POINT('Ctrl Pts',(-32.3138052359217,-34.4082233726336,
46.5564894609863));
#26033=CARTESIAN_POINT('Ctrl Pts',(-30.360350765969,-33.6524066858803,46.6566779972433));
#26034=CARTESIAN_POINT('Ctrl Pts',(-29.950441983378,-32.4802404827688,46.7198232704271));
#26035=CARTESIAN_POINT('Ctrl Pts',(-29.9464657329942,-31.9982258658082,
46.7459252805377));
#26036=CARTESIAN_POINT('Origin',(-32.,-32.,39.4540747194623));
#26037=CARTESIAN_POINT('',(-29.9427892107444,-32.0012284764652,45.3459252805377));
#26038=CARTESIAN_POINT('',(-29.9474011798426,-31.9985278358768,45.4040747194623));
#26039=CARTESIAN_POINT('',(-29.94525,-31.9999999999998,39.4540747194623));
#26040=CARTESIAN_POINT('Ctrl Pts',(-29.9474011798426,-31.9985278358768,
45.4040747194623));
#26041=CARTESIAN_POINT('Ctrl Pts',(-29.94581141717,-31.758608449279,45.4170518896686));
#26042=CARTESIAN_POINT('Ctrl Pts',(-30.0955923500213,-30.8357624344355,
45.4670723229481));
#26043=CARTESIAN_POINT('Ctrl Pts',(-31.4608924178518,-29.6320102139679,
45.5541360193008));
#26044=CARTESIAN_POINT('Ctrl Pts',(-33.6969732951919,-30.2626761248151,
45.6652658085205));
#26045=CARTESIAN_POINT('Ctrl Pts',(-34.3800026156816,-32.4833220057386,
45.7763955977402));
#26046=CARTESIAN_POINT('Ctrl Pts',(-32.8848793523529,-34.2616368284191,
45.88752538696));
#26047=CARTESIAN_POINT('Ctrl Pts',(-30.6194030494022,-33.9751191057943,
45.9967517608673));
#26048=CARTESIAN_POINT('Ctrl Pts',(-29.9447224036788,-32.6447171600214,
46.0689348717014));
#26049=CARTESIAN_POINT('Ctrl Pts',(-29.9420942139572,-31.999362613781,46.1040747194623));
#26050=CARTESIAN_POINT('Ctrl Pts',(-29.9427892107444,-32.0012284764652,
45.3459252805377));
#26051=CARTESIAN_POINT('Ctrl Pts',(-29.9470895307118,-31.3929993370659,
45.3790140432881));
#26052=CARTESIAN_POINT('Ctrl Pts',(-30.5546547538757,-30.0963856466631,
45.4491460691119));
#26053=CARTESIAN_POINT('Ctrl Pts',(-32.7586800166002,-29.6929633355749,
45.5563213580088));
#26054=CARTESIAN_POINT('Ctrl Pts',(-34.3496925798768,-31.3860306858952,
45.6674511472285));
#26055=CARTESIAN_POINT('Ctrl Pts',(-33.7902919754051,-33.6409960942643,
45.7785809364483));
#26056=CARTESIAN_POINT('Ctrl Pts',(-31.5924355699507,-34.3941396730243,
45.889710725668));
#26057=CARTESIAN_POINT('Ctrl Pts',(-30.1290852814386,-33.2410524482903,
45.9788255070311));
#26058=CARTESIAN_POINT('Ctrl Pts',(-29.9468705092646,-32.2790855505863,
46.030897025321));
#26059=CARTESIAN_POINT('Ctrl Pts',(-29.9481039192408,-32.0010072981663,
46.0459252805377));
#26060=CARTESIAN_POINT('Origin',(-32.,-32.,39.4540747194623));
#26061=CARTESIAN_POINT('',(-29.9443798132546,-31.9982099715446,44.6459252805377));
#26062=CARTESIAN_POINT('',(-29.9474073488643,-32.0014692601838,44.7040747194623));
#26063=CARTESIAN_POINT('',(-29.94525,-31.9999999999998,39.4540747194623));
#26064=CARTESIAN_POINT('Ctrl Pts',(-29.9474073488643,-32.0014692601838,
44.7040747194623));
#26065=CARTESIAN_POINT('Ctrl Pts',(-29.9503473165645,-31.5568170973055,
44.7281256445624));
#26066=CARTESIAN_POINT('Ctrl Pts',(-30.3107091196527,-30.4229700275786,
44.7892198327358));
#26067=CARTESIAN_POINT('Ctrl Pts',(-32.1803845633948,-29.5781259278874,
44.8873572839824));
#26068=CARTESIAN_POINT('Ctrl Pts',(-34.1324988340666,-30.8379064862986,
44.9984870732022));
#26069=CARTESIAN_POINT('Ctrl Pts',(-34.1329732977875,-33.1612224260699,
45.1096168624218));
#26070=CARTESIAN_POINT('Ctrl Pts',(-32.1813737305056,-34.4218001944348,
45.2207466516416));
#26071=CARTESIAN_POINT('Ctrl Pts',(-30.3110643538795,-33.5775893512171,
45.3188992706551));
#26072=CARTESIAN_POINT('Ctrl Pts',(-29.9503493862318,-32.4434570574783,
45.3800086265953));
#26073=CARTESIAN_POINT('Ctrl Pts',(-29.9474011798426,-31.9985278358768,
45.4040747194623));
#26074=CARTESIAN_POINT('Ctrl Pts',(-29.9443798132547,-31.9982099715446,
44.6459252805377));
#26075=CARTESIAN_POINT('Ctrl Pts',(-29.943180692852,-31.867082129172,44.6530445351088));
#26076=CARTESIAN_POINT('Ctrl Pts',(-30.014346413535,-31.0549598855982,44.6972070527531));
#26077=CARTESIAN_POINT('Ctrl Pts',(-31.0956022698719,-29.7460970996221,
44.7784128334707));
#26078=CARTESIAN_POINT('Ctrl Pts',(-33.4029916207618,-30.0176710538707,
44.8895426226904));
#26079=CARTESIAN_POINT('Ctrl Pts',(-34.4263782551407,-32.1034509621539,
45.0006724119102));
#26080=CARTESIAN_POINT('Ctrl Pts',(-33.2291698233915,-34.0945536717531,
45.1118022011298));
#26081=CARTESIAN_POINT('Ctrl Pts',(-30.907038499066,-34.1687435754524,45.2229319903497));
#26082=CARTESIAN_POINT('Ctrl Pts',(-29.9787573653101,-32.8270079213671,
45.3009730168189));
#26083=CARTESIAN_POINT('Ctrl Pts',(-29.9422752714102,-32.0739190858488,
45.3419707802149));
#26084=CARTESIAN_POINT('Ctrl Pts',(-29.9427892107444,-32.0012284764652,
45.3459252805377));
#26085=CARTESIAN_POINT('Origin',(-32.,-32.,39.4540747194623));
#26086=CARTESIAN_POINT('',(-29.9485867049726,-31.9999002048695,43.9459252805377));
#26087=CARTESIAN_POINT('',(-29.9420978900125,-32.0006422249924,44.0040747194623));
#26088=CARTESIAN_POINT('',(-29.94525,-31.9999999999998,39.4540747194623));
#26089=CARTESIAN_POINT('Ctrl Pts',(-29.9420978900125,-32.0006422249924,
44.0040747194623));
#26090=CARTESIAN_POINT('Ctrl Pts',(-29.9447425969129,-31.3555631669369,
44.0391993994563));
#26091=CARTESIAN_POINT('Ctrl Pts',(-30.6189110335615,-30.0254050294705,
44.1113673425236));
#26092=CARTESIAN_POINT('Ctrl Pts',(-32.8839555431527,-29.7380019430538,
44.2205785486641));
#26093=CARTESIAN_POINT('Ctrl Pts',(-34.3798050107393,-31.5157059542584,
44.3317083378838));
#26094=CARTESIAN_POINT('Ctrl Pts',(-33.6976827404077,-33.7366306241687,
44.4428381271036));
#26095=CARTESIAN_POINT('Ctrl Pts',(-31.4618596366578,-34.3682097798181,
44.5539679163232));
#26096=CARTESIAN_POINT('Ctrl Pts',(-30.0958300853345,-33.1648056843117,
44.6410467804429));
#26097=CARTESIAN_POINT('Ctrl Pts',(-29.9458191748613,-32.2416708805599,
44.6910823814892));
#26098=CARTESIAN_POINT('Ctrl Pts',(-29.9474073488643,-32.0014692601838,
44.7040747194623));
#26099=CARTESIAN_POINT('Ctrl Pts',(-29.9485867049726,-31.9999002048695,
43.9459252805377));
#26100=CARTESIAN_POINT('Ctrl Pts',(-29.948440755186,-31.6630643448139,43.9641182900027));
#26101=CARTESIAN_POINT('Ctrl Pts',(-30.1862445800855,-30.6405822494248,
44.0193545625409));
#26102=CARTESIAN_POINT('Ctrl Pts',(-31.7976970806331,-29.5798580480631,
44.1116340981523));
#26103=CARTESIAN_POINT('Ctrl Pts',(-33.923471884996,-30.5173437869082,44.2227638873721));
#26104=CARTESIAN_POINT('Ctrl Pts',(-34.2889060793629,-32.8117404131962,
44.3338936765918));
#26105=CARTESIAN_POINT('Ctrl Pts',(-32.5595582520656,-34.3632410163062,
44.4450234658115));
#26106=CARTESIAN_POINT('Ctrl Pts',(-30.4617016867902,-33.7910912546249,
44.5490340004601));
#26107=CARTESIAN_POINT('Ctrl Pts',(-29.9494200163777,-32.5493731067912,
44.6160012720355));
#26108=CARTESIAN_POINT('Ctrl Pts',(-29.9443798132547,-31.9982099715446,
44.6459252805377));
#26109=CARTESIAN_POINT('Origin',(-32.,-32.,39.4540747194623));
#26110=CARTESIAN_POINT('',(-29.9447460435121,-32.001842447186,43.2459252805377));
#26111=CARTESIAN_POINT('',(-29.9455159708164,-31.9981228849833,43.3040747194623));
#26112=CARTESIAN_POINT('',(-29.94525,-31.9999999999998,39.4540747194623));
#26113=CARTESIAN_POINT('Ctrl Pts',(-29.9455159708164,-31.9981228849833,
43.3040747194623));
#26114=CARTESIAN_POINT('Ctrl Pts',(-29.9439847559442,-31.8292568307923,
43.3132298912769));
#26115=CARTESIAN_POINT('Ctrl Pts',(-30.0402482322227,-30.9788546338471,
43.3594283261648));
#26116=CARTESIAN_POINT('Ctrl Pts',(-31.2204650508714,-29.6999265505474,
43.442670024126));
#26117=CARTESIAN_POINT('Ctrl Pts',(-33.5095065278182,-30.0975272261643,
43.5537998133457));
#26118=CARTESIAN_POINT('Ctrl Pts',(-34.4170640004594,-32.2362503537452,
43.6649296025654));
#26119=CARTESIAN_POINT('Ctrl Pts',(-33.1125507118291,-34.1587597191989,
43.7760593917852));
#26120=CARTESIAN_POINT('Ctrl Pts',(-30.7898430768523,-34.1055956006222,
43.8871891810049));
#26121=CARTESIAN_POINT('Ctrl Pts',(-29.9587402723266,-32.7512874624185,
43.9631942902306));
#26122=CARTESIAN_POINT('Ctrl Pts',(-29.9419534306207,-32.0358777848827,
44.0021561363831));
#26123=CARTESIAN_POINT('Ctrl Pts',(-29.9420978900125,-32.0006422249924,
44.0040747194623));
#26124=CARTESIAN_POINT('Ctrl Pts',(-29.9447460435121,-32.001842447186,43.2459252805377));
#26125=CARTESIAN_POINT('Ctrl Pts',(-29.9497235311244,-31.4625377523841,
43.2751920448965));
#26126=CARTESIAN_POINT('Ctrl Pts',(-30.4434354407804,-30.2325635251486,
43.3415020723286));
#26127=CARTESIAN_POINT('Ctrl Pts',(-32.5176476217965,-29.6272264154066,
43.444855362834));
#26128=CARTESIAN_POINT('Ctrl Pts',(-34.2741819976516,-31.1478792448328,
43.5559851520537));
#26129=CARTESIAN_POINT('Ctrl Pts',(-33.9494096698203,-33.4483837460143,
43.6671149412734));
#26130=CARTESIAN_POINT('Ctrl Pts',(-31.8405587536029,-34.4233431511784,
43.7782447304932));
#26131=CARTESIAN_POINT('Ctrl Pts',(-30.1989774834058,-33.3839529211499,
43.8711815102479));
#26132=CARTESIAN_POINT('Ctrl Pts',(-29.9487379273691,-32.3489046616982,
43.9270750269294));
#26133=CARTESIAN_POINT('Ctrl Pts',(-29.9485867049726,-31.9999002048695,
43.9459252805377));
#26134=CARTESIAN_POINT('Origin',(-32.,-32.,39.4540747194623));
#26135=CARTESIAN_POINT('',(-29.9425269848562,-31.9989451474637,42.5459252805377));
#26136=CARTESIAN_POINT('',(-29.9484731266049,-32.0005123640697,42.6040747194623));
#26137=CARTESIAN_POINT('',(-29.94525,-31.9999999999998,39.4540747194623));
#26138=CARTESIAN_POINT('Ctrl Pts',(-29.9484731266049,-32.0005123640697,
42.6040747194623));
#26139=CARTESIAN_POINT('Ctrl Pts',(-29.9493088636411,-31.6260341876009,
42.6243036461708));
#26140=CARTESIAN_POINT('Ctrl Pts',(-30.2266782234694,-30.5646578541764,
42.6815758359526));
#26141=CARTESIAN_POINT('Ctrl Pts',(-31.9306141422462,-29.57240899581,42.7758912888076));
#26142=CARTESIAN_POINT('Ctrl Pts',(-34.0018249157517,-30.6249692172527,
42.8870210780274));
#26143=CARTESIAN_POINT('Ctrl Pts',(-34.2409872374696,-32.9359427480687,
42.9981508672471));
#26144=CARTESIAN_POINT('Ctrl Pts',(-32.4292223408278,-34.3903516011817,
43.1092806564668));
#26145=CARTESIAN_POINT('Ctrl Pts',(-30.406257433528,-33.7175408329679,43.2112552738719));
#26146=CARTESIAN_POINT('Ctrl Pts',(-29.9501802918094,-32.5125154081499,
43.2761866282037));
#26147=CARTESIAN_POINT('Ctrl Pts',(-29.9455159708164,-31.9981228849833,
43.3040747194623));
#26148=CARTESIAN_POINT('Ctrl Pts',(-29.9425269848562,-31.9989451474637,
42.5459252805377));
#26149=CARTESIAN_POINT('Ctrl Pts',(-29.9421476701604,-31.9383561623691,
42.5492225367172));
#26150=CARTESIAN_POINT('Ctrl Pts',(-29.9720545404929,-31.1974555822032,
42.5895630559699));
#26151=CARTESIAN_POINT('Ctrl Pts',(-30.8688288772728,-29.8509387094972,
42.6669468382958));
#26152=CARTESIAN_POINT('Ctrl Pts',(-33.1919093046072,-29.8840212783247,
42.7780766275157));
#26153=CARTESIAN_POINT('Ctrl Pts',(-34.4241674901357,-31.8536249255854,
42.8892064167353));
#26154=CARTESIAN_POINT('Ctrl Pts',(-33.4378537625072,-33.9571893024616,
43.0003362059551));
#26155=CARTESIAN_POINT('Ctrl Pts',(-31.1356319224862,-34.2695553308866,
43.1114659951748));
#26156=CARTESIAN_POINT('Ctrl Pts',(-30.0224447317067,-32.9695959958596,
43.1933290200357));
#26157=CARTESIAN_POINT('Ctrl Pts',(-29.9434234707281,-32.145141590691,43.2381487818233));
#26158=CARTESIAN_POINT('Ctrl Pts',(-29.9447460435121,-32.001842447186,43.2459252805377));
#26159=CARTESIAN_POINT('Origin',(-32.,-32.,39.4540747194623));
#26160=CARTESIAN_POINT('',(-29.9479126462767,-31.9988339667449,41.8459252805377));
#26161=CARTESIAN_POINT('',(-29.9436380165453,-32.001608018912,41.9040747194623));
#26162=CARTESIAN_POINT('',(-29.94525,-31.9999999999998,39.4540747194623));
#26163=CARTESIAN_POINT('Ctrl Pts',(-29.9436380165453,-32.001608018912,41.9040747194623));
#26164=CARTESIAN_POINT('Ctrl Pts',(-29.9485892150319,-31.4255899166451,
41.9353774010647));
#26165=CARTESIAN_POINT('Ctrl Pts',(-30.5011706140803,-30.1595907295533,
42.0037233457405));
#26166=CARTESIAN_POINT('Ctrl Pts',(-32.646887464373,-29.6591579023516,42.1091125534892));
#26167=CARTESIAN_POINT('Ctrl Pts',(-34.3174574925706,-31.2737738657493,
42.220242342709));
#26168=CARTESIAN_POINT('Ctrl Pts',(-33.8671156889712,-33.553027035053,42.3313721319286));
#26169=CARTESIAN_POINT('Ctrl Pts',(-31.7080097873483,-34.4109652269018,
42.4425019211485));
#26170=CARTESIAN_POINT('Ctrl Pts',(-30.1605085472801,-33.3078911948606,
42.5334027836596));
#26171=CARTESIAN_POINT('Ctrl Pts',(-29.9477784598121,-32.3117795959461,
42.5872603830976));
#26172=CARTESIAN_POINT('Ctrl Pts',(-29.9484731266049,-32.0005123640697,
42.6040747194623));
#26173=CARTESIAN_POINT('Ctrl Pts',(-29.9479126462767,-31.9988339667449,
41.8459252805377));
#26174=CARTESIAN_POINT('Ctrl Pts',(-29.9465310751269,-31.7329766292276,
41.8602962916111));
#26175=CARTESIAN_POINT('Ctrl Pts',(-30.1180449363604,-30.783544371031,41.9117105657577));
#26176=CARTESIAN_POINT('Ctrl Pts',(-31.5501371962138,-29.6134580581644,
42.0001681029775));
#26177=CARTESIAN_POINT('Ctrl Pts',(-33.7609665425501,-30.3275725104634,
42.1112978921973));
#26178=CARTESIAN_POINT('Ctrl Pts',(-34.3601921411462,-32.5722924840244,
42.2224276814169));
#26179=CARTESIAN_POINT('Ctrl Pts',(-32.7993885499411,-34.2932474809962,
42.3335574706367));
#26180=CARTESIAN_POINT('Ctrl Pts',(-30.5750127249874,-33.9266611661355,
42.4413900036769));
#26181=CARTESIAN_POINT('Ctrl Pts',(-29.9464091085501,-32.6190474984427,
42.512179273644));
#26182=CARTESIAN_POINT('Ctrl Pts',(-29.9425269848562,-31.9989451474637,
42.5459252805377));
#26183=CARTESIAN_POINT('Origin',(-32.,-32.,39.4540747194623));
#26184=CARTESIAN_POINT('',(-29.9473238289665,-32.0023603893952,41.1459252805377));
#26185=CARTESIAN_POINT('',(-29.9434322372613,-31.9985074052702,41.2040747194623));
#26186=CARTESIAN_POINT('',(-29.94525,-31.9999999999998,39.4540747194623));
#26187=CARTESIAN_POINT('',(-31.4698297828114,-33.9851743256717,41.));
#26188=CARTESIAN_POINT('Ctrl Pts',(-31.4698297828114,-33.9851743256717,
41.));
#26189=CARTESIAN_POINT('Ctrl Pts',(-30.8097602092473,-33.8088929660699,
41.0370432630732));
#26190=CARTESIAN_POINT('Ctrl Pts',(-30.0750747845072,-33.1128764409483,
41.0856850232525));
#26191=CARTESIAN_POINT('Ctrl Pts',(-29.9457054770538,-32.216656490295,41.1343267834317));
#26192=CARTESIAN_POINT('Ctrl Pts',(-29.9473238289665,-32.0023603893952,
41.1459252805377));
#26193=CARTESIAN_POINT('',(-32.5313020899646,-33.98873329687,41.));
#26194=CARTESIAN_POINT('Origin',(-32.,-32.,41.));
#26195=CARTESIAN_POINT('Ctrl Pts',(-32.5313027126548,-33.9887352548077,
41.));
#26196=CARTESIAN_POINT('Ctrl Pts',(-31.886832910374,-34.1600186848657,41.0363148168372));
#26197=CARTESIAN_POINT('Ctrl Pts',(-30.5071217326733,-33.8407636746777,
41.1043397233247));
#26198=CARTESIAN_POINT('Ctrl Pts',(-29.9482863554879,-32.5817335143899,
41.1723646298121));
#26199=CARTESIAN_POINT('Ctrl Pts',(-29.9434322372613,-31.9985074052702,
41.2040747194623));
#26200=CARTESIAN_POINT('Origin',(32.,-32.,172.));
#26201=CARTESIAN_POINT('',(30.3314948688693,-31.9993848803471,166.67148036339));
#26202=CARTESIAN_POINT('',(30.3351640391491,-31.9985292345028,166.47851963661));
#26203=CARTESIAN_POINT('',(30.334,-32.,172.));
#26204=CARTESIAN_POINT('',(32.6750771856746,-33.5230977622535,166.));
#26205=CARTESIAN_POINT('Ctrl Pts',(30.3351640391491,-31.9985292345028,166.47851963661));
#26206=CARTESIAN_POINT('Ctrl Pts',(30.3338126585907,-31.8287852696714,166.467186143366));
#26207=CARTESIAN_POINT('Ctrl Pts',(30.3576887735277,-31.6594223554909,166.455852650123));
#26208=CARTESIAN_POINT('Ctrl Pts',(30.4083704460928,-31.4985231798901,166.444519156879));
#26209=CARTESIAN_POINT('Ctrl Pts',(30.5740223320084,-30.9726279098336,166.407475893806));
#26210=CARTESIAN_POINT('Ctrl Pts',(31.0260364492964,-30.5371502725322,166.370432630732));
#26211=CARTESIAN_POINT('Ctrl Pts',(31.5578489866309,-30.390951172157,166.333389367659));
#26212=CARTESIAN_POINT('Ctrl Pts',(32.0896615239654,-30.2447520717818,166.296346104586));
#26213=CARTESIAN_POINT('Ctrl Pts',(32.7012724813464,-30.3878315083329,166.259302841513));
#26214=CARTESIAN_POINT('Ctrl Pts',(33.1122475059105,-30.7555629775481,166.222259578439));
#26215=CARTESIAN_POINT('Ctrl Pts',(33.5232225304745,-31.1232944467632,166.185216315366));
#26216=CARTESIAN_POINT('Ctrl Pts',(33.7335616222216,-31.7156779486424,166.148173052293));
#26217=CARTESIAN_POINT('Ctrl Pts',(33.6481326168522,-32.2595130620954,166.11112978922));
#26218=CARTESIAN_POINT('Ctrl Pts',(33.5627036114828,-32.8033481755483,166.074086526146));
#26219=CARTESIAN_POINT('Ctrl Pts',(33.181506508997,-33.298634900575,166.037043263073));
#26220=CARTESIAN_POINT('Ctrl Pts',(32.6750771856746,-33.5230977622535,166.));
#26221=CARTESIAN_POINT('',(30.334,-32.,166.));
#26222=CARTESIAN_POINT('Origin',(32.,-32.,166.));
#26223=CARTESIAN_POINT('',(30.334,-32.,165.));
#26224=CARTESIAN_POINT('',(30.334,-32.,172.));
#26225=CARTESIAN_POINT('Origin',(32.,-32.,165.));
#26226=CARTESIAN_POINT('',(30.38531543383,-32.4224457855202,166.));
#26227=CARTESIAN_POINT('Origin',(32.,-32.,166.));
#26228=CARTESIAN_POINT('Ctrl Pts',(30.385313195272,-32.4224462418485,166.));
#26229=CARTESIAN_POINT('Ctrl Pts',(30.5228540811707,-32.9453078801577,166.036314816837));
#26230=CARTESIAN_POINT('Ctrl Pts',(30.9381273047563,-33.3962489804972,166.072629633675));
#26231=CARTESIAN_POINT('Ctrl Pts',(31.4484542466326,-33.5749075296435,166.108944450512));
#26232=CARTESIAN_POINT('Ctrl Pts',(31.9690179395742,-33.7571498266643,166.145987713585));
#26233=CARTESIAN_POINT('Ctrl Pts',(32.5884870011376,-33.6560764725003,166.183030976658));
#26234=CARTESIAN_POINT('Ctrl Pts',(33.0238560671702,-33.3177567300594,166.220074239731));
#26235=CARTESIAN_POINT('Ctrl Pts',(33.4592251332029,-32.9794369876186,166.257117502805));
#26236=CARTESIAN_POINT('Ctrl Pts',(33.7104942037048,-32.4038708569011,166.294160765878));
#26237=CARTESIAN_POINT('Ctrl Pts',(33.6624581941067,-31.8545228213468,166.331204028951));
#26238=CARTESIAN_POINT('Ctrl Pts',(33.6144221845086,-31.3051747857925,166.368247292024));
#26239=CARTESIAN_POINT('Ctrl Pts',(33.2670810948105,-30.7820448454015,166.405290555098));
#26240=CARTESIAN_POINT('Ctrl Pts',(32.7794871658154,-30.524470954864,166.442333818171));
#26241=CARTESIAN_POINT('Ctrl Pts',(32.2918932368204,-30.2668970643265,166.479377081244));
#26242=CARTESIAN_POINT('Ctrl Pts',(31.6640464685286,-30.2748792236425,166.516420344317));
#26243=CARTESIAN_POINT('Ctrl Pts',(31.1831917006873,-30.5447861876656,166.553463607391));
#26244=CARTESIAN_POINT('Ctrl Pts',(30.702336932846,-30.8146931516887,166.590506870464));
#26245=CARTESIAN_POINT('Ctrl Pts',(30.3684741654553,-31.3465249204188,166.627550133537));
#26246=CARTESIAN_POINT('Ctrl Pts',(30.3344039265837,-31.896907675664,166.66459339661));
#26247=CARTESIAN_POINT('Ctrl Pts',(30.3322925160885,-31.9310161516919,166.666889052204));
#26248=CARTESIAN_POINT('Ctrl Pts',(30.3313324779548,-31.9651958739689,166.669184707797));
#26249=CARTESIAN_POINT('Ctrl Pts',(30.3314948688693,-31.9993848803471,166.67148036339));
#26250=CARTESIAN_POINT('Origin',(32.,-32.,172.));
#26251=CARTESIAN_POINT('',(30.3358443822319,-31.9988695272148,167.37148036339));
#26252=CARTESIAN_POINT('',(30.3361975811458,-32.0008966207542,167.17851963661));
#26253=CARTESIAN_POINT('',(30.334,-32.,172.));
#26254=CARTESIAN_POINT('Ctrl Pts',(30.3361975811458,-32.0008966207542,167.17851963661));
#26255=CARTESIAN_POINT('Ctrl Pts',(30.3378409630666,-31.6647641269526,167.156112388472));
#26256=CARTESIAN_POINT('Ctrl Pts',(30.4366195132904,-31.3277436672723,167.133705140335));
#26257=CARTESIAN_POINT('Ctrl Pts',(30.6258907070991,-31.0530840229842,167.111297892197));
#26258=CARTESIAN_POINT('Ctrl Pts',(30.9387904697746,-30.5990215965532,167.074254629124));
#26259=CARTESIAN_POINT('Ctrl Pts',(31.4990076484233,-30.3153919822247,167.037211366051));
#26260=CARTESIAN_POINT('Ctrl Pts',(32.0501937676499,-30.3319767966563,167.000168102978));
#26261=CARTESIAN_POINT('Ctrl Pts',(32.6013798868764,-30.3485616110878,166.963124839904));
#26262=CARTESIAN_POINT('Ctrl Pts',(33.1435349466808,-30.6653608542793,166.926081576831));
#26263=CARTESIAN_POINT('Ctrl Pts',(33.4285638569807,-31.1374206305279,166.889038313758));
#26264=CARTESIAN_POINT('Ctrl Pts',(33.7135927672805,-31.6094804067765,166.851995050685));
#26265=CARTESIAN_POINT('Ctrl Pts',(33.7414955280759,-32.2368007160821,166.814951787611));
#26266=CARTESIAN_POINT('Ctrl Pts',(33.4995200183968,-32.7322993259295,166.777908524538));
#26267=CARTESIAN_POINT('Ctrl Pts',(33.2575445087177,-33.227797935777,166.740865261465));
#26268=CARTESIAN_POINT('Ctrl Pts',(32.7456907285641,-33.5914748461662,166.703821998392));
#26269=CARTESIAN_POINT('Ctrl Pts',(32.1981475556008,-33.6569620511966,166.666778735318));
#26270=CARTESIAN_POINT('Ctrl Pts',(31.6506043826374,-33.7224492562269,166.629735472245));
#26271=CARTESIAN_POINT('Ctrl Pts',(31.0673718168642,-33.4897467558983,166.592692209172));
#26272=CARTESIAN_POINT('Ctrl Pts',(30.7154003612491,-33.0652390543282,166.555648946099));
#26273=CARTESIAN_POINT('Ctrl Pts',(30.4711155882646,-32.7706107091773,166.529939176269));
#26274=CARTESIAN_POINT('Ctrl Pts',(30.3382296149924,-32.3835895307383,166.504229406439));
#26275=CARTESIAN_POINT('Ctrl Pts',(30.3351640391491,-31.9985292345028,166.47851963661));
#26276=CARTESIAN_POINT('Ctrl Pts',(30.3314948688693,-31.9993848803471,166.67148036339));
#26277=CARTESIAN_POINT('Ctrl Pts',(30.333952857677,-32.5168780867464,166.70622797087));
#26278=CARTESIAN_POINT('Ctrl Pts',(30.5935660073833,-33.0364983358831,166.74097557835));
#26279=CARTESIAN_POINT('Ctrl Pts',(31.0099645855531,-33.3433730549829,166.77572318583));
#26280=CARTESIAN_POINT('Ctrl Pts',(31.4538731937464,-33.6705219372966,166.812766448903));
#26281=CARTESIAN_POINT('Ctrl Pts',(32.0759681204853,-33.7558859601639,166.849809711977));
#26282=CARTESIAN_POINT('Ctrl Pts',(32.5915885496141,-33.5604004805478,166.88685297505));
#26283=CARTESIAN_POINT('Ctrl Pts',(33.107208978743,-33.3649150009316,166.923896238123));
#26284=CARTESIAN_POINT('Ctrl Pts',(33.5163549102618,-32.8885800188319,166.960939501196));
#26285=CARTESIAN_POINT('Ctrl Pts',(33.6318002169891,-32.3493650813451,166.997982764269));
#26286=CARTESIAN_POINT('Ctrl Pts',(33.7472455237165,-31.8101501438584,167.035026027343));
#26287=CARTESIAN_POINT('Ctrl Pts',(33.5689902056525,-31.2080552509844,167.072069290416));
#26288=CARTESIAN_POINT('Ctrl Pts',(33.1786044854326,-30.8185951509338,167.109112553489));
#26289=CARTESIAN_POINT('Ctrl Pts',(32.7882187652126,-30.4291350508832,167.146155816562));
#26290=CARTESIAN_POINT('Ctrl Pts',(32.1857026428369,-30.2523097436559,167.183199079636));
#26291=CARTESIAN_POINT('Ctrl Pts',(31.6467634648643,-30.3690338306598,167.220242342709));
#26292=CARTESIAN_POINT('Ctrl Pts',(31.1078242868917,-30.4857579176637,167.257285605782));
#26293=CARTESIAN_POINT('Ctrl Pts',(30.6324620533223,-30.8960313988988,167.294328868856));
#26294=CARTESIAN_POINT('Ctrl Pts',(30.438200319938,-31.4121152068147,167.331372131929));
#26295=CARTESIAN_POINT('Ctrl Pts',(30.3680886548174,-31.5983767750833,167.344741542416));
#26296=CARTESIAN_POINT('Ctrl Pts',(30.3345927167679,-31.7984210368744,167.358110952903));
#26297=CARTESIAN_POINT('Ctrl Pts',(30.3358443822319,-31.9988695272148,167.37148036339));
#26298=CARTESIAN_POINT('Origin',(32.,-32.,172.));
#26299=CARTESIAN_POINT('',(30.3355908703268,-32.0012498346338,168.07148036339));
#26300=CARTESIAN_POINT('',(30.3318493573046,-32.0009136636957,167.87851963661));
#26301=CARTESIAN_POINT('',(30.334,-32.,172.));
#26302=CARTESIAN_POINT('Ctrl Pts',(30.3318493573046,-32.0009136636957,167.87851963661));
#26303=CARTESIAN_POINT('Ctrl Pts',(30.3351439225427,-31.5020077390951,167.845038633578));
#26304=CARTESIAN_POINT('Ctrl Pts',(30.5738270707978,-31.0003673701955,167.811557630547));
#26305=CARTESIAN_POINT('Ctrl Pts',(30.9647290831503,-30.6911683371181,167.778076627516));
#26306=CARTESIAN_POINT('Ctrl Pts',(31.3972216839798,-30.3490716229446,167.741033364442));
#26307=CARTESIAN_POINT('Ctrl Pts',(32.0160473928934,-30.2425448720619,167.703990101369));
#26308=CARTESIAN_POINT('Ctrl Pts',(32.5380349752617,-30.4203340671972,167.666946838296));
#26309=CARTESIAN_POINT('Ctrl Pts',(33.0600225576301,-30.5981232623325,167.629903575223));
#26310=CARTESIAN_POINT('Ctrl Pts',(33.4851720134531,-31.0602284034857,167.592860312149));
#26311=CARTESIAN_POINT('Ctrl Pts',(33.6189371464225,-31.595192848343,167.555817049076));
#26312=CARTESIAN_POINT('Ctrl Pts',(33.7527022793919,-32.1301572932002,167.518773786003));
#26313=CARTESIAN_POINT('Ctrl Pts',(33.5950830895075,-32.7379810417613,167.48173052293));
#26314=CARTESIAN_POINT('Ctrl Pts',(33.2182054885714,-33.1405269073384,167.444687259856));
#26315=CARTESIAN_POINT('Ctrl Pts',(32.8413278876354,-33.5430727729154,167.407643996783));
#26316=CARTESIAN_POINT('Ctrl Pts',(32.2451918756475,-33.7403407555083,167.37060073371));
#26317=CARTESIAN_POINT('Ctrl Pts',(31.7025856008802,-33.6420627782017,167.333557470637));
#26318=CARTESIAN_POINT('Ctrl Pts',(31.1599793261128,-33.543784800895,167.296514207563));
#26319=CARTESIAN_POINT('Ctrl Pts',(30.6709027885658,-33.1499608636888,167.25947094449));
#26320=CARTESIAN_POINT('Ctrl Pts',(30.4591556931435,-32.6408012758188,167.222427681417));
#26321=CARTESIAN_POINT('Ctrl Pts',(30.3754931484841,-32.4396292754474,167.207791666481));
#26322=CARTESIAN_POINT('Ctrl Pts',(30.3351241533785,-32.2204523720658,167.193155651546));
#26323=CARTESIAN_POINT('Ctrl Pts',(30.3361975811458,-32.0008966207542,167.17851963661));
#26324=CARTESIAN_POINT('Ctrl Pts',(30.3358443822319,-31.9988695272148,167.37148036339));
#26325=CARTESIAN_POINT('Ctrl Pts',(30.3380607659467,-32.3538132261889,167.395154215976));
#26326=CARTESIAN_POINT('Ctrl Pts',(30.4492299054888,-32.7100244029166,167.418828068562));
#26327=CARTESIAN_POINT('Ctrl Pts',(30.6589794872193,-32.9932222989656,167.442501921148));
#26328=CARTESIAN_POINT('Ctrl Pts',(30.987181621084,-33.4363514486041,167.479545184222));
#26329=CARTESIAN_POINT('Ctrl Pts',(31.5567471220124,-33.7007156132847,167.516588447295));
#26330=CARTESIAN_POINT('Ctrl Pts',(32.1070459956353,-33.6653431492089,167.553631710368));
#26331=CARTESIAN_POINT('Ctrl Pts',(32.6573448692581,-33.6299706851331,167.590674973441));
#26332=CARTESIAN_POINT('Ctrl Pts',(33.1883771155753,-33.2948615923009,167.627718236515));
#26333=CARTESIAN_POINT('Ctrl Pts',(33.4571452136192,-32.8133599919722,167.664761499588));
#26334=CARTESIAN_POINT('Ctrl Pts',(33.7259133116631,-32.3318583916434,167.701804762661));
#26335=CARTESIAN_POINT('Ctrl Pts',(33.7324172614337,-31.7039642838181,167.738848025734));
#26336=CARTESIAN_POINT('Ctrl Pts',(33.4736809126159,-31.2169985990609,167.775891288808));
#26337=CARTESIAN_POINT('Ctrl Pts',(33.214944563798,-30.7300329143038,167.812934551881));
#26338=CARTESIAN_POINT('Ctrl Pts',(32.6909679163918,-30.3839956526149,167.849977814954));
#26339=CARTESIAN_POINT('Ctrl Pts',(32.1415198323818,-30.3372315928392,167.887021078027));
#26340=CARTESIAN_POINT('Ctrl Pts',(31.5920717483718,-30.2904675330635,167.924064341101));
#26341=CARTESIAN_POINT('Ctrl Pts',(31.0171522277581,-30.5429766752011,167.961107604174));
#26342=CARTESIAN_POINT('Ctrl Pts',(30.6798413310688,-30.9792122029183,167.998150867247));
#26343=CARTESIAN_POINT('Ctrl Pts',(30.4572652038981,-31.2670641971662,168.022594032628));
#26344=CARTESIAN_POINT('Ctrl Pts',(30.3381457763264,-31.6349121325016,168.047037198009));
#26345=CARTESIAN_POINT('Ctrl Pts',(30.3355908703268,-32.0012498346338,168.07148036339));
#26346=CARTESIAN_POINT('Origin',(32.,-32.,172.));
#26347=CARTESIAN_POINT('',(30.331348159225,-32.0004179215413,168.77148036339));
#26348=CARTESIAN_POINT('',(30.3334459265416,-31.9985209914786,168.57851963661));
#26349=CARTESIAN_POINT('',(30.334,-32.,172.));
#26350=CARTESIAN_POINT('Ctrl Pts',(30.3334459265416,-31.9985209914786,168.57851963661));
#26351=CARTESIAN_POINT('Ctrl Pts',(30.3324126580069,-31.8863119073345,168.571008141758));
#26352=CARTESIAN_POINT('Ctrl Pts',(30.3427777477924,-31.7742926336736,168.563496646906));
#26353=CARTESIAN_POINT('Ctrl Pts',(30.3652411290288,-31.6647543980759,168.555985152054));
#26354=CARTESIAN_POINT('Ctrl Pts',(30.4760202691391,-31.1245618321822,168.518941888981));
#26355=CARTESIAN_POINT('Ctrl Pts',(30.8810313161917,-30.6447084111596,168.481898625907));
#26356=CARTESIAN_POINT('Ctrl Pts',(31.3949434107614,-30.444772459129,168.444855362834));
#26357=CARTESIAN_POINT('Ctrl Pts',(31.908855505331,-30.2448365070984,168.407812099761));
#26358=CARTESIAN_POINT('Ctrl Pts',(32.5316686474178,-30.3248180240599,168.370768836687));
#26359=CARTESIAN_POINT('Ctrl Pts',(32.9783869210295,-30.6481179003979,168.333725573614));
#26360=CARTESIAN_POINT('Ctrl Pts',(33.4251051946411,-30.9714177767359,168.296682310541));
#26361=CARTESIAN_POINT('Ctrl Pts',(33.6957285997776,-31.5380360124503,168.259639047468));
#26362=CARTESIAN_POINT('Ctrl Pts',(33.6664213320894,-32.0886911775499,168.222595784395));
#26363=CARTESIAN_POINT('Ctrl Pts',(33.6371140644012,-32.6393463426495,168.185552521321));
#26364=CARTESIAN_POINT('Ctrl Pts',(33.3078761238883,-33.1740384371342,168.148509258248));
#26365=CARTESIAN_POINT('Ctrl Pts',(32.8293650100735,-33.4480952531079,168.111465995175));
#26366=CARTESIAN_POINT('Ctrl Pts',(32.3508538962588,-33.7221520690815,168.074422732102));
#26367=CARTESIAN_POINT('Ctrl Pts',(31.7230696091422,-33.7355736065441,168.037379469028));
#26368=CARTESIAN_POINT('Ctrl Pts',(31.2332828280513,-33.482218252311,168.000336205955));
#26369=CARTESIAN_POINT('Ctrl Pts',(30.7434960469603,-33.2288628980779,167.963292942882));
#26370=CARTESIAN_POINT('Ctrl Pts',(30.3917067718951,-32.7087306521491,167.926249679809));
#26371=CARTESIAN_POINT('Ctrl Pts',(30.3388918807352,-32.1598311904525,167.889206416735));
#26372=CARTESIAN_POINT('Ctrl Pts',(30.3338129443569,-32.1070463530174,167.885644156694));
#26373=CARTESIAN_POINT('Ctrl Pts',(30.3314988272416,-32.0539954855925,167.882081896652));
#26374=CARTESIAN_POINT('Ctrl Pts',(30.3318493573046,-32.0009136636957,167.87851963661));
#26375=CARTESIAN_POINT('Ctrl Pts',(30.3355908703268,-32.0012498346338,168.07148036339));
#26376=CARTESIAN_POINT('Ctrl Pts',(30.334273853292,-32.1900916136439,168.084080461082));
#26377=CARTESIAN_POINT('Ctrl Pts',(30.3639309805944,-32.3785320854588,168.096680558775));
#26378=CARTESIAN_POINT('Ctrl Pts',(30.4263577295918,-32.5554067339021,168.109280656467));
#26379=CARTESIAN_POINT('Ctrl Pts',(30.6098872975689,-33.0754038238718,168.14632391954));
#26380=CARTESIAN_POINT('Ctrl Pts',(31.076648706288,-33.4954360905143,168.183367182613));
#26381=CARTESIAN_POINT('Ctrl Pts',(31.6130544672979,-33.6232990456459,168.220410445686));
#26382=CARTESIAN_POINT('Ctrl Pts',(32.1494602283077,-33.7511620007776,168.25745370876));
#26383=CARTESIAN_POINT('Ctrl Pts',(32.7555103416085,-33.5868556443984,168.294496971833));
#26384=CARTESIAN_POINT('Ctrl Pts',(33.1538795608996,-33.205565674518,168.331540234906));
#26385=CARTESIAN_POINT('Ctrl Pts',(33.5522487801907,-32.8242757046377,168.36858349798));
#26386=CARTESIAN_POINT('Ctrl Pts',(33.7429371054722,-32.2260021212562,168.405626761053));
#26387=CARTESIAN_POINT('Ctrl Pts',(33.6386865933661,-31.6845116720053,168.442670024126));
#26388=CARTESIAN_POINT('Ctrl Pts',(33.53443608126,-31.1430212227544,168.479713287199));
#26389=CARTESIAN_POINT('Ctrl Pts',(33.1352467317664,-30.6583139076341,168.516756550272));
#26390=CARTESIAN_POINT('Ctrl Pts',(32.6237854265488,-30.4521891658866,168.553799813346));
#26391=CARTESIAN_POINT('Ctrl Pts',(32.1123241213312,-30.246064424139,168.590843076419));
#26392=CARTESIAN_POINT('Ctrl Pts',(31.4885908603897,-30.3185222557641,168.627886339492));
#26393=CARTESIAN_POINT('Ctrl Pts',(31.0380026019522,-30.6364063498675,168.664929602565));
#26394=CARTESIAN_POINT('Ctrl Pts',(30.6059805303517,-30.9411922431787,168.70044652284));
#26395=CARTESIAN_POINT('Ctrl Pts',(30.3331287789836,-31.4715958339525,168.735963443115));
#26396=CARTESIAN_POINT('Ctrl Pts',(30.331348159225,-32.0004179215413,168.77148036339));
#26397=CARTESIAN_POINT('Origin',(32.,-32.,172.));
#26398=CARTESIAN_POINT('',(30.3343646455143,-31.9984849817613,169.47148036339));
#26399=CARTESIAN_POINT('',(30.3366835507802,-32.0000156713773,169.27851963661));
#26400=CARTESIAN_POINT('',(30.334,-32.,172.));
#26401=CARTESIAN_POINT('Ctrl Pts',(30.3366835507802,-32.0000156713773,169.27851963661));
#26402=CARTESIAN_POINT('Ctrl Pts',(30.3367069615302,-31.7210138591281,169.259934386864));
#26403=CARTESIAN_POINT('Ctrl Pts',(30.4031258453532,-31.4420015723541,169.241349137118));
#26404=CARTESIAN_POINT('Ctrl Pts',(30.5358780363316,-31.1992671761327,169.222763887372));
#26405=CARTESIAN_POINT('Ctrl Pts',(30.8004735839401,-30.7154601668603,169.185720624299));
#26406=CARTESIAN_POINT('Ctrl Pts',(31.3285889721842,-30.3757729723078,169.148677361226));
#26407=CARTESIAN_POINT('Ctrl Pts',(31.8785614629847,-30.3356446108332,169.111634098152));
#26408=CARTESIAN_POINT('Ctrl Pts',(32.4285339537853,-30.2955162493585,169.074590835079));
#26409=CARTESIAN_POINT('Ctrl Pts',(33.0003635471422,-30.5549467209617,169.037547572006));
#26410=CARTESIAN_POINT('Ctrl Pts',(33.3323841217629,-30.9952220485243,169.000504308933));
#26411=CARTESIAN_POINT('Ctrl Pts',(33.6644046963836,-31.4354973760869,168.963461045859));
#26412=CARTESIAN_POINT('Ctrl Pts',(33.7566162522682,-32.0566175596089,168.926417782786));
#26413=CARTESIAN_POINT('Ctrl Pts',(33.5668232814184,-32.574361371027,168.889374519713));
#26414=CARTESIAN_POINT('Ctrl Pts',(33.3770303105685,-33.0921051824452,168.85233125664));
#26415=CARTESIAN_POINT('Ctrl Pts',(32.9052328129843,-33.5064726217596,168.815287993567));
#26416=CARTESIAN_POINT('Ctrl Pts',(32.3673227653892,-33.6278513954876,168.778244730493));
#26417=CARTESIAN_POINT('Ctrl Pts',(31.829412717794,-33.7492301692157,168.74120146742));
#26418=CARTESIAN_POINT('Ctrl Pts',(31.2253901201881,-33.5776202773574,168.704158204347));
#26419=CARTESIAN_POINT('Ctrl Pts',(30.8316524379692,-33.1915494760459,168.667114941273));
#26420=CARTESIAN_POINT('Ctrl Pts',(30.5177554157697,-32.8837646732125,168.637583173052));
#26421=CARTESIAN_POINT('Ctrl Pts',(30.3375082666587,-32.4396758788251,168.608051404831));
#26422=CARTESIAN_POINT('Ctrl Pts',(30.3334459265416,-31.9985209914786,168.57851963661));
#26423=CARTESIAN_POINT('Ctrl Pts',(30.331348159225,-32.0004179215413,168.77148036339));
#26424=CARTESIAN_POINT('Ctrl Pts',(30.331271636933,-32.0231440976491,168.773006706189));
#26425=CARTESIAN_POINT('Ctrl Pts',(30.3316957445959,-32.0458673529448,168.774533048987));
#26426=CARTESIAN_POINT('Ctrl Pts',(30.3326293636575,-32.0685696548783,168.776059391785));
#26427=CARTESIAN_POINT('Ctrl Pts',(30.3552876397336,-32.6195385092039,168.813102654858));
#26428=CARTESIAN_POINT('Ctrl Pts',(30.6780474478191,-33.1581658612735,168.850145917932));
#26429=CARTESIAN_POINT('Ctrl Pts',(31.1532156498442,-33.4379787553583,168.887189181005));
#26430=CARTESIAN_POINT('Ctrl Pts',(31.6283838518693,-33.717791649443,168.924232444078));
#26431=CARTESIAN_POINT('Ctrl Pts',(32.2559604478339,-33.7387900855429,168.961275707151));
#26432=CARTESIAN_POINT('Ctrl Pts',(32.7487697903083,-33.4913652931613,168.998318970225));
#26433=CARTESIAN_POINT('Ctrl Pts',(33.2415791327826,-33.2439405007796,169.035362233298));
#26434=CARTESIAN_POINT('Ctrl Pts',(33.5996212217667,-32.7280924799166,169.072405496371));
#26435=CARTESIAN_POINT('Ctrl Pts',(33.6590579387482,-32.1798704878478,169.109448759444));
#26436=CARTESIAN_POINT('Ctrl Pts',(33.7184946557296,-31.6316484957791,169.146492022518));
#26437=CARTESIAN_POINT('Ctrl Pts',(33.4793260007084,-31.0510525325048,169.183535285591));
#26438=CARTESIAN_POINT('Ctrl Pts',(33.050994253382,-30.7037601626695,169.220578548664));
#26439=CARTESIAN_POINT('Ctrl Pts',(32.6226625060557,-30.3564677928342,169.257621811737));
#26440=CARTESIAN_POINT('Ctrl Pts',(32.0051676664242,-30.2424790164378,169.29466507481));
#26441=CARTESIAN_POINT('Ctrl Pts',(31.4810720248777,-30.4139544794807,169.331708337884));
#26442=CARTESIAN_POINT('Ctrl Pts',(30.9569763833312,-30.5854299425236,169.368751600957));
#26443=CARTESIAN_POINT('Ctrl Pts',(30.5262799398696,-31.0423696450056,169.40579486403));
#26444=CARTESIAN_POINT('Ctrl Pts',(30.3860670516662,-31.5756804567236,169.442838127103));
#26445=CARTESIAN_POINT('Ctrl Pts',(30.3499290305059,-31.7131342788782,169.452385539199));
#26446=CARTESIAN_POINT('Ctrl Pts',(30.3330873259591,-31.8556613007967,169.461932951295));
#26447=CARTESIAN_POINT('Ctrl Pts',(30.3343646455143,-31.9984849817613,169.47148036339));
#26448=CARTESIAN_POINT('Origin',(32.,-32.,172.));
#26449=CARTESIAN_POINT('',(30.3365390411281,-32.0005076151419,170.17148036339));
#26450=CARTESIAN_POINT('',(30.333388412875,-32.0014707790079,169.97851963661));
#26451=CARTESIAN_POINT('',(30.334,-32.,172.));
#26452=CARTESIAN_POINT('Ctrl Pts',(30.333388412875,-32.0014707790079,169.97851963661));
#26453=CARTESIAN_POINT('Ctrl Pts',(30.3374606408701,-31.5584545318011,169.94886063197));
#26454=CARTESIAN_POINT('Ctrl Pts',(30.5194351289634,-31.1124834732387,169.91920162733));
#26455=CARTESIAN_POINT('Ctrl Pts',(30.8357417913499,-30.8044545164215,169.88954262269));
#26456=CARTESIAN_POINT('Ctrl Pts',(31.2307999212129,-30.4197350081262,169.852499359617));
#26457=CARTESIAN_POINT('Ctrl Pts',(31.8354069446881,-30.2501956303943,169.815456096544));
#26458=CARTESIAN_POINT('Ctrl Pts',(32.3728979661781,-30.3734166831869,169.778412833471));
#26459=CARTESIAN_POINT('Ctrl Pts',(32.9103889876682,-30.4966377359796,169.741369570397));
#26460=CARTESIAN_POINT('Ctrl Pts',(33.3807640071732,-30.9126192192969,169.704326307324));
#26461=CARTESIAN_POINT('Ctrl Pts',(33.5687819662701,-31.4310102619383,169.667283044251));
#26462=CARTESIAN_POINT('Ctrl Pts',(33.7567999253671,-31.9494013045796,169.630239781178));
#26463=CARTESIAN_POINT('Ctrl Pts',(33.6624608240559,-32.570201906545,169.593196518104));
#26464=CARTESIAN_POINT('Ctrl Pts',(33.3289337235639,-33.0093370785267,169.556153255031));
#26465=CARTESIAN_POINT('Ctrl Pts',(32.9954066230718,-33.4484722505083,169.519109991958));
#26466=CARTESIAN_POINT('Ctrl Pts',(32.4226915233989,-33.7059419925063,169.482066728885));
#26467=CARTESIAN_POINT('Ctrl Pts',(31.8728597487378,-33.6639295466528,169.445023465811));
#26468=CARTESIAN_POINT('Ctrl Pts',(31.3230279740766,-33.6219171007993,169.407980202738));
#26469=CARTESIAN_POINT('Ctrl Pts',(30.7960795244272,-33.2804224670944,169.370936939665));
#26470=CARTESIAN_POINT('Ctrl Pts',(30.5331431530888,-32.7957117382458,169.333893676592));
#26471=CARTESIAN_POINT('Ctrl Pts',(30.4021265351196,-32.5541888174575,169.315435663264));
#26472=CARTESIAN_POINT('Ctrl Pts',(30.3366603003024,-32.2771074102156,169.296977649937));
#26473=CARTESIAN_POINT('Ctrl Pts',(30.3366835507802,-32.0000156713773,169.27851963661));
#26474=CARTESIAN_POINT('Ctrl Pts',(30.3343646455143,-31.9984849817613,169.47148036339));
#26475=CARTESIAN_POINT('Ctrl Pts',(30.3380432327368,-32.4098067733181,169.498976214368));
#26476=CARTESIAN_POINT('Ctrl Pts',(30.4920006469433,-32.8235890491262,169.526472065346));
#26477=CARTESIAN_POINT('Ctrl Pts',(30.7681160103956,-33.1257390784193,169.553967916323));
#26478=CARTESIAN_POINT('Ctrl Pts',(31.1401071902734,-33.5328049674431,169.591011179396));
#26479=CARTESIAN_POINT('Ctrl Pts',(31.7338188829742,-33.7372548245368,169.62805444247));
#26480=CARTESIAN_POINT('Ctrl Pts',(32.2775718371854,-33.6455335036776,169.665097705543));
#26481=CARTESIAN_POINT('Ctrl Pts',(32.8213247913967,-33.5538121828183,169.702140968616));
#26482=CARTESIAN_POINT('Ctrl Pts',(33.3151190071186,-33.1659196840061,169.739184231689));
#26483=CARTESIAN_POINT('Ctrl Pts',(33.5329969287243,-32.6593535114379,169.776227494763));
#26484=CARTESIAN_POINT('Ctrl Pts',(33.7508748503301,-32.1527873388697,169.813270757836));
#26485=CARTESIAN_POINT('Ctrl Pts',(33.6928364778198,-31.5275474925455,169.850314020909));
#26486=CARTESIAN_POINT('Ctrl Pts',(33.3854398557542,-31.0697403359214,169.887357283982));
#26487=CARTESIAN_POINT('Ctrl Pts',(33.0780432336886,-30.6119331792972,169.924400547056));
#26488=CARTESIAN_POINT('Ctrl Pts',(32.5212883620675,-30.3215587123731,169.961443810129));
#26489=CARTESIAN_POINT('Ctrl Pts',(31.9699432512674,-30.3314907167236,169.998487073202));
#26490=CARTESIAN_POINT('Ctrl Pts',(31.4185981404672,-30.3414227210741,170.035530336275));
#26491=CARTESIAN_POINT('Ctrl Pts',(30.8726627904879,-30.6516611966991,170.072573599349));
#26492=CARTESIAN_POINT('Ctrl Pts',(30.5819542572688,-31.1202426993507,170.109616862422));
#26493=CARTESIAN_POINT('Ctrl Pts',(30.420123232909,-31.3810916800477,170.130238029411));
#26494=CARTESIAN_POINT('Ctrl Pts',(30.3373845277505,-31.6910096316149,170.150859196401));
#26495=CARTESIAN_POINT('Ctrl Pts',(30.3365390411281,-32.0005076151419,170.17148036339));
#26496=CARTESIAN_POINT('Origin',(32.,-32.,172.));
#26497=CARTESIAN_POINT('',(30.3325051052426,-32.0012453678659,170.87148036339));
#26498=CARTESIAN_POINT('',(30.3318905468311,-31.9990590648467,170.67851963661));
#26499=CARTESIAN_POINT('',(30.334,-32.,172.));
#26500=CARTESIAN_POINT('Ctrl Pts',(30.3318905468311,-31.9990590648467,170.67851963661));
#26501=CARTESIAN_POINT('Ctrl Pts',(30.3315188547892,-31.9440776971841,170.674830140149));
#26502=CARTESIAN_POINT('Ctrl Pts',(30.3340016227238,-31.889130307882,170.671140643689));
#26503=CARTESIAN_POINT('Ctrl Pts',(30.3394492489536,-31.8344784518149,170.667451147228));
#26504=CARTESIAN_POINT('Ctrl Pts',(30.3941444773462,-31.2857631722528,170.630407884155));
#26505=CARTESIAN_POINT('Ctrl Pts',(30.7477137614107,-30.7668392714703,170.593364621082));
#26506=CARTESIAN_POINT('Ctrl Pts',(31.2383657139088,-30.5151635127178,170.556321358009));
#26507=CARTESIAN_POINT('Ctrl Pts',(31.7290176664068,-30.2634877539653,170.519278094935));
#26508=CARTESIAN_POINT('Ctrl Pts',(32.3567522873385,-30.2790601372428,170.482234831862));
#26509=CARTESIAN_POINT('Ctrl Pts',(32.8343216179147,-30.5547548244002,170.445191568789));
#26510=CARTESIAN_POINT('Ctrl Pts',(33.3118909484909,-30.8304495115576,170.408148305716));
#26511=CARTESIAN_POINT('Ctrl Pts',(33.6392949887116,-31.366266502595,170.371105042643));
#26512=CARTESIAN_POINT('Ctrl Pts',(33.6667154250463,-31.9170188477602,170.334061779569));
#26513=CARTESIAN_POINT('Ctrl Pts',(33.694135861381,-32.4677711929255,170.297018516496));
#26514=CARTESIAN_POINT('Ctrl Pts',(33.4215726938297,-33.0334588922186,170.259975253423));
#26515=CARTESIAN_POINT('Ctrl Pts',(32.9737493499516,-33.355226321757,170.22293199035));
#26516=CARTESIAN_POINT('Ctrl Pts',(32.5259260060736,-33.6769937512953,170.185888727276));
#26517=CARTESIAN_POINT('Ctrl Pts',(31.9028424858688,-33.7548409110788,170.148845464203));
#26518=CARTESIAN_POINT('Ctrl Pts',(31.3896184296533,-33.5531453628992,170.11180220113));
#26519=CARTESIAN_POINT('Ctrl Pts',(30.8763943734377,-33.3514498147196,170.074758938057));
#26520=CARTESIAN_POINT('Ctrl Pts',(30.4730297812114,-32.8702115585768,170.037715674983));
#26521=CARTESIAN_POINT('Ctrl Pts',(30.3641021032237,-32.3296426110762,170.00067241191));
#26522=CARTESIAN_POINT('Ctrl Pts',(30.3423883000087,-32.2218848036297,169.993288153477));
#26523=CARTESIAN_POINT('Ctrl Pts',(30.3323745425755,-32.1117693712673,169.985903895043));
#26524=CARTESIAN_POINT('Ctrl Pts',(30.333388412875,-32.0014707790079,169.97851963661));
#26525=CARTESIAN_POINT('Ctrl Pts',(30.3365390411281,-32.0005076151419,170.17148036339));
#26526=CARTESIAN_POINT('Ctrl Pts',(30.3358657202362,-32.2469827843609,170.187902459474));
#26527=CARTESIAN_POINT('Ctrl Pts',(30.3871296120999,-32.4931916071125,170.204324555558));
#26528=CARTESIAN_POINT('Ctrl Pts',(30.4917453489521,-32.7141390229613,170.220746651642));
#26529=CARTESIAN_POINT('Ctrl Pts',(30.7277266903134,-33.2125293142421,170.257789914715));
#26530=CARTESIAN_POINT('Ctrl Pts',(31.2351710894949,-33.5823853671255,170.294833177788));
#26531=CARTESIAN_POINT('Ctrl Pts',(31.7818747409338,-33.654463057273,170.331876440861));
#26532=CARTESIAN_POINT('Ctrl Pts',(32.3285783923727,-33.7265407474205,170.368919703935));
#26533=CARTESIAN_POINT('Ctrl Pts',(32.9145412960691,-33.500840074832,170.405962967008));
#26534=CARTESIAN_POINT('Ctrl Pts',(33.271630004543,-33.0806404434732,170.443006230081));
#26535=CARTESIAN_POINT('Ctrl Pts',(33.6287187130169,-32.6604408121143,170.480049493154));
#26536=CARTESIAN_POINT('Ctrl Pts',(33.7569332262683,-32.0457422219851,170.517092756228));
#26537=CARTESIAN_POINT('Ctrl Pts',(33.5976032782476,-31.5178274148643,170.554136019301));
#26538=CARTESIAN_POINT('Ctrl Pts',(33.4382733302269,-30.9899126077435,170.591179282374));
#26539=CARTESIAN_POINT('Ctrl Pts',(32.9913989209342,-30.5487815836311,170.628222545447));
#26540=CARTESIAN_POINT('Ctrl Pts',(32.4614673569861,-30.3962935072277,170.665265808521));
#26541=CARTESIAN_POINT('Ctrl Pts',(31.9315357930381,-30.2438054308242,170.702309071594));
#26542=CARTESIAN_POINT('Ctrl Pts',(31.3185470744347,-30.3799603021296,170.739352334667));
#26543=CARTESIAN_POINT('Ctrl Pts',(30.9030015150161,-30.7424543903036,170.77639559774));
#26544=CARTESIAN_POINT('Ctrl Pts',(30.5474528146032,-31.0526112408253,170.808090519624));
#26545=CARTESIAN_POINT('Ctrl Pts',(30.3364490867416,-31.5284674046311,170.839785441507));
#26546=CARTESIAN_POINT('Ctrl Pts',(30.3325051052426,-32.0012453678659,170.87148036339));
#26547=CARTESIAN_POINT('Origin',(32.,-32.,172.));
#26548=CARTESIAN_POINT('',(30.3326609344046,-31.9986999066702,171.57148036339));
#26549=CARTESIAN_POINT('',(30.3362279033014,-31.9991286353279,171.37851963661));
#26550=CARTESIAN_POINT('',(30.334,-32.,172.));
#26551=CARTESIAN_POINT('Ctrl Pts',(30.3362279033014,-31.9991286353279,171.37851963661));
#26552=CARTESIAN_POINT('Ctrl Pts',(30.3351774875366,-31.7776543086145,171.363756385256));
#26553=CARTESIAN_POINT('Ctrl Pts',(30.3762757945419,-31.55655399107,171.348993133901));
#26554=CARTESIAN_POINT('Ctrl Pts',(30.4613605091736,-31.3539236136619,171.334229882547));
#26555=CARTESIAN_POINT('Ctrl Pts',(30.674851114459,-30.8454929030546,171.297186619474));
#26556=CARTESIAN_POINT('Ctrl Pts',(31.1652735898184,-30.4533461842114,171.2601433564));
#26557=CARTESIAN_POINT('Ctrl Pts',(31.7082132697327,-30.356927669348,171.223100093327));
#26558=CARTESIAN_POINT('Ctrl Pts',(32.2511529496469,-30.2605091544846,171.186056830254));
#26559=CARTESIAN_POINT('Ctrl Pts',(32.8466098341158,-30.4598188436011,171.149013567181));
#26560=CARTESIAN_POINT('Ctrl Pts',(33.222106081537,-30.8636537036694,171.111970304107));
#26561=CARTESIAN_POINT('Ctrl Pts',(33.5976023289583,-31.2674885637377,171.074927041034));
#26562=CARTESIAN_POINT('Ctrl Pts',(33.7531379393318,-31.8758485947579,171.037883777961));
#26563=CARTESIAN_POINT('Ctrl Pts',(33.6175406607073,-32.41035154523,171.000840514888));
#26564=CARTESIAN_POINT('Ctrl Pts',(33.4819433820829,-32.9448544957022,170.963797251814));
#26565=CARTESIAN_POINT('Ctrl Pts',(33.0552132144606,-33.4055003656264,170.926753988741));
#26566=CARTESIAN_POINT('Ctrl Pts',(32.5326195686963,-33.5815001026734,170.889710725668));
#26567=CARTESIAN_POINT('Ctrl Pts',(32.010025922932,-33.7574998397204,170.852667462595));
#26568=CARTESIAN_POINT('Ctrl Pts',(31.3915687990259,-33.6488534438904,170.815624199522));
#26569=CARTESIAN_POINT('Ctrl Pts',(30.9602508234331,-33.3052769168045,170.778580936448));
#26570=CARTESIAN_POINT('Ctrl Pts',(30.5718919721791,-32.9959204954925,170.745227169836));
#26571=CARTESIAN_POINT('Ctrl Pts',(30.3352507152854,-32.4961013373448,170.711873403223));
#26572=CARTESIAN_POINT('Ctrl Pts',(30.3318905468311,-31.9990590648467,170.67851963661));
#26573=CARTESIAN_POINT('Ctrl Pts',(30.3325051052426,-32.0012453678659,170.87148036339));
#26574=CARTESIAN_POINT('Ctrl Pts',(30.3318395803745,-32.0810240107588,170.87682870458));
#26575=CARTESIAN_POINT('Ctrl Pts',(30.3370700153316,-32.1607150028783,170.88217704577));
#26576=CARTESIAN_POINT('Ctrl Pts',(30.3484967900501,-32.2395073778593,170.88752538696));
#26577=CARTESIAN_POINT('Ctrl Pts',(30.4276400247368,-32.7852329721987,170.924568650033));
#26578=CARTESIAN_POINT('Ctrl Pts',(30.8040288943443,-33.2878508558347,170.961611913106));
#26579=CARTESIAN_POINT('Ctrl Pts',(31.3054298930238,-33.5173658105477,170.99865517618));
#26580=CARTESIAN_POINT('Ctrl Pts',(31.8068308917033,-33.7468807652606,171.035698439253));
#26581=CARTESIAN_POINT('Ctrl Pts',(32.4332440194548,-33.7032927910504,171.072741702326));
#26582=CARTESIAN_POINT('Ctrl Pts',(32.8980260256029,-33.4065475085697,171.109784965399));
#26583=CARTESIAN_POINT('Ctrl Pts',(33.3628080317511,-33.109802226089,171.146828228473));
#26584=CARTESIAN_POINT('Ctrl Pts',(33.665958916296,-32.5598996353379,171.183871491546));
#26585=CARTESIAN_POINT('Ctrl Pts',(33.668758478237,-32.0084721801214,171.220914754619));
#26586=CARTESIAN_POINT('Ctrl Pts',(33.671558040178,-31.4570447249048,171.257958017692));
#26587=CARTESIAN_POINT('Ctrl Pts',(33.3740062795152,-30.9040924052229,171.295001280766));
#26588=CARTESIAN_POINT('Ctrl Pts',(32.9122612685207,-30.6026432043029,171.332044543839));
#26589=CARTESIAN_POINT('Ctrl Pts',(32.4505162575261,-30.3011940033829,171.369087806912));
#26590=CARTESIAN_POINT('Ctrl Pts',(31.8245779961998,-30.2512479212249,171.406131069985));
#26591=CARTESIAN_POINT('Ctrl Pts',(31.3208724389158,-30.475660014203,171.443174333059));
#26592=CARTESIAN_POINT('Ctrl Pts',(30.8171668816317,-30.7000721071811,171.480217596132));
#26593=CARTESIAN_POINT('Ctrl Pts',(30.4356940283899,-31.1988423752953,171.517260859205));
#26594=CARTESIAN_POINT('Ctrl Pts',(30.3510137883834,-31.7437362483257,171.554304122278));
#26595=CARTESIAN_POINT('Ctrl Pts',(30.3379255945698,-31.8279551477702,171.560029535982));
#26596=CARTESIAN_POINT('Ctrl Pts',(30.331927435482,-31.9132758871728,171.565754949686));
#26597=CARTESIAN_POINT('Ctrl Pts',(30.3326609344046,-31.9986999066702,171.57148036339));
#26598=CARTESIAN_POINT('Origin',(32.,-32.,172.));
#26599=CARTESIAN_POINT('',(30.3365860588666,-31.9995809884575,172.27148036339));
#26600=CARTESIAN_POINT('',(30.3350677693052,-32.0014151633937,172.07851963661));
#26601=CARTESIAN_POINT('',(30.334,-32.,172.));
#26602=CARTESIAN_POINT('Ctrl Pts',(30.3350677693052,-32.0014151633937,172.07851963661));
#26603=CARTESIAN_POINT('Ctrl Pts',(30.3381925394303,-31.6144945028862,172.052682630362));
#26604=CARTESIAN_POINT('Ctrl Pts',(30.4725557471307,-31.2256167628786,172.026845624113));
#26605=CARTESIAN_POINT('Ctrl Pts',(30.7190757093515,-30.9303929967783,172.001008617865));
#26606=CARTESIAN_POINT('Ctrl Pts',(31.0725185086303,-30.5071221453465,171.963965354792));
#26607=CARTESIAN_POINT('Ctrl Pts',(31.6565083342578,-30.2763644000794,171.926922091719));
#26608=CARTESIAN_POINT('Ctrl Pts',(32.2038146085797,-30.3437132539793,171.889878828646));
#26609=CARTESIAN_POINT('Ctrl Pts',(32.7511208829017,-30.4110621078793,171.852835565572));
#26610=CARTESIAN_POINT('Ctrl Pts',(33.2617436059181,-30.7765175609463,171.815792302499));
#26611=CARTESIAN_POINT('Ctrl Pts',(33.5020245883132,-31.2728491794567,171.778749039426));
#26612=CARTESIAN_POINT('Ctrl Pts',(33.7423055707082,-31.769180797967,171.741705776352));
#26613=CARTESIAN_POINT('Ctrl Pts',(33.7122448124818,-32.3963885819206,171.704662513279));
#26614=CARTESIAN_POINT('Ctrl Pts',(33.4255979536008,-32.867465650273,171.667619250206));
#26615=CARTESIAN_POINT('Ctrl Pts',(33.1389510947197,-33.3385427186253,171.630575987133));
#26616=CARTESIAN_POINT('Ctrl Pts',(32.595718135184,-33.6534890713764,171.59353272406));
#26617=CARTESIAN_POINT('Ctrl Pts',(32.044479531719,-33.6681869652327,171.556489460986));
#26618=CARTESIAN_POINT('Ctrl Pts',(31.493240928254,-33.6828848590891,171.519446197913));
#26619=CARTESIAN_POINT('Ctrl Pts',(30.9339966808599,-33.3973342940507,171.48240293484));
#26620=CARTESIAN_POINT('Ctrl Pts',(30.6226539247684,-32.9422016603458,171.445359671767));
#26621=CARTESIAN_POINT('Ctrl Pts',(30.43539395686,-32.6684579463388,171.423079660048));
#26622=CARTESIAN_POINT('Ctrl Pts',(30.3378131418771,-32.3333673796386,171.400799648329));
#26623=CARTESIAN_POINT('Ctrl Pts',(30.3362279033014,-31.9991286353279,171.37851963661));
#26624=CARTESIAN_POINT('Ctrl Pts',(30.3326609344046,-31.9986999066702,171.57148036339));
#26625=CARTESIAN_POINT('Ctrl Pts',(30.3366731525528,-32.4659668525121,171.60279821276));
#26626=CARTESIAN_POINT('Ctrl Pts',(30.5421005326414,-32.9363239994605,171.634116062129));
#26627=CARTESIAN_POINT('Ctrl Pts',(30.8902894362117,-33.2463422889161,171.665433911498));
#26628=CARTESIAN_POINT('Ctrl Pts',(31.3021329508178,-33.6130369785294,171.702477174571));
#26629=CARTESIAN_POINT('Ctrl Pts',(31.9137076068011,-33.7554088798094,171.739520437644));
#26630=CARTESIAN_POINT('Ctrl Pts',(32.4451601577091,-33.6083093827098,171.776563700718));
#26631=CARTESIAN_POINT('Ctrl Pts',(32.9766127086172,-33.4612098856102,171.813606963791));
#26632=CARTESIAN_POINT('Ctrl Pts',(33.42794315445,-33.024638990131,171.850650226864));
#26633=CARTESIAN_POINT('Ctrl Pts',(33.592625130432,-32.4983691708365,171.887693489937));
#26634=CARTESIAN_POINT('Ctrl Pts',(33.757307106414,-31.9720993515419,171.924736753011));
#26635=CARTESIAN_POINT('Ctrl Pts',(33.6353406125451,-31.3561306084319,171.961780016084));
#26636=CARTESIAN_POINT('Ctrl Pts',(33.2825368550839,-30.9323268984023,171.998823279157));
#26637=CARTESIAN_POINT('Ctrl Pts',(32.9297330976227,-30.5085231883726,172.035866542231));
#26638=CARTESIAN_POINT('Ctrl Pts',(32.3460920765693,-30.2768845114231,172.072909805304));
#26639=CARTESIAN_POINT('Ctrl Pts',(31.798684758496,-30.3434074701176,172.109953068377));
#26640=CARTESIAN_POINT('Ctrl Pts',(31.2512774404227,-30.4099304288121,172.14699633145));
#26641=CARTESIAN_POINT('Ctrl Pts',(30.7401038253296,-30.7746150231505,172.184039594523));
#26642=CARTESIAN_POINT('Ctrl Pts',(30.4990741877597,-31.2705835601835,172.221082857597));
#26643=CARTESIAN_POINT('Ctrl Pts',(30.3897669296326,-31.4955059450278,172.237882026195));
#26644=CARTESIAN_POINT('Ctrl Pts',(30.3360184124935,-31.7474286377632,172.254681194792));
#26645=CARTESIAN_POINT('Ctrl Pts',(30.3365860588666,-31.9995809884575,172.27148036339));
#26646=CARTESIAN_POINT('Origin',(32.,-32.,172.));
#26647=CARTESIAN_POINT('',(30.3341968407374,-32.0015218483092,172.97148036339));
#26648=CARTESIAN_POINT('',(30.3312207903893,-32.00003685081,172.77851963661));
#26649=CARTESIAN_POINT('',(30.334,-32.,172.));
#26650=CARTESIAN_POINT('Ctrl Pts',(30.3312211840313,-32.0000368455905,172.77851963661));
#26651=CARTESIAN_POINT('Ctrl Pts',(30.3313999767094,-31.4505738647218,172.741608875468));
#26652=CARTESIAN_POINT('Ctrl Pts',(30.6293022634182,-30.9009447454105,172.704698114326));
#26653=CARTESIAN_POINT('Ctrl Pts',(31.0898482998377,-30.6012684094488,172.667787353184));
#26654=CARTESIAN_POINT('Ctrl Pts',(31.552047600436,-30.3005162979679,172.63074409011));
#26655=CARTESIAN_POINT('Ctrl Pts',(32.1780604609226,-30.2515147475589,172.593700827037));
#26656=CARTESIAN_POINT('Ctrl Pts',(32.6814267907523,-30.4766866019892,172.556657563964));
#26657=CARTESIAN_POINT('Ctrl Pts',(33.184793120582,-30.7018584564195,172.519614300891));
#26658=CARTESIAN_POINT('Ctrl Pts',(33.5655129197548,-31.2012037156891,172.482571037817));
#26659=CARTESIAN_POINT('Ctrl Pts',(33.6493708725363,-31.7462246967432,172.445527774744));
#26660=CARTESIAN_POINT('Ctrl Pts',(33.7332288253178,-32.2912456777972,172.408484511671));
#26661=CARTESIAN_POINT('Ctrl Pts',(33.520224931708,-32.8819423806357,172.371441248598));
#26662=CARTESIAN_POINT('Ctrl Pts',(33.1078286184573,-33.2480151969592,172.334397985524));
#26663=CARTESIAN_POINT('Ctrl Pts',(32.6954323052066,-33.6140880132827,172.297354722451));
#26664=CARTESIAN_POINT('Ctrl Pts',(32.083643572315,-33.7555369430913,172.260311459378));
#26665=CARTESIAN_POINT('Ctrl Pts',(31.5524136266673,-33.6076357230794,172.223268196305));
#26666=CARTESIAN_POINT('Ctrl Pts',(31.0211836810197,-33.4597345030675,172.186224933231));
#26667=CARTESIAN_POINT('Ctrl Pts',(30.570512522616,-33.0224831332352,172.149181670158));
#26668=CARTESIAN_POINT('Ctrl Pts',(30.4066248298793,-32.4959654695208,172.112138407085));
#26669=CARTESIAN_POINT('Ctrl Pts',(30.3570458397229,-32.3366843567626,172.10093215026));
#26670=CARTESIAN_POINT('Ctrl Pts',(30.3337124661325,-32.1692338437356,172.089725893435));
#26671=CARTESIAN_POINT('Ctrl Pts',(30.3350677693052,-32.0014151633937,172.07851963661));
#26672=CARTESIAN_POINT('Ctrl Pts',(30.3365860588666,-31.9995809884575,172.27148036339));
#26673=CARTESIAN_POINT('Ctrl Pts',(30.3372701097908,-32.303441026525,172.291724457866));
#26674=CARTESIAN_POINT('Ctrl Pts',(30.4168311309414,-32.6076345698113,172.311968552341));
#26675=CARTESIAN_POINT('Ctrl Pts',(30.573094643523,-32.8653136657775,172.332212646816));
#26676=CARTESIAN_POINT('Ctrl Pts',(30.8590303969029,-33.3368227546111,172.36925590989));
#26677=CARTESIAN_POINT('Ctrl Pts',(31.4017875637094,-33.6525884525509,172.406299172963));
#26678=CARTESIAN_POINT('Ctrl Pts',(31.9530034073899,-33.6681180883879,172.443342436036));
#26679=CARTESIAN_POINT('Ctrl Pts',(32.5042192510704,-33.6836477242249,172.480385699109));
#26680=CARTESIAN_POINT('Ctrl Pts',(33.063893771625,-33.3989412979589,172.517428962183));
#26681=CARTESIAN_POINT('Ctrl Pts',(33.3759229431567,-32.9442789264931,172.554472225256));
#26682=CARTESIAN_POINT('Ctrl Pts',(33.6879521146883,-32.4896165550273,172.591515488329));
#26683=CARTESIAN_POINT('Ctrl Pts',(33.752335937197,-31.8649982383616,172.628558751402));
#26684=CARTESIAN_POINT('Ctrl Pts',(33.5396127226094,-31.3562459313504,172.665602014476));
#26685=CARTESIAN_POINT('Ctrl Pts',(33.3268895080219,-30.8474936243392,172.702645277549));
#26686=CARTESIAN_POINT('Ctrl Pts',(32.8370592563382,-30.4546073269825,172.739688540622));
#26687=CARTESIAN_POINT('Ctrl Pts',(32.2942656347348,-30.3573696786136,172.776731803695));
#26688=CARTESIAN_POINT('Ctrl Pts',(31.7514720131314,-30.2601320302447,172.813775066769));
#26689=CARTESIAN_POINT('Ctrl Pts',(31.1557150216083,-30.4585430308634,172.850818329842));
#26690=CARTESIAN_POINT('Ctrl Pts',(30.7796098291288,-30.8618108824256,172.887861592915));
#26691=CARTESIAN_POINT('Ctrl Pts',(30.4966123179727,-31.1652467312342,172.915734516407));
#26692=CARTESIAN_POINT('Ctrl Pts',(30.3379749857601,-31.5846663086172,172.943607439899));
#26693=CARTESIAN_POINT('Ctrl Pts',(30.3341968407374,-32.0015218483092,172.97148036339));
#26694=CARTESIAN_POINT('Origin',(32.,-32.,172.));
#26695=CARTESIAN_POINT('',(30.3314156322217,-31.9994831966126,173.67148036339));
#26696=CARTESIAN_POINT('',(30.3349604002087,-31.9985615026093,173.47851963661));
#26697=CARTESIAN_POINT('',(30.334,-32.,172.));
#26698=CARTESIAN_POINT('Ctrl Pts',(30.3349604002087,-31.9985615026093,173.47851963661));
#26699=CARTESIAN_POINT('Ctrl Pts',(30.3336089830085,-31.8347381058788,173.467578383647));
#26700=CARTESIAN_POINT('Ctrl Pts',(30.3558306375885,-31.6712733228841,173.456637130684));
#26701=CARTESIAN_POINT('Ctrl Pts',(30.4031262159285,-31.515417398724,173.445695877722));
#26702=CARTESIAN_POINT('Ctrl Pts',(30.5632525338761,-30.9877436469281,173.408652614648));
#26703=CARTESIAN_POINT('Ctrl Pts',(31.0107920151616,-30.5472874446471,173.371609351575));
#26704=CARTESIAN_POINT('Ctrl Pts',(31.5409530198307,-30.3955991617705,173.334566088502));
#26705=CARTESIAN_POINT('Ctrl Pts',(32.0711140244998,-30.2439108788938,173.297522825429));
#26706=CARTESIAN_POINT('Ctrl Pts',(32.6838965525525,-30.3809905154216,173.260479562355));
#26707=CARTESIAN_POINT('Ctrl Pts',(33.0988946418266,-30.744111172962,173.223436299282));
#26708=CARTESIAN_POINT('Ctrl Pts',(33.5138927311008,-31.1072318305024,173.186393036209));
#26709=CARTESIAN_POINT('Ctrl Pts',(33.7311063815966,-31.6963935090555,173.149349773136));
#26710=CARTESIAN_POINT('Ctrl Pts',(33.651139804639,-32.2419990191115,173.112306510063));
#26711=CARTESIAN_POINT('Ctrl Pts',(33.5711732276814,-32.7876045291676,173.075263246989));
#26712=CARTESIAN_POINT('Ctrl Pts',(33.1940264232705,-33.2896538707265,173.038219983916));
#26713=CARTESIAN_POINT('Ctrl Pts',(32.6922797241113,-33.5184119873403,173.001176720843));
#26714=CARTESIAN_POINT('Ctrl Pts',(32.1905330249521,-33.747170103954,172.964133457769));
#26715=CARTESIAN_POINT('Ctrl Pts',(31.5641864310446,-33.7026369956225,172.927090194696));
#26716=CARTESIAN_POINT('Ctrl Pts',(31.0998527475379,-33.4051907712475,172.890046931623));
#26717=CARTESIAN_POINT('Ctrl Pts',(30.6355190640312,-33.1077445468725,172.85300366855));
#26718=CARTESIAN_POINT('Ctrl Pts',(30.3331982909253,-32.5573852064541,172.815960405477));
#26719=CARTESIAN_POINT('Ctrl Pts',(30.3312307747274,-32.0059541999684,172.778917142403));
#26720=CARTESIAN_POINT('Ctrl Pts',(30.3312237370187,-32.0039817583638,172.778784640472));
#26721=CARTESIAN_POINT('Ctrl Pts',(30.3312205422029,-32.0020093030476,172.778652138541));
#26722=CARTESIAN_POINT('Ctrl Pts',(30.3312211840313,-32.0000368455905,172.77851963661));
#26723=CARTESIAN_POINT('Ctrl Pts',(30.3341968407374,-32.0015218483092,172.97148036339));
#26724=CARTESIAN_POINT('Ctrl Pts',(30.3329538109971,-32.1386695305945,172.980650702972));
#26725=CARTESIAN_POINT('Ctrl Pts',(30.3484734346937,-32.2755396699326,172.989821042553));
#26726=CARTESIAN_POINT('Ctrl Pts',(30.3818418733238,-32.4079104234947,172.998991382135));
#26727=CARTESIAN_POINT('Ctrl Pts',(30.5166325034344,-32.942617410496,173.036034645208));
#26728=CARTESIAN_POINT('Ctrl Pts',(30.9426671570916,-33.4039066819931,173.073077908281));
#26729=CARTESIAN_POINT('Ctrl Pts',(31.4649946868587,-33.5806947685858,173.110121171354));
#26730=CARTESIAN_POINT('Ctrl Pts',(31.9873222166257,-33.7574828551785,173.147164434428));
#26731=CARTESIAN_POINT('Ctrl Pts',(32.6059426225026,-33.6497697568668,173.184207697501));
#26732=CARTESIAN_POINT('Ctrl Pts',(33.0377785610895,-33.3068444033881,173.221250960574));
#26733=CARTESIAN_POINT('Ctrl Pts',(33.4696144996764,-32.9639190499095,173.258294223647));
#26734=CARTESIAN_POINT('Ctrl Pts',(33.7146659709733,-32.3857814412639,173.295337486721));
#26735=CARTESIAN_POINT('Ctrl Pts',(33.660798750451,-31.8369842123471,173.332380749794));
#26736=CARTESIAN_POINT('Ctrl Pts',(33.6069315299288,-31.2881869834302,173.369424012867));
#26737=CARTESIAN_POINT('Ctrl Pts',(33.2541456175874,-30.7687301342419,173.40646727594));
#26738=CARTESIAN_POINT('Ctrl Pts',(32.7638739340123,-30.5163143023334,173.443510539014));
#26739=CARTESIAN_POINT('Ctrl Pts',(32.2736022504372,-30.2638984704248,173.480553802087));
#26740=CARTESIAN_POINT('Ctrl Pts',(31.6458447956283,-30.278523655796,173.51759706516));
#26741=CARTESIAN_POINT('Ctrl Pts',(31.1678599770333,-30.5534974529228,173.554640328233));
#26742=CARTESIAN_POINT('Ctrl Pts',(30.6898751584383,-30.8284712500496,173.591683591307));
#26743=CARTESIAN_POINT('Ctrl Pts',(30.361662976057,-31.363793658932,173.62872685438));
#26744=CARTESIAN_POINT('Ctrl Pts',(30.3334115448907,-31.9145040479303,173.665770117453));
#26745=CARTESIAN_POINT('Ctrl Pts',(30.3319598853387,-31.9428015168934,173.667673532765));
#26746=CARTESIAN_POINT('Ctrl Pts',(30.3313002037148,-31.9711396143072,173.669576948078));
#26747=CARTESIAN_POINT('Ctrl Pts',(30.3314156322217,-31.9994831966126,173.67148036339));
#26748=CARTESIAN_POINT('Origin',(32.,-32.,172.));
#26749=CARTESIAN_POINT('',(30.3357186087607,-31.9988063447514,174.37148036339));
#26750=CARTESIAN_POINT('',(30.3362886687534,-32.0008167340388,174.17851963661));
#26751=CARTESIAN_POINT('',(30.334,-32.,172.));
#26752=CARTESIAN_POINT('Ctrl Pts',(30.3362886687534,-32.0008167340388,174.17851963661));
#26753=CARTESIAN_POINT('Ctrl Pts',(30.3377536779545,-31.6705233147409,174.156504628753));
#26754=CARTESIAN_POINT('Ctrl Pts',(30.4328677375841,-31.3394522335906,174.134489620897));
#26755=CARTESIAN_POINT('Ctrl Pts',(30.6159654927621,-31.067650997486,174.11247461304));
#26756=CARTESIAN_POINT('Ctrl Pts',(30.9240525194557,-30.6103082266709,174.075431349967));
#26757=CARTESIAN_POINT('Ctrl Pts',(31.481244854197,-30.3207741949187,174.038388086894));
#26758=CARTESIAN_POINT('Ctrl Pts',(32.0325743058579,-30.3315381052262,174.00134482382));
#26759=CARTESIAN_POINT('Ctrl Pts',(32.5839037575188,-30.3423020155338,173.964301560747));
#26760=CARTESIAN_POINT('Ctrl Pts',(33.1293703260993,-30.6533638679011,173.927258297674));
#26761=CARTESIAN_POINT('Ctrl Pts',(33.4193714674863,-31.1223834453475,173.8902150346));
#26762=CARTESIAN_POINT('Ctrl Pts',(33.7093726088733,-31.591403022794,173.853171771527));
#26763=CARTESIAN_POINT('Ctrl Pts',(33.7439083230667,-32.2183803253196,173.816128508454));
#26764=CARTESIAN_POINT('Ctrl Pts',(33.5071752545138,-32.7164139389316,173.779085245381));
#26765=CARTESIAN_POINT('Ctrl Pts',(33.2704421859609,-33.2144475525435,173.742041982308));
#26766=CARTESIAN_POINT('Ctrl Pts',(32.7624403346617,-33.5835374772417,173.704998719234));
#26767=CARTESIAN_POINT('Ctrl Pts',(32.2156285932453,-33.6547901647911,173.667955456161));
#26768=CARTESIAN_POINT('Ctrl Pts',(31.668816851829,-33.7260428523404,173.630912193088));
#26769=CARTESIAN_POINT('Ctrl Pts',(31.0831952202954,-33.499458302741,173.593868930015));
#26770=CARTESIAN_POINT('Ctrl Pts',(30.7267409818334,-33.0787203772859,173.556825666941));
#26771=CARTESIAN_POINT('Ctrl Pts',(30.4755705566504,-32.7822533635026,173.530723656831));
#26772=CARTESIAN_POINT('Ctrl Pts',(30.3381844098851,-32.3893869384504,173.50462164672));
#26773=CARTESIAN_POINT('Ctrl Pts',(30.3349604002087,-31.9985615026093,173.47851963661));
#26774=CARTESIAN_POINT('Ctrl Pts',(30.3314156322217,-31.9994831966126,173.67148036339));
#26775=CARTESIAN_POINT('Ctrl Pts',(30.3335466123253,-32.5227474368098,173.706620211151));
#26776=CARTESIAN_POINT('Ctrl Pts',(30.5998552268592,-33.0478810703266,173.741760058912));
#26777=CARTESIAN_POINT('Ctrl Pts',(31.0242067934649,-33.353755611107,173.776899906673));
#26778=CARTESIAN_POINT('Ctrl Pts',(31.4715441531567,-33.6761984161711,173.813943169746));
#26779=CARTESIAN_POINT('Ctrl Pts',(32.0945095524917,-33.7549856571851,173.850986432819));
#26780=CARTESIAN_POINT('Ctrl Pts',(32.6080374026233,-33.5540647198669,173.888029695893));
#26781=CARTESIAN_POINT('Ctrl Pts',(33.121565252755,-33.3531437825487,173.925072958966));
#26782=CARTESIAN_POINT('Ctrl Pts',(33.5256555536833,-32.8725146668984,173.962116222039));
#26783=CARTESIAN_POINT('Ctrl Pts',(33.6353987747919,-32.3321106501347,173.999159485112));
#26784=CARTESIAN_POINT('Ctrl Pts',(33.7451419959006,-31.7917066333709,174.036202748186));
#26785=CARTESIAN_POINT('Ctrl Pts',(33.5605381371895,-31.1915277154938,174.073246011259));
#26786=CARTESIAN_POINT('Ctrl Pts',(33.1660609234322,-30.8062125149892,174.110289274332));
#26787=CARTESIAN_POINT('Ctrl Pts',(32.7715837096748,-30.4208973144846,174.147332537405));
#26788=CARTESIAN_POINT('Ctrl Pts',(32.1672331408712,-30.2504458313525,174.184375800479));
#26789=CARTESIAN_POINT('Ctrl Pts',(31.6295567603514,-30.3728557400395,174.221419063552));
#26790=CARTESIAN_POINT('Ctrl Pts',(31.0918803798316,-30.4952656487264,174.258462326625));
#26791=CARTESIAN_POINT('Ctrl Pts',(30.6208781875955,-30.9105369492325,174.295505589698));
#26792=CARTESIAN_POINT('Ctrl Pts',(30.4320782329074,-31.4286437461609,174.332548852772));
#26793=CARTESIAN_POINT('Ctrl Pts',(30.365936944488,-31.6101493569238,174.345526022978));
#26794=CARTESIAN_POINT('Ctrl Pts',(30.3344296026448,-31.8042757006765,174.358503193184));
#26795=CARTESIAN_POINT('Ctrl Pts',(30.3357186087607,-31.9988063447514,174.37148036339));
#26796=CARTESIAN_POINT('Origin',(32.,-32.,172.));
#26797=CARTESIAN_POINT('',(30.3357236107064,-32.0011913006864,175.07148036339));
#26798=CARTESIAN_POINT('',(30.3319794150682,-32.0009960690673,174.87851963661));
#26799=CARTESIAN_POINT('',(30.334,-32.,172.));
#26800=CARTESIAN_POINT('Ctrl Pts',(30.3319794150682,-32.0009960690673,174.87851963661));
#26801=CARTESIAN_POINT('Ctrl Pts',(30.3354661857311,-31.5078338077314,174.845430873859));
#26802=CARTESIAN_POINT('Ctrl Pts',(30.5678894861827,-31.0118158958362,174.812342111109));
#26803=CARTESIAN_POINT('Ctrl Pts',(30.9509629101096,-30.7021759118631,174.779253348358));
#26804=CARTESIAN_POINT('Ctrl Pts',(31.3798181600293,-30.3555302705375,174.742210085285));
#26805=CARTESIAN_POINT('Ctrl Pts',(31.9974842423841,-30.2424733638685,174.705166822212));
#26806=CARTESIAN_POINT('Ctrl Pts',(32.5213205070434,-30.4147394193224,174.668123559139));
#26807=CARTESIAN_POINT('Ctrl Pts',(33.0451567717027,-30.5870054747763,174.631080296065));
#26808=CARTESIAN_POINT('Ctrl Pts',(33.4751632186663,-31.0445944923531,174.594037032992));
#26809=CARTESIAN_POINT('Ctrl Pts',(33.6145712294167,-31.5781162187827,174.556993769919));
#26810=CARTESIAN_POINT('Ctrl Pts',(33.753979240167,-32.1116379452123,174.519950506846));
#26811=CARTESIAN_POINT('Ctrl Pts',(33.602788814704,-32.7210923804948,174.482907243772));
#26812=CARTESIAN_POINT('Ctrl Pts',(33.2301838719237,-33.127596479674,174.445863980699));
#26813=CARTESIAN_POINT('Ctrl Pts',(32.8575789291433,-33.5341005788531,174.408820717626));
#26814=CARTESIAN_POINT('Ctrl Pts',(32.2635594690455,-33.7376543419289,174.371777454553));
#26815=CARTESIAN_POINT('Ctrl Pts',(31.7199455756347,-33.6451126706422,174.334734191479));
#26816=CARTESIAN_POINT('Ctrl Pts',(31.1763316822239,-33.5525709993555,174.297690928406));
#26817=CARTESIAN_POINT('Ctrl Pts',(30.6831233555,-33.1639338937063,174.260647665333));
#26818=CARTESIAN_POINT('Ctrl Pts',(30.4660100514611,-32.6570395859427,174.22360440226));
#26819=CARTESIAN_POINT('Ctrl Pts',(30.377928336371,-32.4513952556937,174.208576147043));
#26820=CARTESIAN_POINT('Ctrl Pts',(30.3352885995137,-32.2262871873733,174.193547891827));
#26821=CARTESIAN_POINT('Ctrl Pts',(30.3362886687534,-32.0008167340388,174.17851963661));
#26822=CARTESIAN_POINT('Ctrl Pts',(30.3357186087607,-31.9988063447514,174.37148036339));
#26823=CARTESIAN_POINT('Ctrl Pts',(30.3381090637209,-32.359562385658,174.395546456257));
#26824=CARTESIAN_POINT('Ctrl Pts',(30.4532910934898,-32.7217088761992,174.419612549124));
#26825=CARTESIAN_POINT('Ctrl Pts',(30.669544703303,-33.0073307996953,174.443678641991));
#26826=CARTESIAN_POINT('Ctrl Pts',(31.0024088455269,-33.4469687629505,174.480721905064));
#26827=CARTESIAN_POINT('Ctrl Pts',(31.5747348471149,-33.7053023961102,174.517765168138));
#26828=CARTESIAN_POINT('Ctrl Pts',(32.1246294330488,-33.6641196293962,174.554808431211));
#26829=CARTESIAN_POINT('Ctrl Pts',(32.6745240189827,-33.6229368626822,174.591851694284));
#26830=CARTESIAN_POINT('Ctrl Pts',(33.2019871892626,-33.2822376960947,174.628894957357));
#26831=CARTESIAN_POINT('Ctrl Pts',(33.4656546572183,-32.7979242208996,174.665938220431));
#26832=CARTESIAN_POINT('Ctrl Pts',(33.7293221251739,-32.3136107457046,174.702981483504));
#26833=CARTESIAN_POINT('Ctrl Pts',(33.7291938908055,-31.6856829619021,174.740024746577));
#26834=CARTESIAN_POINT('Ctrl Pts',(33.4653286334645,-31.2014772185636,174.77706800965));
#26835=CARTESIAN_POINT('Ctrl Pts',(33.2014633761235,-30.717271475225,174.814111272724));
#26836=CARTESIAN_POINT('Ctrl Pts',(32.6738610958101,-30.3767877723504,174.851154535797));
#26837=CARTESIAN_POINT('Ctrl Pts',(32.1239497351913,-30.3358296061791,174.88819779887));
#26838=CARTESIAN_POINT('Ctrl Pts',(31.5740383745726,-30.2948714400079,174.925241061943));
#26839=CARTESIAN_POINT('Ctrl Pts',(31.0018179336486,-30.55343881054,174.962284325017));
#26840=CARTESIAN_POINT('Ctrl Pts',(30.66913338345,-30.9932126910432,174.99932758809));
#26841=CARTESIAN_POINT('Ctrl Pts',(30.4531326714452,-31.2787428464203,175.02337851319));
#26842=CARTESIAN_POINT('Ctrl Pts',(30.3381073856001,-31.6406599036176,175.04742943829));
#26843=CARTESIAN_POINT('Ctrl Pts',(30.3357236107064,-32.0011913006864,175.07148036339));
#26844=CARTESIAN_POINT('Origin',(32.,-32.,172.));
#26845=CARTESIAN_POINT('',(30.3314186128286,-32.0005207267479,175.77148036339));
#26846=CARTESIAN_POINT('',(30.3332691019313,-31.9985486152772,175.57851963661));
#26847=CARTESIAN_POINT('',(30.334,-32.,172.));
#26848=CARTESIAN_POINT('Ctrl Pts',(30.3332691019313,-31.9985486152772,175.57851963661));
#26849=CARTESIAN_POINT('Ctrl Pts',(30.3322968352458,-31.8922279885927,175.571400382039));
#26850=CARTESIAN_POINT('Ctrl Pts',(30.3415987887235,-31.7860768352642,175.564281127468));
#26851=CARTESIAN_POINT('Ctrl Pts',(30.3617914430141,-31.6820394623037,175.557161872896));
#26852=CARTESIAN_POINT('Ctrl Pts',(30.4668588763472,-31.1407069762228,175.520118609823));
#26853=CARTESIAN_POINT('Ctrl Pts',(30.8667791078583,-30.6566025847272,175.48307534675));
#26854=CARTESIAN_POINT('Ctrl Pts',(31.3785508080852,-30.4512498324188,175.446032083677));
#26855=CARTESIAN_POINT('Ctrl Pts',(31.8903225083122,-30.2458970801104,175.408988820603));
#26856=CARTESIAN_POINT('Ctrl Pts',(32.5139456772549,-30.3192959669891,175.37194555753));
#26857=CARTESIAN_POINT('Ctrl Pts',(32.964053734261,-30.6378595604081,175.334902294457));
#26858=CARTESIAN_POINT('Ctrl Pts',(33.4141617912671,-30.9564231538271,175.297859031384));
#26859=CARTESIAN_POINT('Ctrl Pts',(33.6907547363366,-31.5201514537863,175.26081576831));
#26860=CARTESIAN_POINT('Ctrl Pts',(33.6672651375685,-32.0710854469139,175.223772505237));
#26861=CARTESIAN_POINT('Ctrl Pts',(33.6437755388003,-32.6220194400415,175.186729242164));
#26862=CARTESIAN_POINT('Ctrl Pts',(33.3202033961946,-33.1601591263375,175.149685979091));
#26863=CARTESIAN_POINT('Ctrl Pts',(32.8446135677108,-33.4392547032937,175.112642716018));
#26864=CARTESIAN_POINT('Ctrl Pts',(32.369023739227,-33.7183502802499,175.075599452944));
#26865=CARTESIAN_POINT('Ctrl Pts',(31.741416224865,-33.7384017478664,175.038556189871));
#26866=CARTESIAN_POINT('Ctrl Pts',(31.2489808201369,-33.4902336632864,175.001512926798));
#26867=CARTESIAN_POINT('Ctrl Pts',(30.7565454154088,-33.2420655787064,174.964469663725));
#26868=CARTESIAN_POINT('Ctrl Pts',(30.3992821203146,-32.7256779419299,174.927426400651));
#26869=CARTESIAN_POINT('Ctrl Pts',(30.3406726815099,-32.1773669355505,174.890383137578));
#26870=CARTESIAN_POINT('Ctrl Pts',(30.3344159150848,-32.11883278192,174.886428637255));
#26871=CARTESIAN_POINT('Ctrl Pts',(30.3315627045428,-32.0599348192507,174.882474136933));
#26872=CARTESIAN_POINT('Ctrl Pts',(30.3319794150682,-32.0009960690673,174.87851963661));
#26873=CARTESIAN_POINT('Ctrl Pts',(30.3357236107064,-32.0011913006864,175.07148036339));
#26874=CARTESIAN_POINT('Ctrl Pts',(30.3344358927105,-32.1959507846202,175.084472701363));
#26875=CARTESIAN_POINT('Ctrl Pts',(30.3660189172445,-32.3903059089451,175.097465039337));
#26876=CARTESIAN_POINT('Ctrl Pts',(30.4323117265277,-32.5719966029107,175.11045737731));
#26877=CARTESIAN_POINT('Ctrl Pts',(30.6213232792773,-33.090026243801,175.147500640383));
#26878=CARTESIAN_POINT('Ctrl Pts',(31.0924950442497,-33.5051051351073,175.184543903456));
#26879=CARTESIAN_POINT('Ctrl Pts',(31.6302213766159,-33.6272954268393,175.221587166529));
#26880=CARTESIAN_POINT('Ctrl Pts',(32.1679477089822,-33.7494857185713,175.258630429603));
#26881=CARTESIAN_POINT('Ctrl Pts',(32.7722286087424,-33.5787874107291,175.295673692676));
#26882=CARTESIAN_POINT('Ctrl Pts',(33.166548412743,-33.1933111234085,175.332716955749));
#26883=CARTESIAN_POINT('Ctrl Pts',(33.5608682167436,-32.8078348360878,175.369760218822));
#26884=CARTESIAN_POINT('Ctrl Pts',(33.7452269249847,-32.2075805692888,175.406803481895));
#26885=CARTESIAN_POINT('Ctrl Pts',(33.6352629922185,-31.6672214207547,175.443846744969));
#26886=CARTESIAN_POINT('Ctrl Pts',(33.5252990594523,-31.1268622722207,175.480890008042));
#26887=CARTESIAN_POINT('Ctrl Pts',(33.1210124856788,-30.6463982419517,175.517933271115));
#26888=CARTESIAN_POINT('Ctrl Pts',(32.6074026149042,-30.4456870649923,175.554976534189));
#26889=CARTESIAN_POINT('Ctrl Pts',(32.0937927441297,-30.2449758880328,175.592019797262));
#26890=CARTESIAN_POINT('Ctrl Pts',(31.4708595763541,-30.3240175643829,175.629063060335));
#26891=CARTESIAN_POINT('Ctrl Pts',(31.0236539514369,-30.6466430515281,175.666106323408));
#26892=CARTESIAN_POINT('Ctrl Pts',(30.5996104638076,-30.9525587850175,175.701231003402));
#26893=CARTESIAN_POINT('Ctrl Pts',(30.3335629853364,-31.4774798569709,175.736355683396));
#26894=CARTESIAN_POINT('Ctrl Pts',(30.3314186128286,-32.0005207267479,175.77148036339));
#26895=CARTESIAN_POINT('Origin',(32.,-32.,172.));
#26896=CARTESIAN_POINT('',(30.3341900498104,-31.9984780038006,176.47148036339));
#26897=CARTESIAN_POINT('',(30.3366801194269,-31.9999190844631,176.27851963661));
#26898=CARTESIAN_POINT('',(30.334,-32.,172.));
#26899=CARTESIAN_POINT('Ctrl Pts',(30.3366801194269,-31.9999190844631,176.27851963661));
#26900=CARTESIAN_POINT('Ctrl Pts',(30.3365617809194,-31.7268069895527,176.260326627145));
#26901=CARTESIAN_POINT('Ctrl Pts',(30.4000687856344,-31.4537467253374,176.24213361768));
#26902=CARTESIAN_POINT('Ctrl Pts',(30.5275023444207,-31.2147759338819,176.223940608215));
#26903=CARTESIAN_POINT('Ctrl Pts',(30.7869731511369,-30.7282012464043,176.186897345142));
#26904=CARTESIAN_POINT('Ctrl Pts',(31.3114712965213,-30.3829550314745,176.149854082068));
#26905=CARTESIAN_POINT('Ctrl Pts',(31.8609892732317,-30.3370200850388,176.112810818995));
#26906=CARTESIAN_POINT('Ctrl Pts',(32.4105072499422,-30.2910851386031,176.075767555922));
#26907=CARTESIAN_POINT('Ctrl Pts',(32.9850450579787,-30.5444614606614,176.038724292849));
#26908=CARTESIAN_POINT('Ctrl Pts',(33.3216973116788,-30.9812054201089,176.001681029775));
#26909=CARTESIAN_POINT('Ctrl Pts',(33.658349565379,-31.4179493795564,175.964637766702));
#26910=CARTESIAN_POINT('Ctrl Pts',(33.7571162647429,-32.0380609763929,175.927594503629));
#26911=CARTESIAN_POINT('Ctrl Pts',(33.5728023036849,-32.5577805063248,175.890551240556));
#26912=CARTESIAN_POINT('Ctrl Pts',(33.3884883426268,-33.0775000362566,175.853507977482));
#26913=CARTESIAN_POINT('Ctrl Pts',(32.9210937211468,-33.4968274992837,175.816464714409));
#26914=CARTESIAN_POINT('Ctrl Pts',(32.3844956836908,-33.6238809220316,175.779421451336));
#26915=CARTESIAN_POINT('Ctrl Pts',(31.8478976462348,-33.7509343447796,175.742378188263));
#26916=CARTESIAN_POINT('Ctrl Pts',(31.2420961928027,-33.5857137272483,175.705334925189));
#26917=CARTESIAN_POINT('Ctrl Pts',(30.8443027836642,-33.2038231281496,175.668291662116));
#26918=CARTESIAN_POINT('Ctrl Pts',(30.5229603216459,-32.895327153815,175.638367653614));
#26919=CARTESIAN_POINT('Ctrl Pts',(30.3373557821128,-32.4454408151666,175.608443645112));
#26920=CARTESIAN_POINT('Ctrl Pts',(30.3332691019313,-31.9985486152772,175.57851963661));
#26921=CARTESIAN_POINT('Ctrl Pts',(30.3314186128286,-32.0005207267479,175.77148036339));
#26922=CARTESIAN_POINT('Ctrl Pts',(30.331301482742,-32.0290903069594,175.77339894647));
#26923=CARTESIAN_POINT('Ctrl Pts',(30.3319717264726,-32.0576542774531,175.775317529549));
#26924=CARTESIAN_POINT('Ctrl Pts',(30.3334466035821,-32.0861766407582,175.777236112628));
#26925=CARTESIAN_POINT('Ctrl Pts',(30.3619229627037,-32.6368754449028,175.814279375701));
#26926=CARTESIAN_POINT('Ctrl Pts',(30.6903537630058,-33.1720637552517,175.851322638774));
#26927=CARTESIAN_POINT('Ctrl Pts',(31.1684508511107,-33.4468423029177,175.888365901848));
#26928=CARTESIAN_POINT('Ctrl Pts',(31.6465479392156,-33.7216208505837,175.925409164921));
#26929=CARTESIAN_POINT('Ctrl Pts',(32.2743113151233,-33.7359896355667,175.962452427994));
#26930=CARTESIAN_POINT('Ctrl Pts',(32.7644798619264,-33.4833735797891,175.999495691067));
#26931=CARTESIAN_POINT('Ctrl Pts',(33.2546484087295,-33.2307575240115,176.036538954141));
#26932=CARTESIAN_POINT('Ctrl Pts',(33.6072221264279,-32.7111566274731,176.073582217214));
#26933=CARTESIAN_POINT('Ctrl Pts',(33.6608651935486,-32.1623374429729,176.110625480287));
#26934=CARTESIAN_POINT('Ctrl Pts',(33.7145082606694,-31.6135182584726,176.14766874336));
#26935=CARTESIAN_POINT('Ctrl Pts',(33.4692206772125,-31.0354807860105,176.184712006434));
#26936=CARTESIAN_POINT('Ctrl Pts',(33.0372447113627,-30.6927318387861,176.221755269507));
#26937=CARTESIAN_POINT('Ctrl Pts',(32.6052687455129,-30.3499828915616,176.25879853258));
#26938=CARTESIAN_POINT('Ctrl Pts',(31.98660439727,-30.2425224695748,176.295841795653));
#26939=CARTESIAN_POINT('Ctrl Pts',(31.4643491177993,-30.4195238790869,176.332885058727));
#26940=CARTESIAN_POINT('Ctrl Pts',(30.9420938383286,-30.5965252885991,176.3699283218));
#26941=CARTESIAN_POINT('Ctrl Pts',(30.51624762763,-31.0579885296102,176.406971584873));
#26942=CARTESIAN_POINT('Ctrl Pts',(30.3816754027113,-31.5927505255396,176.444014847946));
#26943=CARTESIAN_POINT('Ctrl Pts',(30.3484161339968,-31.7249159328636,176.453170019761));
#26944=CARTESIAN_POINT('Ctrl Pts',(30.3329485152262,-31.8615585879079,176.462325191576));
#26945=CARTESIAN_POINT('Ctrl Pts',(30.3341900498104,-31.9984780038006,176.47148036339));
#26946=CARTESIAN_POINT('Origin',(32.,-32.,172.));
#26947=CARTESIAN_POINT('',(30.3365877619741,-32.0004154259877,177.17148036339));
#26948=CARTESIAN_POINT('',(30.3335660478939,-32.0014938873844,176.97851963661));
#26949=CARTESIAN_POINT('',(30.334,-32.,172.));
#26950=CARTESIAN_POINT('Ctrl Pts',(30.3335660478939,-32.0014938873844,176.97851963661));
#26951=CARTESIAN_POINT('Ctrl Pts',(30.3376018772674,-31.5642167073913,176.949252872251));
#26952=CARTESIAN_POINT('Ctrl Pts',(30.5142836379638,-31.1240531044688,176.919986107892));
#26953=CARTESIAN_POINT('Ctrl Pts',(30.823179352105,-30.8168181284545,176.890719343533));
#26954=CARTESIAN_POINT('Ctrl Pts',(31.2141520288524,-30.4279474660799,176.85367608046));
#26955=CARTESIAN_POINT('Ctrl Pts',(31.8169346478076,-30.2520316700382,176.816632817387));
#26956=CARTESIAN_POINT('Ctrl Pts',(32.3556971519197,-30.3695688557376,176.779589554313));
#26957=CARTESIAN_POINT('Ctrl Pts',(32.8944596560319,-30.487106041437,176.74254629124));
#26958=CARTESIAN_POINT('Ctrl Pts',(33.3692020453011,-30.8980962088774,176.705503028167));
#26959=CARTESIAN_POINT('Ctrl Pts',(33.562684776124,-31.4144724854469,176.668459765094));
#26960=CARTESIAN_POINT('Ctrl Pts',(33.756167506947,-31.9308487620163,176.63141650202));
#26961=CARTESIAN_POINT('Ctrl Pts',(33.6683905793237,-32.5526111477147,176.594373238947));
#26962=CARTESIAN_POINT('Ctrl Pts',(33.3395202396086,-32.9952445464546,176.557329975874));
#26963=CARTESIAN_POINT('Ctrl Pts',(33.0106498998934,-33.4378779451946,176.520286712801));
#26964=CARTESIAN_POINT('Ctrl Pts',(32.4406861480864,-33.7013823569761,176.483243449727));
#26965=CARTESIAN_POINT('Ctrl Pts',(31.8904413064044,-33.6651795916422,176.446200186654));
#26966=CARTESIAN_POINT('Ctrl Pts',(31.3401964647224,-33.6289768263084,176.409156923581));
#26967=CARTESIAN_POINT('Ctrl Pts',(30.8096705331653,-33.2930668838592,176.372113660508));
#26968=CARTESIAN_POINT('Ctrl Pts',(30.5416293014109,-32.8111603326219,176.335070397435));
#26969=CARTESIAN_POINT('Ctrl Pts',(30.4052308101104,-32.5659319171787,176.316220143826));
#26970=CARTESIAN_POINT('Ctrl Pts',(30.336802733054,-32.2828976792056,176.297369890218));
#26971=CARTESIAN_POINT('Ctrl Pts',(30.3366801194269,-31.9999190844631,176.27851963661));
#26972=CARTESIAN_POINT('Ctrl Pts',(30.3341900498104,-31.9984780038006,176.47148036339));
#26973=CARTESIAN_POINT('Ctrl Pts',(30.3379719591493,-32.4155560491711,176.499368454649));
#26974=CARTESIAN_POINT('Ctrl Pts',(30.4967993194642,-32.8352021786124,176.527256545907));
#26975=CARTESIAN_POINT('Ctrl Pts',(30.7800748091088,-33.1386874749035,176.555144637166));
#26976=CARTESIAN_POINT('Ctrl Pts',(31.156344679564,-33.5418016774904,176.592187900239));
#26977=CARTESIAN_POINT('Ctrl Pts',(31.7521826596132,-33.7399693318165,176.629231163313));
#26978=CARTESIAN_POINT('Ctrl Pts',(32.2949365205777,-33.6425099951321,176.666274426386));
#26979=CARTESIAN_POINT('Ctrl Pts',(32.8376903815422,-33.5450506584477,176.703317689459));
#26980=CARTESIAN_POINT('Ctrl Pts',(33.3273601234219,-33.1519643307528,176.740360952532));
#26981=CARTESIAN_POINT('Ctrl Pts',(33.5398755270596,-32.6431251814289,176.777404215605));
#26982=CARTESIAN_POINT('Ctrl Pts',(33.7523909306974,-32.1342860321049,176.814447478679));
#26983=CARTESIAN_POINT('Ctrl Pts',(33.6877519960932,-31.5096940611519,176.851490741752));
#26984=CARTESIAN_POINT('Ctrl Pts',(33.3755371500396,-31.0551591733681,176.888534004825));
#26985=CARTESIAN_POINT('Ctrl Pts',(33.0633223039859,-30.6006242855842,176.925577267898));
#26986=CARTESIAN_POINT('Ctrl Pts',(32.5035315464827,-30.3161464809697,176.962620530972));
#26987=CARTESIAN_POINT('Ctrl Pts',(31.9523220911802,-30.3319012489989,176.999663794045));
#26988=CARTESIAN_POINT('Ctrl Pts',(31.4011126358776,-30.3476560170281,177.036707057118));
#26989=CARTESIAN_POINT('Ctrl Pts',(30.8584844827757,-30.6636433577011,177.073750320191));
#26990=CARTESIAN_POINT('Ctrl Pts',(30.5727413358032,-31.1352692005083,177.110793583265));
#26991=CARTESIAN_POINT('Ctrl Pts',(30.416700083008,-31.3928189900376,177.131022509973));
#26992=CARTESIAN_POINT('Ctrl Pts',(30.3372653911337,-31.6967822724175,177.151251436682));
#26993=CARTESIAN_POINT('Ctrl Pts',(30.3365877619741,-32.0004154259877,177.17148036339));
#26994=CARTESIAN_POINT('Origin',(32.,-32.,172.));
#26995=CARTESIAN_POINT('',(30.3326674689016,-32.0013033567452,177.87148036339));
#26996=CARTESIAN_POINT('',(30.3317668085256,-31.999144727569,177.67851963661));
#26997=CARTESIAN_POINT('',(30.334,-32.,172.));
#26998=CARTESIAN_POINT('Ctrl Pts',(30.3317668085256,-31.999144727569,177.67851963661));
#26999=CARTESIAN_POINT('Ctrl Pts',(30.3314592554189,-31.9500181779958,177.67522238043));
#27000=CARTESIAN_POINT('Ctrl Pts',(30.3334412619116,-31.9009167943827,177.671925124251));
#27001=CARTESIAN_POINT('Ctrl Pts',(30.3377935944025,-31.8520264236762,177.668627868071));
#27002=CARTESIAN_POINT('Ctrl Pts',(30.3866901886209,-31.3027640172314,177.631584604998));
#27003=CARTESIAN_POINT('Ctrl Pts',(30.7347589380456,-30.7801347347176,177.594541341925));
#27004=CARTESIAN_POINT('Ctrl Pts',(31.2227253353964,-30.5232907565712,177.557498078852));
#27005=CARTESIAN_POINT('Ctrl Pts',(31.7106917327472,-30.2664467784248,177.520454815778));
#27006=CARTESIAN_POINT('Ctrl Pts',(32.3385557780241,-30.2753881046458,177.483411552705));
#27007=CARTESIAN_POINT('Ctrl Pts',(32.8190103548061,-30.5460233042592,177.446368289632));
#27008=CARTESIAN_POINT('Ctrl Pts',(33.2994649315881,-30.8166585038727,177.409325026559));
#27009=CARTESIAN_POINT('Ctrl Pts',(33.6325100398753,-31.3489875768786,177.372281763485));
#27010=CARTESIAN_POINT('Ctrl Pts',(33.6657460114371,-31.8994195908216,177.335238500412));
#27011=CARTESIAN_POINT('Ctrl Pts',(33.6989819829988,-32.4498516047646,177.298195237339));
#27012=CARTESIAN_POINT('Ctrl Pts',(33.4324088178351,-33.0183865596447,177.261151974266));
#27013=CARTESIAN_POINT('Ctrl Pts',(32.9880089668758,-33.3448659600934,177.224108711192));
#27014=CARTESIAN_POINT('Ctrl Pts',(32.5436091159166,-33.6713453605421,177.187065448119));
#27015=CARTESIAN_POINT('Ctrl Pts',(31.9213825791617,-33.7557692065595,177.150022185046));
#27016=CARTESIAN_POINT('Ctrl Pts',(31.4060568380961,-33.5595055955127,177.112978921973));
#27017=CARTESIAN_POINT('Ctrl Pts',(30.8907310970306,-33.3632419844659,177.075935658899));
#27018=CARTESIAN_POINT('Ctrl Pts',(30.4823061516544,-32.8862909163551,177.038892395826));
#27019=CARTESIAN_POINT('Ctrl Pts',(30.3676750462361,-32.3469026179459,177.001849132753));
#27020=CARTESIAN_POINT('Ctrl Pts',(30.3436105181693,-32.233668737852,176.994072634039));
#27021=CARTESIAN_POINT('Ctrl Pts',(30.3324936839814,-32.1176832066525,176.986296135324));
#27022=CARTESIAN_POINT('Ctrl Pts',(30.3335660478939,-32.0014938873844,176.97851963661));
#27023=CARTESIAN_POINT('Ctrl Pts',(30.3365877619741,-32.0004154259877,177.17148036339));
#27024=CARTESIAN_POINT('Ctrl Pts',(30.3360245148585,-32.2527960910209,177.188294699755));
#27025=CARTESIAN_POINT('Ctrl Pts',(30.3898743454176,-32.5049486708014,177.20510903612));
#27026=CARTESIAN_POINT('Ctrl Pts',(30.4993722352302,-32.7300294250239,177.221923372484));
#27027=CARTESIAN_POINT('Ctrl Pts',(30.7406044224728,-33.2258994617911,177.258966635558));
#27028=CARTESIAN_POINT('Ctrl Pts',(31.2519269378011,-33.5903751903842,177.296009898631));
#27029=CARTESIAN_POINT('Ctrl Pts',(31.7993613846112,-33.6566745899168,177.333053161704));
#27030=CARTESIAN_POINT('Ctrl Pts',(32.3467958314214,-33.7229739894494,177.370096424777));
#27031=CARTESIAN_POINT('Ctrl Pts',(32.9303422097134,-33.4910970599214,177.407139687851));
#27032=CARTESIAN_POINT('Ctrl Pts',(33.2829728326695,-33.0671492310509,177.444182950924));
#27033=CARTESIAN_POINT('Ctrl Pts',(33.6356034556255,-32.6432014021804,177.481226213997));
#27034=CARTESIAN_POINT('Ctrl Pts',(33.7573183232455,-32.0271826739674,177.51826947707));
#27035=CARTESIAN_POINT('Ctrl Pts',(33.5924214296177,-31.5009802751582,177.555312740144));
#27036=CARTESIAN_POINT('Ctrl Pts',(33.4275245359899,-30.974777876349,177.592356003217));
#27037=CARTESIAN_POINT('Ctrl Pts',(32.9760158811143,-30.5383918069435,177.62939926629));
#27038=CARTESIAN_POINT('Ctrl Pts',(32.4445032601022,-30.3915091538223,177.666442529363));
#27039=CARTESIAN_POINT('Ctrl Pts',(31.9129906390901,-30.2446265007011,177.703485792437));
#27040=CARTESIAN_POINT('Ctrl Pts',(31.3014740519416,-30.3872472638642,177.74052905551));
#27041=CARTESIAN_POINT('Ctrl Pts',(30.8897804116652,-30.7541106092808,177.777572318583));
#27042=CARTESIAN_POINT('Ctrl Pts',(30.5418867902575,-31.064121270881,177.808875000185));
#27043=CARTESIAN_POINT('Ctrl Pts',(30.3366819982801,-31.5342582446545,177.840177681788));
#27044=CARTESIAN_POINT('Ctrl Pts',(30.3326674689016,-32.0013033567452,177.87148036339));
#27045=CARTESIAN_POINT('Origin',(32.,-32.,172.));
#27046=CARTESIAN_POINT('',(30.3325025779359,-31.9987820654682,178.57148036339));
#27047=CARTESIAN_POINT('',(30.3361334267378,-31.9990537049732,178.37851963661));
#27048=CARTESIAN_POINT('',(30.334,-32.,172.));
#27049=CARTESIAN_POINT('',(33.2690708798529,-30.9206413469521,179.));
#27050=CARTESIAN_POINT('Ctrl Pts',(30.3325025779359,-31.9987820654682,178.57148036339));
#27051=CARTESIAN_POINT('Ctrl Pts',(30.336429253093,-32.4716839315359,178.60319045304));
#27052=CARTESIAN_POINT('Ctrl Pts',(30.547633069383,-32.9475800416084,178.634900542691));
#27053=CARTESIAN_POINT('Ctrl Pts',(30.9034954394858,-33.2578609596282,178.666610632341));
#27054=CARTESIAN_POINT('Ctrl Pts',(31.3192086569192,-33.6203265912177,178.703653895414));
#27055=CARTESIAN_POINT('Ctrl Pts',(31.9323311937098,-33.7567842787443,178.740697158487));
#27056=CARTESIAN_POINT('Ctrl Pts',(32.4621594616056,-33.6037851887319,178.777740421561));
#27057=CARTESIAN_POINT('Ctrl Pts',(32.9919877295014,-33.4507860987195,178.814783684634));
#27058=CARTESIAN_POINT('Ctrl Pts',(33.4385217285025,-33.008330231168,178.851826947707));
#27059=CARTESIAN_POINT('Ctrl Pts',(33.5975140831873,-32.4812854179199,178.88887021078));
#27060=CARTESIAN_POINT('Ctrl Pts',(33.7565064378722,-31.9542406046717,178.925913473854));
#27061=CARTESIAN_POINT('Ctrl Pts',(33.6279571482409,-31.3426068457268,178.962956736927));
#27062=CARTESIAN_POINT('Ctrl Pts',(33.2690708798528,-30.920641346952,179.));
#27063=CARTESIAN_POINT('',(30.7285119307802,-30.9188041231383,179.));
#27064=CARTESIAN_POINT('Origin',(32.,-32.,179.));
#27065=CARTESIAN_POINT('Ctrl Pts',(30.7285101132668,-30.918802741708,179.));
#27066=CARTESIAN_POINT('Ctrl Pts',(31.0792913649319,-30.5073972709685,178.963685183163));
#27067=CARTESIAN_POINT('Ctrl Pts',(31.6490955450374,-30.2812940154422,178.927370366325));
#27068=CARTESIAN_POINT('Ctrl Pts',(32.1864012091873,-30.3417508515848,178.891055549488));
#27069=CARTESIAN_POINT('Ctrl Pts',(32.7344847960344,-30.4034204035983,178.854012286415));
#27070=CARTESIAN_POINT('Ctrl Pts',(33.2487530018731,-30.7632616842773,178.816969023342));
#27071=CARTESIAN_POINT('Ctrl Pts',(33.4942155254316,-31.2569767153464,178.779925760268));
#27072=CARTESIAN_POINT('Ctrl Pts',(33.7396780489901,-31.7506917464154,178.742882497195));
#27073=CARTESIAN_POINT('Ctrl Pts',(33.7163348902683,-32.3782805278743,178.705839234122));
#27074=CARTESIAN_POINT('Ctrl Pts',(33.4347027853158,-32.8523839466767,178.668795971049));
#27075=CARTESIAN_POINT('Ctrl Pts',(33.1530706803632,-33.326487365479,178.631752707976));
#27076=CARTESIAN_POINT('Ctrl Pts',(32.6131496291799,-33.6471054216247,178.594709444902));
#27077=CARTESIAN_POINT('Ctrl Pts',(32.0620855996171,-33.6676123863825,178.557666181829));
#27078=CARTESIAN_POINT('Ctrl Pts',(31.5110215700544,-33.6881193511403,178.520622918756));
#27079=CARTESIAN_POINT('Ctrl Pts',(30.9488145621123,-33.4085152245102,178.483579655683));
#27080=CARTESIAN_POINT('Ctrl Pts',(30.6326876565862,-32.9567024322525,178.446536392609));
#27081=CARTESIAN_POINT('Ctrl Pts',(30.4392028425771,-32.680171353914,178.423864140609));
#27082=CARTESIAN_POINT('Ctrl Pts',(30.3379002876861,-32.33913045263,178.40119188861));
#27083=CARTESIAN_POINT('Ctrl Pts',(30.3361334267378,-31.9990537049732,178.37851963661));
#27084=CARTESIAN_POINT('Origin',(32.,-32.,180.545925280538));
#27085=CARTESIAN_POINT('',(29.9466856599289,-31.9981860411733,166.254074719462));
#27086=CARTESIAN_POINT('',(29.9453305924909,-32.0018604224553,166.195925280538));
#27087=CARTESIAN_POINT('',(29.94525,-31.9999999999998,180.545925280538));
#27088=CARTESIAN_POINT('',(32.3836679988472,-29.9813874990082,166.));
#27089=CARTESIAN_POINT('Ctrl Pts',(29.9453305924909,-32.0018604224553,166.195925280538));
#27090=CARTESIAN_POINT('Ctrl Pts',(29.9505791509393,-31.480465367446,166.167660116765));
#27091=CARTESIAN_POINT('Ctrl Pts',(30.4181725087355,-30.2681453601149,166.102351689919));
#27092=CARTESIAN_POINT('Ctrl Pts',(31.7124802469756,-29.853818061345,166.037043263073));
#27093=CARTESIAN_POINT('Ctrl Pts',(32.3836679988472,-29.9813874990082,166.));
#27094=CARTESIAN_POINT('',(33.341594060514,-30.4387497693343,166.));
#27095=CARTESIAN_POINT('Origin',(32.,-32.,166.));
#27096=CARTESIAN_POINT('Ctrl Pts',(29.9466856599289,-31.9981860411733,166.254074719462));
#27097=CARTESIAN_POINT('Ctrl Pts',(29.945018943721,-31.7888334530956,166.242741226219));
#27098=CARTESIAN_POINT('Ctrl Pts',(30.070714697938,-30.8972227664145,166.194364469902));
#27099=CARTESIAN_POINT('Ctrl Pts',(31.3452942740116,-29.6692723969184,166.109672896747));
#27100=CARTESIAN_POINT('Ctrl Pts',(32.8352805361695,-30.004840379919,166.036314816837));
#27101=CARTESIAN_POINT('Ctrl Pts',(33.3415960097258,-30.4387477375165,166.));
#27102=CARTESIAN_POINT('Origin',(32.,-32.,180.545925280538));
#27103=CARTESIAN_POINT('',(29.9479603720644,-32.0011058412333,166.954074719462));
#27104=CARTESIAN_POINT('',(29.9421603132108,-31.9992413462749,166.895925280538));
#27105=CARTESIAN_POINT('',(29.94525,-31.9999999999998,180.545925280538));
#27106=CARTESIAN_POINT('Ctrl Pts',(29.9421603132107,-31.9992413462749,166.895925280538));
#27107=CARTESIAN_POINT('Ctrl Pts',(29.9419600294583,-31.9570745630481,166.893629624944));
#27108=CARTESIAN_POINT('Ctrl Pts',(29.9622503150868,-31.2346904166825,166.854290706278));
#27109=CARTESIAN_POINT('Ctrl Pts',(30.8113033217656,-29.8821785273914,166.777908524538));
#27110=CARTESIAN_POINT('Ctrl Pts',(33.1343552073857,-29.8526442983615,166.666778735318));
#27111=CARTESIAN_POINT('Ctrl Pts',(34.4195276636713,-31.7882407779865,166.555648946099));
#27112=CARTESIAN_POINT('Ctrl Pts',(33.4898245617256,-33.917852735535,166.444519156879));
#27113=CARTESIAN_POINT('Ctrl Pts',(31.1977704424326,-34.291827179356,166.333389367659));
#27114=CARTESIAN_POINT('Ctrl Pts',(30.0344359462898,-33.0073757885885,166.250524742212));
#27115=CARTESIAN_POINT('Ctrl Pts',(29.9437005871736,-32.163786162724,166.204703379838));
#27116=CARTESIAN_POINT('Ctrl Pts',(29.9453305924909,-32.0018604224553,166.195925280538));
#27117=CARTESIAN_POINT('Ctrl Pts',(29.9479603720644,-32.0011058412333,166.954074719462));
#27118=CARTESIAN_POINT('Ctrl Pts',(29.9499872262071,-31.5865390695413,166.931667471325));
#27119=CARTESIAN_POINT('Ctrl Pts',(30.2732187500398,-30.4837122260773,166.872216960114));
#27120=CARTESIAN_POINT('Ctrl Pts',(32.0730445458741,-29.572487230153,166.77572318583));
#27121=CARTESIAN_POINT('Ctrl Pts',(34.0790345383106,-30.7446539377421,166.66459339661));
#27122=CARTESIAN_POINT('Ctrl Pts',(34.1822755906712,-33.0657579093129,166.55346360739));
#27123=CARTESIAN_POINT('Ctrl Pts',(32.2884012423449,-34.4113733924264,166.442333818171));
#27124=CARTESIAN_POINT('Ctrl Pts',(30.3505031103998,-33.638176271501,166.342537522195));
#27125=CARTESIAN_POINT('Ctrl Pts',(29.9504665674704,-32.4730975920075,166.279784489292));
#27126=CARTESIAN_POINT('Ctrl Pts',(29.9466856599289,-31.9981860411733,166.254074719462));
#27127=CARTESIAN_POINT('Origin',(32.,-32.,180.545925280538));
#27128=CARTESIAN_POINT('',(29.9425975191606,-32.001126861031,167.654074719462));
#27129=CARTESIAN_POINT('',(29.9475247565372,-31.9986057389228,167.595925280538));
#27130=CARTESIAN_POINT('',(29.94525,-31.9999999999998,180.545925280538));
#27131=CARTESIAN_POINT('Ctrl Pts',(29.9475247565372,-31.9986057389228,167.595925280538));
#27132=CARTESIAN_POINT('Ctrl Pts',(29.9459810232766,-31.7513839288824,167.582555870051));
#27133=CARTESIAN_POINT('Ctrl Pts',(30.1017581212936,-30.8210527785577,167.53214319649));
#27134=CARTESIAN_POINT('Ctrl Pts',(31.4859258720994,-29.6264115520718,167.444687259857));
#27135=CARTESIAN_POINT('Ctrl Pts',(33.7152536076064,-30.2806704956948,167.333557470637));
#27136=CARTESIAN_POINT('Ctrl Pts',(34.3748036342428,-32.5084396694031,167.222427681417));
#27137=CARTESIAN_POINT('Ctrl Pts',(32.8609514083336,-34.2708933989397,167.111297892197));
#27138=CARTESIAN_POINT('Ctrl Pts',(30.6067301545083,-33.9615685895118,167.002463758571));
#27139=CARTESIAN_POINT('Ctrl Pts',(29.9451918573301,-32.6374881445034,166.930672888018));
#27140=CARTESIAN_POINT('Ctrl Pts',(29.9421603132107,-31.9992413462749,166.895925280538));
#27141=CARTESIAN_POINT('Ctrl Pts',(29.9425975191606,-32.001126861031,167.654074719462));
#27142=CARTESIAN_POINT('Ctrl Pts',(29.9466608492467,-31.3858045629682,167.620593716431));
#27143=CARTESIAN_POINT('Ctrl Pts',(30.5667381950234,-30.0825880151908,167.550069450326));
#27144=CARTESIAN_POINT('Ctrl Pts',(32.7830165101667,-29.7010703688433,167.442501921148));
#27145=CARTESIAN_POINT('Ctrl Pts',(34.3560822562997,-31.4108732598121,167.331372131929));
#27146=CARTESIAN_POINT('Ctrl Pts',(33.7728865232597,-33.6598393714977,167.220242342709));
#27147=CARTESIAN_POINT('Ctrl Pts',(31.567165387668,-34.3897368274991,167.10911255349));
#27148=CARTESIAN_POINT('Ctrl Pts',(30.1224391605011,-33.22638563952,167.020390012407));
#27149=CARTESIAN_POINT('Ctrl Pts',(29.9466364670795,-32.271893464287,166.968710734398));
#27150=CARTESIAN_POINT('Ctrl Pts',(29.9479603720644,-32.0011058412333,166.954074719462));
#27151=CARTESIAN_POINT('Origin',(32.,-32.,180.545925280538));
#27152=CARTESIAN_POINT('',(29.9445666371917,-31.9981758746936,168.354074719462));
#27153=CARTESIAN_POINT('',(29.9472120893181,-32.0015414752182,168.295925280538));
#27154=CARTESIAN_POINT('',(29.94525,-31.9999999999998,180.545925280538));
#27155=CARTESIAN_POINT('Ctrl Pts',(29.9472120893181,-32.0015414752182,168.295925280538));
#27156=CARTESIAN_POINT('Ctrl Pts',(29.9503631656104,-31.5497213110789,168.271482115157));
#27157=CARTESIAN_POINT('Ctrl Pts',(30.3199261032473,-30.4084887988219,168.209995686702));
#27158=CARTESIAN_POINT('Ctrl Pts',(32.2059575689964,-29.5801290538745,168.111465995175));
#27159=CARTESIAN_POINT('Ctrl Pts',(34.1446868899892,-30.8604773073957,168.000336205955));
#27160=CARTESIAN_POINT('Ctrl Pts',(34.1206220806415,-33.1837043507103,167.889206416735));
#27161=CARTESIAN_POINT('Ctrl Pts',(32.1557868319255,-34.4236180514851,167.778076627515));
#27162=CARTESIAN_POINT('Ctrl Pts',(30.301908163091,-33.5631391690622,167.680316248783));
#27163=CARTESIAN_POINT('Ctrl Pts',(29.9502583186249,-32.4363731851813,167.619599133124));
#27164=CARTESIAN_POINT('Ctrl Pts',(29.9475247565372,-31.9986057389228,167.595925280538));
#27165=CARTESIAN_POINT('Ctrl Pts',(29.9445666371917,-31.9981758746936,168.354074719462));
#27166=CARTESIAN_POINT('Ctrl Pts',(29.9432922623288,-31.8597835483762,168.34656322461));
#27167=CARTESIAN_POINT('Ctrl Pts',(30.0191194196309,-31.0402920378829,168.302008466685));
#27168=CARTESIAN_POINT('Ctrl Pts',(31.1194451055679,-29.7366361290419,168.220410445686));
#27169=CARTESIAN_POINT('Ctrl Pts',(33.42387242316,-30.0325701422052,168.109280656467));
#27170=CARTESIAN_POINT('Ctrl Pts',(34.4251871441161,-32.1290746196978,167.998150867247));
#27171=CARTESIAN_POINT('Ctrl Pts',(33.2069968831276,-34.107451416473,167.887021078027));
#27172=CARTESIAN_POINT('Ctrl Pts',(30.8841761797311,-34.1571115078919,167.775891288808));
#27173=CARTESIAN_POINT('Ctrl Pts',(29.9746985475988,-32.8124183152547,167.698242502619));
#27174=CARTESIAN_POINT('Ctrl Pts',(29.9421651952428,-32.0665949724013,167.657636979504));
#27175=CARTESIAN_POINT('Ctrl Pts',(29.9425975191606,-32.001126861031,167.654074719462));
#27176=CARTESIAN_POINT('Origin',(32.,-32.,180.545925280538));
#27177=CARTESIAN_POINT('',(29.9485597394751,-32.0000193281882,169.054074719462));
#27178=CARTESIAN_POINT('',(29.9419793698485,-32.0005154407483,168.995925280538));
#27179=CARTESIAN_POINT('',(29.94525,-31.9999999999998,180.545925280538));
#27180=CARTESIAN_POINT('Ctrl Pts',(29.9419793698485,-32.0005154407483,168.995925280538));
#27181=CARTESIAN_POINT('Ctrl Pts',(29.9441754853642,-31.3482962423852,168.960408360263));
#27182=CARTESIAN_POINT('Ctrl Pts',(30.6316772367222,-30.0118437704654,168.887848176914));
#27183=CARTESIAN_POINT('Ctrl Pts',(32.9078114683222,-29.7474298595245,168.778244730493));
#27184=CARTESIAN_POINT('Ctrl Pts',(34.3848240419215,-31.5408614725078,168.667114941273));
#27185=CARTESIAN_POINT('Ctrl Pts',(33.679271515441,-33.7544916864091,168.555985152054));
#27186=CARTESIAN_POINT('Ctrl Pts',(31.4368679074494,-34.3624301361752,168.444855362834));
#27187=CARTESIAN_POINT('Ctrl Pts',(30.0896998183334,-33.1501318281965,168.358168738995));
#27188=CARTESIAN_POINT('Ctrl Pts',(29.9455877551331,-32.2344482251709,168.30852537823));
#27189=CARTESIAN_POINT('Ctrl Pts',(29.9472120893181,-32.0015414752182,168.295925280538));
#27190=CARTESIAN_POINT('Ctrl Pts',(29.9485597394751,-32.0000193281882,169.054074719462));
#27191=CARTESIAN_POINT('Ctrl Pts',(29.9485886129679,-31.6559143019464,169.035489469716));
#27192=CARTESIAN_POINT('Ctrl Pts',(30.1937796627957,-30.6259163319228,168.979860956897));
#27193=CARTESIAN_POINT('Ctrl Pts',(31.8232672776651,-29.5778194788973,168.887189181005));
#27194=CARTESIAN_POINT('Ctrl Pts',(33.9390539348382,-30.5377200098576,168.776059391785));
#27195=CARTESIAN_POINT('Ctrl Pts',(34.2802394590648,-32.8358833299508,168.664929602565));
#27196=CARTESIAN_POINT('Ctrl Pts',(32.5345745584143,-34.3690552914116,168.553799813346));
#27197=CARTESIAN_POINT('Ctrl Pts',(30.4507345015949,-33.7770119337325,168.450181518978));
#27198=CARTESIAN_POINT('Ctrl Pts',(29.949576897309,-32.5422713157353,168.383606487684));
#27199=CARTESIAN_POINT('Ctrl Pts',(29.9445666371917,-31.9981758746936,168.354074719462));
#27200=CARTESIAN_POINT('Origin',(32.,-32.,180.545925280538));
#27201=CARTESIAN_POINT('',(29.9444957030941,-32.0018139754894,169.754074719462));
#27202=CARTESIAN_POINT('',(29.9456997331156,-31.9981314623491,169.695925280538));
#27203=CARTESIAN_POINT('',(29.94525,-31.9999999999998,180.545925280538));
#27204=CARTESIAN_POINT('Ctrl Pts',(29.9456997331156,-31.9981314623491,169.695925280538));
#27205=CARTESIAN_POINT('Ctrl Pts',(29.9441243595525,-31.8219808270179,169.686377868442));
#27206=CARTESIAN_POINT('Ctrl Pts',(30.0454882735961,-30.9641640449656,169.639787193273));
#27207=CARTESIAN_POINT('Ctrl Pts',(31.2447903606557,-29.6917859067979,169.556153255031));
#27208=CARTESIAN_POINT('Ctrl Pts',(33.5295397995502,-30.113547800496,169.445023465812));
#27209=CARTESIAN_POINT('Ctrl Pts',(34.4144710010597,-32.2617702894598,169.333893676592));
#27210=CARTESIAN_POINT('Ctrl Pts',(33.0897045262574,-34.1704234482866,169.222763887372));
#27211=CARTESIAN_POINT('Ctrl Pts',(30.7676522863566,-34.092728604512,169.111634098152));
#27212=CARTESIAN_POINT('Ctrl Pts',(29.9551026106334,-32.7367311435647,169.036021229208));
#27213=CARTESIAN_POINT('Ctrl Pts',(29.9418849915895,-32.028544618634,168.997451623336));
#27214=CARTESIAN_POINT('Ctrl Pts',(29.9419793698485,-32.0005154407483,168.995925280538));
#27215=CARTESIAN_POINT('Ctrl Pts',(29.9444957030942,-32.0018139754894,169.754074719462));
#27216=CARTESIAN_POINT('Ctrl Pts',(29.9495181583603,-31.455422838666,169.724415714822));
#27217=CARTESIAN_POINT('Ctrl Pts',(30.4542707128816,-30.2184086098558,169.65771344711));
#27218=CARTESIAN_POINT('Ctrl Pts',(32.5426882959684,-29.6327901771656,169.553967916323));
#27219=CARTESIAN_POINT('Ctrl Pts',(34.2830899850343,-31.1719341498779,169.442838127104));
#27220=CARTESIAN_POINT('Ctrl Pts',(33.9340324788774,-33.4689150086206,169.331708337884));
#27221=CARTESIAN_POINT('Ctrl Pts',(31.8149694217593,-34.4215607811959,169.220578548664));
#27222=CARTESIAN_POINT('Ctrl Pts',(30.1913146775582,-33.3693337891571,169.12803400919));
#27223=CARTESIAN_POINT('Ctrl Pts',(29.9485310636531,-32.3417685781152,169.07253273279));
#27224=CARTESIAN_POINT('Ctrl Pts',(29.9485597394751,-32.0000193281882,169.054074719462));
#27225=CARTESIAN_POINT('Origin',(32.,-32.,180.545925280538));
#27226=CARTESIAN_POINT('',(29.9426483199887,-31.9988395038972,170.454074719462));
#27227=CARTESIAN_POINT('',(29.9483815094586,-32.0006260637531,170.395925280538));
#27228=CARTESIAN_POINT('',(29.94525,-31.9999999999998,180.545925280538));
#27229=CARTESIAN_POINT('Ctrl Pts',(29.9483815094586,-32.0006260637531,170.395925280538));
#27230=CARTESIAN_POINT('Ctrl Pts',(29.9494242847511,-31.6189087878515,170.375304113548));
#27231=CARTESIAN_POINT('Ctrl Pts',(30.2347805924059,-30.5500373066546,170.317639683485));
#27232=CARTESIAN_POINT('Ctrl Pts',(31.9562576167437,-29.5717742066846,170.22293199035));
#27233=CARTESIAN_POINT('Ctrl Pts',(34.0162673510713,-30.6461684490236,170.11180220113));
#27234=CARTESIAN_POINT('Ctrl Pts',(34.2310110712073,-32.9595746451244,170.00067241191));
#27235=CARTESIAN_POINT('Ctrl Pts',(32.4039576532821,-34.394788532161,169.88954262269));
#27236=CARTESIAN_POINT('Ctrl Pts',(30.3959344367109,-33.7033080295599,169.787960245566));
#27237=CARTESIAN_POINT('Ctrl Pts',(29.9502366941572,-32.5054324534664,169.723421131515));
#27238=CARTESIAN_POINT('Ctrl Pts',(29.9456997331156,-31.9981314623491,169.695925280538));
#27239=CARTESIAN_POINT('Ctrl Pts',(29.9426483199887,-31.9988395038972,170.454074719462));
#27240=CARTESIAN_POINT('Ctrl Pts',(29.9421898960853,-31.9310286004131,170.450385223002));
#27241=CARTESIAN_POINT('Ctrl Pts',(29.9759961349022,-31.1828456795586,170.409652463468));
#27242=CARTESIAN_POINT('Ctrl Pts',(30.8915734319869,-29.8390780959909,170.331876440861));
#27243=CARTESIAN_POINT('Ctrl Pts',(33.2142103690085,-29.896696381476,170.220746651642));
#27244=CARTESIAN_POINT('Ctrl Pts',(34.4256151438767,-31.8792353292564,170.109616862422));
#27245=CARTESIAN_POINT('Ctrl Pts',(33.4171232437699,-33.9722967940629,169.998487073202));
#27246=CARTESIAN_POINT('Ctrl Pts',(31.1116955190265,-34.2603336216113,169.887357283983));
#27247=CARTESIAN_POINT('Ctrl Pts',(30.0175516591059,-32.9549540883922,169.805886499402));
#27248=CARTESIAN_POINT('Ctrl Pts',(29.9432452529153,-32.1378500093702,169.761458977896));
#27249=CARTESIAN_POINT('Ctrl Pts',(29.9444957030942,-32.0018139754894,169.754074719462));
#27250=CARTESIAN_POINT('Origin',(32.,-32.,180.545925280538));
#27251=CARTESIAN_POINT('',(29.947997769693,-31.9989253081866,171.154074719462));
#27252=CARTESIAN_POINT('',(29.9434062815109,-32.0015359661597,171.095925280538));
#27253=CARTESIAN_POINT('',(29.94525,-31.9999999999998,180.545925280538));
#27254=CARTESIAN_POINT('Ctrl Pts',(29.9434062815109,-32.0015359661597,171.095925280538));
#27255=CARTESIAN_POINT('Ctrl Pts',(29.9482705648154,-31.4184384151654,171.064230358654));
#27256=CARTESIAN_POINT('Ctrl Pts',(30.5126647034041,-30.1456152646691,170.995492173698));
#27257=CARTESIAN_POINT('Ctrl Pts',(32.6715856784485,-29.666083425673,170.889710725668));
#27258=CARTESIAN_POINT('Ctrl Pts',(34.3250344044286,-31.2982814541151,170.778580936448));
#27259=CARTESIAN_POINT('Ctrl Pts',(33.8506368574238,-33.5726846859303,170.667451147228));
#27260=CARTESIAN_POINT('Ctrl Pts',(31.6825565278258,-34.4077839482373,170.556321358009));
#27261=CARTESIAN_POINT('Ctrl Pts',(30.1533956676068,-33.2932393776467,170.465812735779));
#27262=CARTESIAN_POINT('Ctrl Pts',(29.9475510736226,-32.3046145715278,170.412347376622));
#27263=CARTESIAN_POINT('Ctrl Pts',(29.9483815094586,-32.0006260637531,170.395925280538));
#27264=CARTESIAN_POINT('Ctrl Pts',(29.947997769693,-31.9989253081866,171.154074719462));
#27265=CARTESIAN_POINT('Ctrl Pts',(29.9467022464081,-31.7257714229441,171.139311468108));
#27266=CARTESIAN_POINT('Ctrl Pts',(30.1245753503767,-30.7688512324111,171.087504953681));
#27267=CARTESIAN_POINT('Ctrl Pts',(31.5753550359689,-29.6087932781905,170.99865517618));
#27268=CARTESIAN_POINT('Ctrl Pts',(33.778563379359,-30.3462451096045,170.88752538696));
#27269=CARTESIAN_POINT('Ctrl Pts',(34.3540498056764,-32.5971954824835,170.77639559774));
#27270=CARTESIAN_POINT('Ctrl Pts',(32.7751353784459,-34.3015990261089,170.665265808521));
#27271=CARTESIAN_POINT('Ctrl Pts',(30.5627970899358,-33.9129502869929,170.557825515761));
#27272=CARTESIAN_POINT('Ctrl Pts',(29.9467925613639,-32.6118632790567,170.487428486075));
#27273=CARTESIAN_POINT('Ctrl Pts',(29.9426483199887,-31.9988395038972,170.454074719462));
#27274=CARTESIAN_POINT('Origin',(32.,-32.,180.545925280538));
#27275=CARTESIAN_POINT('',(29.9465669261584,-32.0017453823422,171.854074719462));
#27276=CARTESIAN_POINT('',(29.9435984723696,-31.9983965385536,171.795925280538));
#27277=CARTESIAN_POINT('',(29.94525,-31.9999999999998,180.545925280538));
#27278=CARTESIAN_POINT('Ctrl Pts',(29.9435984723696,-31.9983965385536,171.795925280538));
#27279=CARTESIAN_POINT('Ctrl Pts',(29.9426938163605,-31.8930393932581,171.790199866834));
#27280=CARTESIAN_POINT('Ctrl Pts',(29.9979550929028,-31.1069760518487,171.747431190057));
#27281=CARTESIAN_POINT('Ctrl Pts',(31.0116476562013,-29.7815876073365,171.667619250206));
#27282=CARTESIAN_POINT('Ctrl Pts',(33.3276380087708,-29.9663896103033,171.556489460986));
#27283=CARTESIAN_POINT('Ctrl Pts',(34.4285884533479,-32.0123297883341,171.445359671767));
#27284=CARTESIAN_POINT('Ctrl Pts',(33.3069210823662,-34.0469858777925,171.334229882547));
#27285=CARTESIAN_POINT('Ctrl Pts',(30.9891737097718,-34.2082626905328,171.223100093327));
#27286=CARTESIAN_POINT('Ctrl Pts',(29.9937162558609,-32.8789600486766,171.143665225991));
#27287=CARTESIAN_POINT('Ctrl Pts',(29.9425854608491,-32.0999304238333,171.101273621728));
#27288=CARTESIAN_POINT('Ctrl Pts',(29.9434062815109,-32.0015359661597,171.095925280538));
#27289=CARTESIAN_POINT('Ctrl Pts',(29.9465669261584,-32.0017453823422,171.854074719462));
#27290=CARTESIAN_POINT('Ctrl Pts',(29.950420840573,-31.5245393636282,171.828237713214));
#27291=CARTESIAN_POINT('Ctrl Pts',(30.3537285820249,-30.3572748593973,171.765357443893));
#27292=CARTESIAN_POINT('Ctrl Pts',(32.2966168031358,-29.589561989181,171.665433911498));
#27293=CARTESIAN_POINT('Ctrl Pts',(34.1859362031082,-30.9417581335798,171.554304122278));
#27294=CARTESIAN_POINT('Ctrl Pts',(34.0747104954871,-33.2624457579713,171.443174333059));
#27295=CARTESIAN_POINT('Ctrl Pts',(32.0647322416946,-34.4277567153216,171.332044543839));
#27296=CARTESIAN_POINT('Ctrl Pts',(30.2704013335975,-33.5115699023856,171.235678005973));
#27297=CARTESIAN_POINT('Ctrl Pts',(29.9499529131283,-32.4111564365617,171.176354731181));
#27298=CARTESIAN_POINT('Ctrl Pts',(29.947997769693,-31.9989253081866,171.154074719462));
#27299=CARTESIAN_POINT('Origin',(32.,-32.,180.545925280538));
#27300=CARTESIAN_POINT('',(29.9418222803435,-32.0000454497003,172.554074719462));
#27301=CARTESIAN_POINT('',(29.948439498473,-31.9994832149056,172.495925280538));
#27302=CARTESIAN_POINT('',(29.94525,-31.9999999999998,180.545925280538));
#27303=CARTESIAN_POINT('Ctrl Pts',(29.948439498473,-31.9994832149056,172.495925280538));
#27304=CARTESIAN_POINT('Ctrl Pts',(29.9477393956008,-31.6884927931834,172.47912611194));
#27305=CARTESIAN_POINT('Ctrl Pts',(30.1602043752097,-30.6926560217899,172.425283680269));
#27306=CARTESIAN_POINT('Ctrl Pts',(31.7070205920295,-29.5891169738205,172.334397985525));
#27307=CARTESIAN_POINT('Ctrl Pts',(33.8665098861644,-30.4461870304743,172.223268196305));
#27308=CARTESIAN_POINT('Ctrl Pts',(34.3177895739383,-32.7252898664381,172.112138407085));
#27309=CARTESIAN_POINT('Ctrl Pts',(32.6478533790253,-34.3406152820788,172.001008617865));
#27310=CARTESIAN_POINT('Ctrl Pts',(30.5015906919452,-33.8409747289323,171.895604242349));
#27311=CARTESIAN_POINT('Ctrl Pts',(29.9485469148907,-32.5746971129646,171.827243129907));
#27312=CARTESIAN_POINT('Ctrl Pts',(29.9435984723696,-31.9983965385536,171.795925280538));
#27313=CARTESIAN_POINT('Ctrl Pts',(29.9418227658393,-32.0000454432629,172.554074719462));
#27314=CARTESIAN_POINT('Ctrl Pts',(29.9420432785979,-31.3223689366965,172.51716395832));
#27315=CARTESIAN_POINT('Ctrl Pts',(30.6781938256394,-29.9641726592493,172.443209934105));
#27316=CARTESIAN_POINT('Ctrl Pts',(32.9916984736889,-29.7830816277574,172.332212646816));
#27317=CARTESIAN_POINT('Ctrl Pts',(34.4003731567925,-31.6306740734072,172.221082857597));
#27318=CARTESIAN_POINT('Ctrl Pts',(33.6122523577626,-33.8162696019019,172.109953068377));
#27319=CARTESIAN_POINT('Ctrl Pts',(31.3486156850571,-34.3396348873596,171.998823279157));
#27320=CARTESIAN_POINT('Ctrl Pts',(30.0688018326291,-33.0979304878885,171.913530496186));
#27321=CARTESIAN_POINT('Ctrl Pts',(29.9448953720202,-32.2087234336225,171.865280976287));
#27322=CARTESIAN_POINT('Ctrl Pts',(29.9465669261584,-32.0017453823422,171.854074719462));
#27323=CARTESIAN_POINT('Origin',(32.,-32.,180.545925280538));
#27324=CARTESIAN_POINT('',(29.9464345031986,-31.9982258388275,173.254074719462));
#27325=CARTESIAN_POINT('',(29.9454927722119,-32.0018769614724,173.195925280538));
#27326=CARTESIAN_POINT('',(29.94525,-31.9999999999998,180.545925280538));
#27327=CARTESIAN_POINT('Ctrl Pts',(29.9454927722119,-32.0018769614724,173.195925280538));
#27328=CARTESIAN_POINT('Ctrl Pts',(29.9501525222033,-31.4877509589622,173.168052357046));
#27329=CARTESIAN_POINT('Ctrl Pts',(30.4058324164555,-30.282983669929,173.103136170481));
#27330=CARTESIAN_POINT('Ctrl Pts',(32.4282525794201,-29.6094365459927,173.001176720843));
#27331=CARTESIAN_POINT('Ctrl Pts',(34.2406392114377,-31.0631276375177,172.890046931623));
#27332=CARTESIAN_POINT('Ctrl Pts',(34.002417135868,-33.3742341552288,172.778917142403));
#27333=CARTESIAN_POINT('Ctrl Pts',(31.9316046128615,-34.4276564770234,172.667787353183));
#27334=CARTESIAN_POINT('Ctrl Pts',(30.2269632799385,-33.4359288810624,172.573456732562));
#27335=CARTESIAN_POINT('Ctrl Pts',(29.9492831681228,-32.3742469683386,172.516169375013));
#27336=CARTESIAN_POINT('Ctrl Pts',(29.948439498473,-31.9994832149056,172.495925280538));
#27337=CARTESIAN_POINT('Ctrl Pts',(29.9464345031986,-31.9982258388275,173.254074719462));
#27338=CARTESIAN_POINT('Ctrl Pts',(29.9447677417987,-31.7961753439703,173.2431334665));
#27339=CARTESIAN_POINT('Ctrl Pts',(30.0649649676893,-30.9119921533782,173.195148950464));
#27340=CARTESIAN_POINT('Ctrl Pts',(31.331936760099,-29.6650729263216,173.110121171355));
#27341=CARTESIAN_POINT('Ctrl Pts',(33.5992505047259,-30.1722716955089,172.998991382135));
#27342=CARTESIAN_POINT('Ctrl Pts',(34.4029475305773,-32.3521875880785,172.887861592915));
#27343=CARTESIAN_POINT('Ctrl Pts',(33.0074930353251,-34.2097852193539,172.776731803695));
#27344=CARTESIAN_POINT('Ctrl Pts',(30.6899918399505,-34.0450113819995,172.665602014476));
#27345=CARTESIAN_POINT('Ctrl Pts',(29.942927496564,-32.6850193607688,172.591382986398));
#27346=CARTESIAN_POINT('Ctrl Pts',(29.9418219742446,-32.002478160526,172.554207221393));
#27347=CARTESIAN_POINT('Ctrl Pts',(29.9418227658393,-32.0000454432629,172.554074719462));
#27348=CARTESIAN_POINT('Origin',(32.,-32.,180.545925280538));
#27349=CARTESIAN_POINT('',(29.9480727143584,-32.0010073134852,173.954074719462));
#27350=CARTESIAN_POINT('',(29.9420625872194,-31.9993626039853,173.895925280538));
#27351=CARTESIAN_POINT('',(29.94525,-31.9999999999998,180.545925280538));
#27352=CARTESIAN_POINT('Ctrl Pts',(29.9420625872194,-31.9993626039853,173.895925280538));
#27353=CARTESIAN_POINT('Ctrl Pts',(29.9419202242395,-31.9644052355927,173.894021865225));
#27354=CARTESIAN_POINT('Ctrl Pts',(29.9585679626885,-31.2492644513283,173.85507518684));
#27355=CARTESIAN_POINT('Ctrl Pts',(30.788964563955,-29.8948664954311,173.779085245381));
#27356=CARTESIAN_POINT('Ctrl Pts',(33.1116859870073,-29.8407528706267,173.667955456161));
#27357=CARTESIAN_POINT('Ctrl Pts',(34.417004450483,-31.7627588025647,173.556825666941));
#27358=CARTESIAN_POINT('Ctrl Pts',(33.5103066521985,-33.9018853056218,173.445695877722));
#27359=CARTESIAN_POINT('Ctrl Pts',(31.2213925844155,-34.3004270020612,173.334566088502));
#27360=CARTESIAN_POINT('Ctrl Pts',(30.0404202070706,-33.0217284667963,173.251309222774));
#27361=CARTESIAN_POINT('Ctrl Pts',(29.9439596897637,-32.17102714165,173.205095620119));
#27362=CARTESIAN_POINT('Ctrl Pts',(29.9454927722119,-32.0018769614724,173.195925280538));
#27363=CARTESIAN_POINT('Ctrl Pts',(29.9480727143584,-32.0010073134852,173.954074719462));
#27364=CARTESIAN_POINT('Ctrl Pts',(29.9498795736957,-31.5936421254285,173.932059711606));
#27365=CARTESIAN_POINT('Ctrl Pts',(30.2645751177761,-30.4982562863879,173.873001440676));
#27366=CARTESIAN_POINT('Ctrl Pts',(32.0474062508829,-29.5718431724288,173.776899906673));
#27367=CARTESIAN_POINT('Ctrl Pts',(34.0656489251761,-30.7227813617776,173.665770117453));
#27368=CARTESIAN_POINT('Ctrl Pts',(34.1934321041778,-33.0426161979683,173.554640328233));
#27369=CARTESIAN_POINT('Ctrl Pts',(32.3138100082167,-34.4082599964802,173.443510539014));
#27370=CARTESIAN_POINT('Ctrl Pts',(30.3603258304653,-33.6524318153962,173.343322002757));
#27371=CARTESIAN_POINT('Ctrl Pts',(29.9504108140525,-32.4802477861831,173.280176729573));
#27372=CARTESIAN_POINT('Ctrl Pts',(29.9464345031986,-31.9982258388275,173.254074719462));
#27373=CARTESIAN_POINT('Origin',(32.,-32.,180.545925280538));
#27374=CARTESIAN_POINT('',(29.9427579250369,-32.0012284951477,174.654074719462));
#27375=CARTESIAN_POINT('',(29.9473696346645,-31.9985278132519,174.595925280538));
#27376=CARTESIAN_POINT('',(29.94525,-31.9999999999998,180.545925280538));
#27377=CARTESIAN_POINT('Ctrl Pts',(29.9473696346645,-31.9985278132519,174.595925280538));
#27378=CARTESIAN_POINT('Ctrl Pts',(29.9457798475597,-31.7586047394747,174.582948110332));
#27379=CARTESIAN_POINT('Ctrl Pts',(30.0955630823059,-30.835744541956,174.532927677052));
#27380=CARTESIAN_POINT('Ctrl Pts',(31.4608841326267,-29.6319738217322,174.445863980699));
#27381=CARTESIAN_POINT('Ctrl Pts',(33.6969993749721,-30.2626494249117,174.33473419148));
#27382=CARTESIAN_POINT('Ctrl Pts',(34.380039192535,-32.4833294336296,174.22360440226));
#27383=CARTESIAN_POINT('Ctrl Pts',(32.8848929515401,-34.2616715861791,174.11247461304));
#27384=CARTESIAN_POINT('Ctrl Pts',(30.6193818318231,-33.9751494602321,174.003248239133));
#27385=CARTESIAN_POINT('Ctrl Pts',(29.9446908173321,-32.6447270682982,173.931065128299));
#27386=CARTESIAN_POINT('Ctrl Pts',(29.9420625872194,-31.9993626039853,173.895925280538));
#27387=CARTESIAN_POINT('Ctrl Pts',(29.9427579250369,-32.0012284951477,174.654074719462));
#27388=CARTESIAN_POINT('Ctrl Pts',(29.9470583104027,-31.3929901059041,174.620985956712));
#27389=CARTESIAN_POINT('Ctrl Pts',(30.5546327733145,-30.0963566968232,174.550853930888));
#27390=CARTESIAN_POINT('Ctrl Pts',(32.7586915544763,-29.6929282505587,174.443678641991));
#27391=CARTESIAN_POINT('Ctrl Pts',(34.3497283135974,-31.3860213487566,174.332548852772));
#27392=CARTESIAN_POINT('Ctrl Pts',(33.7903192018566,-33.6410210502512,174.221419063552));
#27393=CARTESIAN_POINT('Ctrl Pts',(31.5924293717799,-34.3941760826881,174.110289274332));
#27394=CARTESIAN_POINT('Ctrl Pts',(30.1290568288894,-33.2410713220018,174.021174492969));
#27395=CARTESIAN_POINT('Ctrl Pts',(29.9468392856247,-32.2790897948711,173.969102974679));
#27396=CARTESIAN_POINT('Ctrl Pts',(29.9480727143584,-32.0010073134852,173.954074719462));
#27397=CARTESIAN_POINT('Origin',(32.,-32.,180.545925280538));
#27398=CARTESIAN_POINT('',(29.9443485517367,-31.9982099443222,175.354074719462));
#27399=CARTESIAN_POINT('',(29.9473758037809,-32.0014692827641,175.295925280538));
#27400=CARTESIAN_POINT('',(29.94525,-31.9999999999998,180.545925280538));
#27401=CARTESIAN_POINT('Ctrl Pts',(29.9473758037809,-32.0014692827641,175.295925280538));
#27402=CARTESIAN_POINT('Ctrl Pts',(29.9503158166638,-31.5568102862893,175.271874355438));
#27403=CARTESIAN_POINT('Ctrl Pts',(30.3106831579398,-30.4229457911365,175.210780167264));
#27404=CARTESIAN_POINT('Ctrl Pts',(32.1803873356192,-29.5780887075362,175.112642716017));
#27405=CARTESIAN_POINT('Ctrl Pts',(34.1325316071812,-30.8378886267708,175.001512926798));
#27406=CARTESIAN_POINT('Ctrl Pts',(34.1330060781932,-33.1612402722117,174.890383137578));
#27407=CARTESIAN_POINT('Ctrl Pts',(32.1813765179305,-34.4218374136508,174.779253348358));
#27408=CARTESIAN_POINT('Ctrl Pts',(30.3110383976255,-33.5776135962551,174.681100729345));
#27409=CARTESIAN_POINT('Ctrl Pts',(29.9503178863629,-32.4434638727074,174.619991373405));
#27410=CARTESIAN_POINT('Ctrl Pts',(29.9473696346645,-31.9985278132519,174.595925280538));
#27411=CARTESIAN_POINT('Ctrl Pts',(29.9443485517367,-31.9982099443222,175.354074719462));
#27412=CARTESIAN_POINT('Ctrl Pts',(29.943149413098,-31.8670801077796,175.346955464891));
#27413=CARTESIAN_POINT('Ctrl Pts',(30.014316216057,-31.05494551359,175.302792947247));
#27414=CARTESIAN_POINT('Ctrl Pts',(31.095588515948,-29.7460628226547,175.221587166529));
#27415=CARTESIAN_POINT('Ctrl Pts',(33.4030129572177,-30.0176409069538,175.110457377309));
#27416=CARTESIAN_POINT('Ctrl Pts',(34.4264151550835,-32.1034525354194,174.99932758809));
#27417=CARTESIAN_POINT('Ctrl Pts',(33.2291885163936,-34.0945855253653,174.88819779887));
#27418=CARTESIAN_POINT('Ctrl Pts',(30.9070218774947,-34.168776557331,174.777068009651));
#27419=CARTESIAN_POINT('Ctrl Pts',(29.9787266265999,-32.8270204983606,174.699026983181));
#27420=CARTESIAN_POINT('Ctrl Pts',(29.9422439778867,-32.0739202099972,174.658029219785));
#27421=CARTESIAN_POINT('Ctrl Pts',(29.9427579250369,-32.0012284951477,174.654074719462));
#27422=CARTESIAN_POINT('Origin',(32.,-32.,180.545925280538));
#27423=CARTESIAN_POINT('',(29.9485555074385,-31.9999002033617,176.054074719462));
#27424=CARTESIAN_POINT('',(29.9420662633311,-32.0006422348648,175.995925280538));
#27425=CARTESIAN_POINT('',(29.94525,-31.9999999999998,180.545925280538));
#27426=CARTESIAN_POINT('Ctrl Pts',(29.9420662633311,-32.0006422348648,175.995925280538));
#27427=CARTESIAN_POINT('Ctrl Pts',(29.9447110108764,-31.3555532629716,175.960800600544));
#27428=CARTESIAN_POINT('Ctrl Pts',(30.6188898084219,-30.0253746830828,175.888632657476));
#27429=CARTESIAN_POINT('Ctrl Pts',(32.8839691281437,-29.737967179745,175.779421451336));
#27430=CARTESIAN_POINT('Ctrl Pts',(34.3798415845562,-31.515698511429,175.668291662116));
#27431=CARTESIAN_POINT('Ctrl Pts',(33.6977088310898,-33.7366573134195,175.557161872896));
#27432=CARTESIAN_POINT('Ctrl Pts',(31.4618513662959,-34.3682461754341,175.446032083677));
#27433=CARTESIAN_POINT('Ctrl Pts',(30.0958008212723,-33.1648235855215,175.358953219557));
#27434=CARTESIAN_POINT('Ctrl Pts',(29.9457876053703,-32.2416745946567,175.308917618511));
#27435=CARTESIAN_POINT('Ctrl Pts',(29.9473758037809,-32.0014692827641,175.295925280538));
#27436=CARTESIAN_POINT('Ctrl Pts',(29.9485555074385,-31.9999002033617,176.054074719462));
#27437=CARTESIAN_POINT('Ctrl Pts',(29.9484095554287,-31.6630592207583,176.035881709997));
#27438=CARTESIAN_POINT('Ctrl Pts',(30.186216996793,-30.6405615756134,175.980645437459));
#27439=CARTESIAN_POINT('Ctrl Pts',(31.797694004055,-29.5798212429744,175.888365901848));
#27440=CARTESIAN_POINT('Ctrl Pts',(33.9235011368215,-30.5173212389216,175.777236112628));
#27441=CARTESIAN_POINT('Ctrl Pts',(34.2889408886545,-32.8117527580092,175.666106323408));
#27442=CARTESIAN_POINT('Ctrl Pts',(32.5595667617289,-34.3632769560673,175.554976534188));
#27443=CARTESIAN_POINT('Ctrl Pts',(30.4616782926144,-33.7911184932325,175.45096599954));
#27444=CARTESIAN_POINT('Ctrl Pts',(29.9493888315104,-32.5493814615627,175.383998727965));
#27445=CARTESIAN_POINT('Ctrl Pts',(29.9443485517367,-31.9982099443222,175.354074719462));
#27446=CARTESIAN_POINT('Origin',(32.,-32.,180.545925280538));
#27447=CARTESIAN_POINT('',(29.9447147880612,-32.0018424760523,176.754074719462));
#27448=CARTESIAN_POINT('',(29.9454843966674,-31.9981228561279,176.695925280538));
#27449=CARTESIAN_POINT('',(29.94525,-31.9999999999998,180.545925280538));
#27450=CARTESIAN_POINT('Ctrl Pts',(29.9454843966674,-31.9981228561279,176.695925280538));
#27451=CARTESIAN_POINT('Ctrl Pts',(29.9439531582599,-31.8292542067848,176.686770108723));
#27452=CARTESIAN_POINT('Ctrl Pts',(30.040218113941,-30.9788389407387,176.640571673835));
#27453=CARTESIAN_POINT('Ctrl Pts',(31.2204530706714,-29.6998912018496,176.557329975874));
#27454=CARTESIAN_POINT('Ctrl Pts',(33.5095297265273,-30.0974979883034,176.446200186654));
#27455=CARTESIAN_POINT('Ctrl Pts',(34.4171011468898,-32.2362539844767,176.335070397435));
#27456=CARTESIAN_POINT('Ctrl Pts',(33.1125678099616,-34.1587928959332,176.223940608215));
#27457=CARTESIAN_POINT('Ctrl Pts',(30.7898244786656,-34.1056279602598,176.112810818995));
#27458=CARTESIAN_POINT('Ctrl Pts',(29.9587089014121,-32.7512990085116,176.036805709769));
#27459=CARTESIAN_POINT('Ctrl Pts',(29.9419218017192,-32.0358783362693,175.997843863617));
#27460=CARTESIAN_POINT('Ctrl Pts',(29.9420662633311,-32.0006422348648,175.995925280538));
#27461=CARTESIAN_POINT('Ctrl Pts',(29.9447147880613,-32.0018424760523,176.754074719462));
#27462=CARTESIAN_POINT('Ctrl Pts',(29.9496923513297,-31.4625295795391,176.724807955103));
#27463=CARTESIAN_POINT('Ctrl Pts',(30.443411768081,-30.2325366450479,176.658497927671));
#27464=CARTESIAN_POINT('Ctrl Pts',(32.5176554945262,-29.6271903313891,176.555144637166));
#27465=CARTESIAN_POINT('Ctrl Pts',(34.2742165827931,-31.1478662855577,176.444014847946));
#27466=CARTESIAN_POINT('Ctrl Pts',(33.9494393162254,-33.4484057729775,176.332885058727));
#27467=CARTESIAN_POINT('Ctrl Pts',(31.8405563287846,-34.4233800048647,176.221755269507));
#27468=CARTESIAN_POINT('Ctrl Pts',(30.198950093782,-33.3839739680937,176.128818489752));
#27469=CARTESIAN_POINT('Ctrl Pts',(29.9487067321385,-32.3489099677957,176.072924973071));
#27470=CARTESIAN_POINT('Ctrl Pts',(29.9485555074385,-31.9999002033617,176.054074719462));
#27471=CARTESIAN_POINT('Origin',(32.,-32.,180.545925280538));
#27472=CARTESIAN_POINT('',(29.9424957081741,-31.9989451554456,177.454074719462));
#27473=CARTESIAN_POINT('',(29.9484415989894,-32.0005123628745,177.395925280538));
#27474=CARTESIAN_POINT('',(29.94525,-31.9999999999998,180.545925280538));
#27475=CARTESIAN_POINT('Ctrl Pts',(29.9484415989894,-32.0005123628745,177.395925280538));
#27476=CARTESIAN_POINT('Ctrl Pts',(29.9492773483985,-31.6260284359245,177.375696353829));
#27477=CARTESIAN_POINT('Ctrl Pts',(30.2266509686561,-30.5646358117479,177.318424164048));
#27478=CARTESIAN_POINT('Ctrl Pts',(31.9306130769242,-29.5723716763149,177.224108711192));
#27479=CARTESIAN_POINT('Ctrl Pts',(34.0018556801289,-30.624948091138,177.112978921973));
#27480=CARTESIAN_POINT('Ctrl Pts',(34.2410216781083,-32.9359571289216,177.001849132753));
#27481=CARTESIAN_POINT('Ctrl Pts',(32.4292289371827,-34.3903883387013,176.890719343533));
#27482=CARTESIAN_POINT('Ctrl Pts',(30.4062329402781,-33.7175672281966,176.788744726128));
#27483=CARTESIAN_POINT('Ctrl Pts',(29.9501487893529,-32.5125232845343,176.723813371796));
#27484=CARTESIAN_POINT('Ctrl Pts',(29.9454843966674,-31.9981228561279,176.695925280538));
#27485=CARTESIAN_POINT('Ctrl Pts',(29.9424957081741,-31.9989451554456,177.454074719462));
#27486=CARTESIAN_POINT('Ctrl Pts',(29.942116389599,-31.9383552528433,177.450777463283));
#27487=CARTESIAN_POINT('Ctrl Pts',(29.9720237344228,-31.1974434463136,177.41043694403));
#27488=CARTESIAN_POINT('Ctrl Pts',(30.8688116391535,-29.8509059591332,177.333053161704));
#27489=CARTESIAN_POINT('Ctrl Pts',(33.1919274501366,-29.8839891344978,177.221923372484));
#27490=CARTESIAN_POINT('Ctrl Pts',(34.4242043461506,-31.8536226808824,177.110793583265));
#27491=CARTESIAN_POINT('Ctrl Pts',(33.4378756346499,-33.9572190768126,176.999663794045));
#27492=CARTESIAN_POINT('Ctrl Pts',(31.1356187743909,-34.2695898408057,176.888534004825));
#27493=CARTESIAN_POINT('Ctrl Pts',(30.0224146577596,-32.9696107419196,176.806670979964));
#27494=CARTESIAN_POINT('Ctrl Pts',(29.9433921951746,-32.145143798841,176.761851218177));
#27495=CARTESIAN_POINT('Ctrl Pts',(29.9447147880613,-32.0018424760523,176.754074719462));
#27496=CARTESIAN_POINT('Origin',(32.,-32.,180.545925280538));
#27497=CARTESIAN_POINT('',(29.9478812476528,-31.9988328933335,178.154074719462));
#27498=CARTESIAN_POINT('',(29.943606531648,-32.0016074863584,178.095925280538));
#27499=CARTESIAN_POINT('',(29.94525,-31.9999999999998,180.545925280538));
#27500=CARTESIAN_POINT('Ctrl Pts',(29.943606531648,-32.0016074863584,178.095925280538));
#27501=CARTESIAN_POINT('Ctrl Pts',(29.9485578247094,-31.4255805091263,178.064622598935));
#27502=CARTESIAN_POINT('Ctrl Pts',(30.5011474122479,-30.159563307867,177.99627665426));
#27503=CARTESIAN_POINT('Ctrl Pts',(32.6468974928654,-29.6591214220926,177.890887446511));
#27504=CARTESIAN_POINT('Ctrl Pts',(34.3174930665853,-31.2737629757136,177.779757657291));
#27505=CARTESIAN_POINT('Ctrl Pts',(33.8671444034839,-33.5530507580587,177.668627868071));
#27506=CARTESIAN_POINT('Ctrl Pts',(31.7080052904067,-34.4110023564038,177.557498078852));
#27507=CARTESIAN_POINT('Ctrl Pts',(30.1604802792039,-33.3079112757927,177.46659721634));
#27508=CARTESIAN_POINT('Ctrl Pts',(29.9477469219122,-32.3117843745653,177.412739616902));
#27509=CARTESIAN_POINT('Ctrl Pts',(29.9484415989894,-32.0005123628745,177.395925280538));
#27510=CARTESIAN_POINT('Ctrl Pts',(29.9478812476528,-31.9988328933335,178.154074719462));
#27511=CARTESIAN_POINT('Ctrl Pts',(29.9464999762263,-31.7329725296047,178.139703708389));
#27512=CARTESIAN_POINT('Ctrl Pts',(30.1180175877586,-30.7835296862564,178.088289434242));
#27513=CARTESIAN_POINT('Ctrl Pts',(31.5501292172184,-29.6134187564108,177.999831897022));
#27514=CARTESIAN_POINT('Ctrl Pts',(33.7609939876075,-30.3275486926383,177.888702107803));
#27515=CARTESIAN_POINT('Ctrl Pts',(34.3602276546561,-32.5723003233786,177.777572318583));
#27516=CARTESIAN_POINT('Ctrl Pts',(32.7994009204969,-34.2932828161059,177.666442529363));
#27517=CARTESIAN_POINT('Ctrl Pts',(30.5749909453294,-33.9266902436017,177.558609996323));
#27518=CARTESIAN_POINT('Ctrl Pts',(29.9463778715709,-32.6190568967199,177.487820726356));
#27519=CARTESIAN_POINT('Ctrl Pts',(29.9424957081741,-31.9989451554456,177.454074719462));
#27520=CARTESIAN_POINT('Origin',(32.,-32.,180.545925280538));
#27521=CARTESIAN_POINT('',(29.9473399238087,-32.0021821257033,178.854074719462));
#27522=CARTESIAN_POINT('',(29.9434031644741,-31.9984978685597,178.795925280538));
#27523=CARTESIAN_POINT('',(29.94525,-31.9999999999998,180.545925280538));
#27524=CARTESIAN_POINT('',(31.4698297828105,-33.9851743256715,179.));
#27525=CARTESIAN_POINT('Ctrl Pts',(31.4698297828105,-33.9851743256715,179.));
#27526=CARTESIAN_POINT('Ctrl Pts',(30.8097602092464,-33.8088929660693,178.962956736927));
#27527=CARTESIAN_POINT('Ctrl Pts',(30.0751175985078,-33.1125987294256,178.914314976747));
#27528=CARTESIAN_POINT('Ctrl Pts',(29.945727943022,-32.2164517005945,178.865673216568));
#27529=CARTESIAN_POINT('Ctrl Pts',(29.9473399238087,-32.0021821257033,178.854074719462));
#27530=CARTESIAN_POINT('',(32.5313334939852,-33.9887337712632,179.));
#27531=CARTESIAN_POINT('Origin',(32.,-32.,179.));
#27532=CARTESIAN_POINT('Ctrl Pts',(32.5313343692877,-33.9887364495514,179.));
#27533=CARTESIAN_POINT('Ctrl Pts',(31.8868946933699,-34.159991273772,178.963685183163));
#27534=CARTESIAN_POINT('Ctrl Pts',(30.5070458965819,-33.8408668084245,178.895660276675));
#27535=CARTESIAN_POINT('Ctrl Pts',(29.9482461031169,-32.5817482342877,178.827635370188));
#27536=CARTESIAN_POINT('Ctrl Pts',(29.9434031644741,-31.9984978685597,178.795925280538));
#27537=CARTESIAN_POINT('Origin',(-32.,32.,172.));
#27538=CARTESIAN_POINT('',(-33.6685050626317,32.0006151176758,166.67148036339));
#27539=CARTESIAN_POINT('',(-33.6648360378126,32.0014707311122,166.47851963661));
#27540=CARTESIAN_POINT('',(-33.666,32.,172.));
#27541=CARTESIAN_POINT('',(-31.3249228143254,30.4769022377465,166.));
#27542=CARTESIAN_POINT('Ctrl Pts',(-33.6648360378126,32.0014707311122,166.47851963661));
#27543=CARTESIAN_POINT('Ctrl Pts',(-33.6661874191336,32.1712146992289,166.467186143366));
#27544=CARTESIAN_POINT('Ctrl Pts',(-33.6423113042436,32.3405776208252,166.455852650123));
#27545=CARTESIAN_POINT('Ctrl Pts',(-33.5916296311322,32.5014768113726,166.444519156879));
#27546=CARTESIAN_POINT('Ctrl Pts',(-33.4259777434308,33.0273721302816,166.407475893806));
#27547=CARTESIAN_POINT('Ctrl Pts',(-32.9739636180178,33.4628498968862,166.370432630732));
#27548=CARTESIAN_POINT('Ctrl Pts',(-32.4421510381962,33.6090489648024,166.333389367659));
#27549=CARTESIAN_POINT('Ctrl Pts',(-31.9103384583745,33.7552480327186,166.296346104586));
#27550=CARTESIAN_POINT('Ctrl Pts',(-31.2987274241441,33.6121684019463,166.259302841513));
#27551=CARTESIAN_POINT('Ctrl Pts',(-30.8877524385943,33.2444370387197,166.222259578439));
#27552=CARTESIAN_POINT('Ctrl Pts',(-30.4767774530445,32.876705675493,166.185216315366));
#27553=CARTESIAN_POINT('Ctrl Pts',(-30.2664385161753,32.2843225798121,166.148173052293));
#27554=CARTESIAN_POINT('Ctrl Pts',(-30.3518675256649,31.740487435795,166.11112978922));
#27555=CARTESIAN_POINT('Ctrl Pts',(-30.4372965351546,31.1966522917781,166.074086526147));
#27556=CARTESIAN_POINT('Ctrl Pts',(-30.818493491003,30.701365099425,166.037043263073));
#27557=CARTESIAN_POINT('Ctrl Pts',(-31.3249228143254,30.4769022377465,166.));
#27558=CARTESIAN_POINT('',(-33.666,32.,166.));
#27559=CARTESIAN_POINT('Origin',(-32.,32.,166.));
#27560=CARTESIAN_POINT('',(-33.666,32.,165.));
#27561=CARTESIAN_POINT('',(-33.666,32.,172.));
#27562=CARTESIAN_POINT('Origin',(-32.,32.,165.));
#27563=CARTESIAN_POINT('',(-33.6146845196279,31.5775541929288,166.));
#27564=CARTESIAN_POINT('Origin',(-32.,32.,166.));
#27565=CARTESIAN_POINT('Ctrl Pts',(-33.6146867573337,31.5775537367509,166.));
#27566=CARTESIAN_POINT('Ctrl Pts',(-33.4771458934448,31.0546920138059,166.036314816837));
#27567=CARTESIAN_POINT('Ctrl Pts',(-33.0618726298578,30.6037510878086,166.072629633674));
#27568=CARTESIAN_POINT('Ctrl Pts',(-32.55154570234,30.4250925829005,166.108944450512));
#27569=CARTESIAN_POINT('Ctrl Pts',(-32.0309820240448,30.2428503310052,166.145987713585));
#27570=CARTESIAN_POINT('Ctrl Pts',(-31.4115130336904,30.3439235949188,166.183030976658));
#27571=CARTESIAN_POINT('Ctrl Pts',(-30.9761439936337,30.6822433025976,166.220074239731));
#27572=CARTESIAN_POINT('Ctrl Pts',(-30.540774953577,31.0205630102763,166.257117502805));
#27573=CARTESIAN_POINT('Ctrl Pts',(-30.289505863818,31.5961291617202,166.294160765878));
#27574=CARTESIAN_POINT('Ctrl Pts',(-30.3375418657213,32.145477184728,166.331204028951));
#27575=CARTESIAN_POINT('Ctrl Pts',(-30.3855778676247,32.6948252077357,166.368247292024));
#27576=CARTESIAN_POINT('Ctrl Pts',(-30.7329189611904,33.2179551023072,166.405290555098));
#27577=CARTESIAN_POINT('Ctrl Pts',(-31.2205128733123,33.4755289762921,166.442333818171));
#27578=CARTESIAN_POINT('Ctrl Pts',(-31.7081067854342,33.733102850277,166.479377081244));
#27579=CARTESIAN_POINT('Ctrl Pts',(-32.3359535161123,33.7251207036753,166.516420344317));
#27580=CARTESIAN_POINT('Ctrl Pts',(-32.8168082612591,33.4552137540432,166.553463607391));
#27581=CARTESIAN_POINT('Ctrl Pts',(-33.297663006406,33.1853068044112,166.590506870464));
#27582=CARTESIAN_POINT('Ctrl Pts',(-33.6315257660216,32.6534750517487,166.627550133537));
#27583=CARTESIAN_POINT('Ctrl Pts',(-33.6655960048379,32.1030923182541,166.66459339661));
#27584=CARTESIAN_POINT('Ctrl Pts',(-33.6677074153297,32.0689838435741,166.666889052204));
#27585=CARTESIAN_POINT('Ctrl Pts',(-33.6686674534897,32.0348041226669,166.669184707797));
#27586=CARTESIAN_POINT('Ctrl Pts',(-33.6685050626317,32.0006151176758,166.67148036339));
#27587=CARTESIAN_POINT('Origin',(-32.,32.,172.));
#27588=CARTESIAN_POINT('',(-33.6641555473647,32.0011304727029,167.37148036339));
#27589=CARTESIAN_POINT('',(-33.6638024982419,31.9991033788539,167.17851963661));
#27590=CARTESIAN_POINT('',(-33.666,32.,172.));
#27591=CARTESIAN_POINT('Ctrl Pts',(-33.6638024982419,31.9991033788539,167.17851963661));
#27592=CARTESIAN_POINT('Ctrl Pts',(-33.6621591163747,32.335235888221,167.156112388472));
#27593=CARTESIAN_POINT('Ctrl Pts',(-33.5633805615657,32.6722563635698,167.133705140335));
#27594=CARTESIAN_POINT('Ctrl Pts',(-33.3741093586448,32.9469160213603,167.111297892197));
#27595=CARTESIAN_POINT('Ctrl Pts',(-33.0612095809052,33.4009784701134,167.074254629124));
#27596=CARTESIAN_POINT('Ctrl Pts',(-32.5009923748203,33.6846081008443,167.037211366051));
#27597=CARTESIAN_POINT('Ctrl Pts',(-31.9498062295419,33.6680232843613,167.000168102977));
#27598=CARTESIAN_POINT('Ctrl Pts',(-31.3986200842636,33.6514384678784,166.963124839904));
#27599=CARTESIAN_POINT('Ctrl Pts',(-30.8564649997919,33.3346392041815,166.926081576831));
#27600=CARTESIAN_POINT('Ctrl Pts',(-30.5714360756128,32.862579407757,166.889038313758));
#27601=CARTESIAN_POINT('Ctrl Pts',(-30.2864071514337,32.3905196113324,166.851995050685));
#27602=CARTESIAN_POINT('Ctrl Pts',(-30.2585043875471,31.76319928218,166.814951787611));
#27603=CARTESIAN_POINT('Ctrl Pts',(-30.5004799090271,31.2677006444648,166.777908524538));
#27604=CARTESIAN_POINT('Ctrl Pts',(-30.742455430507,30.7722020067496,166.740865261465));
#27605=CARTESIAN_POINT('Ctrl Pts',(-31.2543092373534,30.4085250604714,166.703821998392));
#27606=CARTESIAN_POINT('Ctrl Pts',(-31.8018524365455,30.3430378599729,166.666778735318));
#27607=CARTESIAN_POINT('Ctrl Pts',(-32.3493956357375,30.2775506594744,166.629735472245));
#27608=CARTESIAN_POINT('Ctrl Pts',(-32.9326282272752,30.5102532047555,166.592692209172));
#27609=CARTESIAN_POINT('Ctrl Pts',(-33.2845996980492,30.9347609130028,166.555648946099));
#27610=CARTESIAN_POINT('Ctrl Pts',(-33.5288844815547,31.229389262788,166.529939176269));
#27611=CARTESIAN_POINT('Ctrl Pts',(-33.6617704602393,31.6164104274241,166.504229406439));
#27612=CARTESIAN_POINT('Ctrl Pts',(-33.6648360378126,32.0014707311122,166.47851963661));
#27613=CARTESIAN_POINT('Ctrl Pts',(-33.6685050626317,32.0006151176758,166.67148036339));
#27614=CARTESIAN_POINT('Ctrl Pts',(-33.6660470746791,31.4831219322734,166.70622797087));
#27615=CARTESIAN_POINT('Ctrl Pts',(-33.4064339327629,30.9635017081271,166.74097557835));
#27616=CARTESIAN_POINT('Ctrl Pts',(-32.990035371472,30.656627002776,166.77572318583));
#27617=CARTESIAN_POINT('Ctrl Pts',(-32.5461267812728,30.3294781351193,166.812766448903));
#27618=CARTESIAN_POINT('Ctrl Pts',(-31.9240318828574,30.2441141141327,166.849809711977));
#27619=CARTESIAN_POINT('Ctrl Pts',(-31.4084114760072,30.4395995850539,166.88685297505));
#27620=CARTESIAN_POINT('Ctrl Pts',(-30.892791069157,30.6350850559752,166.923896238123));
#27621=CARTESIAN_POINT('Ctrl Pts',(-30.4836451538719,31.1114200188042,166.960939501196));
#27622=CARTESIAN_POINT('Ctrl Pts',(-30.3681998517826,31.6506349336804,166.997982764269));
#27623=CARTESIAN_POINT('Ctrl Pts',(-30.2527545496932,32.1898498485566,167.035026027343));
#27624=CARTESIAN_POINT('Ctrl Pts',(-30.4310098607996,32.79194471548,167.072069290416));
#27625=CARTESIAN_POINT('Ctrl Pts',(-30.821395564629,33.1814047989309,167.109112553489));
#27626=CARTESIAN_POINT('Ctrl Pts',(-31.2117812684584,33.5708648823819,167.146155816562));
#27627=CARTESIAN_POINT('Ctrl Pts',(-31.8142973650107,33.7476901823603,167.183199079636));
#27628=CARTESIAN_POINT('Ctrl Pts',(-32.3532365200937,33.6309661003555,167.220242342709));
#27629=CARTESIAN_POINT('Ctrl Pts',(-32.8921756751766,33.5142420183508,167.257285605782));
#27630=CARTESIAN_POINT('Ctrl Pts',(-33.3675378887901,33.1039685543629,167.294328868855));
#27631=CARTESIAN_POINT('Ctrl Pts',(-33.5617996139899,32.5878847682657,167.331372131929));
#27632=CARTESIAN_POINT('Ctrl Pts',(-33.6319112761567,32.4016232078717,167.344741542416));
#27633=CARTESIAN_POINT('Ctrl Pts',(-33.6654072127856,32.2015789545508,167.358110952903));
#27634=CARTESIAN_POINT('Ctrl Pts',(-33.6641555473647,32.0011304727029,167.37148036339));
#27635=CARTESIAN_POINT('Origin',(-32.,32.,172.));
#27636=CARTESIAN_POINT('',(-33.6644090592112,31.9987501654189,168.07148036339));
#27637=CARTESIAN_POINT('',(-33.6681507222124,31.9990863362662,167.87851963661));
#27638=CARTESIAN_POINT('',(-33.666,32.,172.));
#27639=CARTESIAN_POINT('Ctrl Pts',(-33.6681507222124,31.9990863362662,167.87851963661));
#27640=CARTESIAN_POINT('Ctrl Pts',(-33.6648561568213,32.497992284639,167.845038633578));
#27641=CARTESIAN_POINT('Ctrl Pts',(-33.4261729971981,32.9996326774274,167.811557630547));
#27642=CARTESIAN_POINT('Ctrl Pts',(-33.0352709662068,33.308831725257,167.778076627516));
#27643=CARTESIAN_POINT('Ctrl Pts',(-32.6027783447553,33.6509284557524,167.741033364442));
#27644=CARTESIAN_POINT('Ctrl Pts',(-31.9839526063196,33.7574552117728,167.703990101369));
#27645=CARTESIAN_POINT('Ctrl Pts',(-31.4619649990783,33.5796660081348,167.666946838296));
#27646=CARTESIAN_POINT('Ctrl Pts',(-30.9399773918371,33.4018768044968,167.629903575223));
#27647=CARTESIAN_POINT('Ctrl Pts',(-30.5148279157903,32.9397716412004,167.592860312149));
#27648=CARTESIAN_POINT('Ctrl Pts',(-30.3810627764268,32.4048071708948,167.555817049076));
#27649=CARTESIAN_POINT('Ctrl Pts',(-30.2472976370633,31.8698427005891,167.518773786003));
#27650=CARTESIAN_POINT('Ctrl Pts',(-30.404916834383,31.2620189232743,167.48173052293));
#27651=CARTESIAN_POINT('Ctrl Pts',(-30.7817944533159,30.8594730384074,167.444687259856));
#27652=CARTESIAN_POINT('Ctrl Pts',(-31.1586720722489,30.4569271535405,167.407643996783));
#27653=CARTESIAN_POINT('Ctrl Pts',(-31.7548081127951,30.2596591611215,167.37060073371));
#27654=CARTESIAN_POINT('Ctrl Pts',(-32.2974144133735,30.3579371433043,167.333557470637));
#27655=CARTESIAN_POINT('Ctrl Pts',(-32.8400207139519,30.4562151254872,167.296514207563));
#27656=CARTESIAN_POINT('Ctrl Pts',(-33.3290972745624,30.8500390822719,167.25947094449));
#27657=CARTESIAN_POINT('Ctrl Pts',(-33.5408443801705,31.3591986940519,167.222427681417));
#27658=CARTESIAN_POINT('Ctrl Pts',(-33.6245069288544,31.5603707038703,167.207791666481));
#27659=CARTESIAN_POINT('Ctrl Pts',(-33.6648759259742,31.7795476173752,167.193155651546));
#27660=CARTESIAN_POINT('Ctrl Pts',(-33.6638024982419,31.9991033788539,167.17851963661));
#27661=CARTESIAN_POINT('Ctrl Pts',(-33.6641555473647,32.0011304727029,167.37148036339));
#27662=CARTESIAN_POINT('Ctrl Pts',(-33.661939163726,31.6461867887672,167.395154215976));
#27663=CARTESIAN_POINT('Ctrl Pts',(-33.5507700288489,31.2899756271486,167.418828068562));
#27664=CARTESIAN_POINT('Ctrl Pts',(-33.3410204559846,31.0067777430984,167.442501921148));
#27665=CARTESIAN_POINT('Ctrl Pts',(-33.0128183359932,30.5636486122348,167.479545184222));
#27666=CARTESIAN_POINT('Ctrl Pts',(-32.4432528592241,30.2992844587142,167.516588447295));
#27667=CARTESIAN_POINT('Ctrl Pts',(-31.8929540089092,30.3346569212847,167.553631710368));
#27668=CARTESIAN_POINT('Ctrl Pts',(-31.3426551585943,30.3700293838553,167.590674973441));
#27669=CARTESIAN_POINT('Ctrl Pts',(-30.8116229347336,30.7051384625169,167.627718236515));
#27670=CARTESIAN_POINT('Ctrl Pts',(-30.5428548480621,31.1866400424654,167.664761499588));
#27671=CARTESIAN_POINT('Ctrl Pts',(-30.2740867613905,31.6681416224139,167.701804762661));
#27672=CARTESIAN_POINT('Ctrl Pts',(-30.2675828119081,32.2960357036492,167.738848025734));
#27673=CARTESIAN_POINT('Ctrl Pts',(-30.5263191497755,32.7830013677887,167.775891288808));
#27674=CARTESIAN_POINT('Ctrl Pts',(-30.7850554876429,33.2699670319283,167.812934551881));
#27675=CARTESIAN_POINT('Ctrl Pts',(-31.30903211286,33.616004278972,167.849977814954));
#27676=CARTESIAN_POINT('Ctrl Pts',(-31.8584801736076,33.662768336769,167.887021078027));
#27677=CARTESIAN_POINT('Ctrl Pts',(-32.4079282343552,33.709532394566,167.924064341101));
#27678=CARTESIAN_POINT('Ctrl Pts',(-32.9828477306334,33.4570232631162,167.961107604174));
#27679=CARTESIAN_POINT('Ctrl Pts',(-33.3201586130435,33.0207877538663,167.998150867247));
#27680=CARTESIAN_POINT('Ctrl Pts',(-33.5427347307921,32.7329357718042,168.022594032628));
#27681=CARTESIAN_POINT('Ctrl Pts',(-33.6618541533202,32.3650878520419,168.047037198009));
#27682=CARTESIAN_POINT('Ctrl Pts',(-33.6644090592112,31.9987501654189,168.07148036339));
#27683=CARTESIAN_POINT('Origin',(-32.,32.,172.));
#27684=CARTESIAN_POINT('',(-33.668651770133,31.9995820784764,168.77148036339));
#27685=CARTESIAN_POINT('',(-33.6665541529016,32.0014790085921,168.57851963661));
#27686=CARTESIAN_POINT('',(-33.666,32.,172.));
#27687=CARTESIAN_POINT('Ctrl Pts',(-33.6665541529016,32.0014790085921,168.57851963661));
#27688=CARTESIAN_POINT('Ctrl Pts',(-33.6675874214856,32.1136880980852,168.571008141758));
#27689=CARTESIAN_POINT('Ctrl Pts',(-33.6572223312059,32.2257073770859,168.563496646906));
#27690=CARTESIAN_POINT('Ctrl Pts',(-33.6347589488988,32.3352456179051,168.555985152054));
#27691=CARTESIAN_POINT('Ctrl Pts',(-33.5239798035077,32.8754382095492,168.518941888981));
#27692=CARTESIAN_POINT('Ctrl Pts',(-33.1189687371489,33.3552916534455,168.481898625907));
#27693=CARTESIAN_POINT('Ctrl Pts',(-32.6050566180813,33.5552276150071,168.444855362834));
#27694=CARTESIAN_POINT('Ctrl Pts',(-32.0911444990138,33.7551635765688,168.407812099761));
#27695=CARTESIAN_POINT('Ctrl Pts',(-31.4683313272375,33.6751820557957,168.370768836687));
#27696=CARTESIAN_POINT('Ctrl Pts',(-31.0216130323314,33.3518821640458,168.333725573614));
#27697=CARTESIAN_POINT('Ctrl Pts',(-30.5748947374253,33.0285822722958,168.296682310541));
#27698=CARTESIAN_POINT('Ctrl Pts',(-30.3042713193893,32.461964009569,168.259639047468));
#27699=CARTESIAN_POINT('Ctrl Pts',(-30.3335785884741,31.9113088182212,168.222595784395));
#27700=CARTESIAN_POINT('Ctrl Pts',(-30.3628858575589,31.3606536268733,168.185552521321));
#27701=CARTESIAN_POINT('Ctrl Pts',(-30.6921238137645,30.8259615069045,168.148509258248));
#27702=CARTESIAN_POINT('Ctrl Pts',(-31.1706349503903,30.5519046778648,168.111465995175));
#27703=CARTESIAN_POINT('Ctrl Pts',(-31.6491460870161,30.277847848825,168.074422732101));
#27704=CARTESIAN_POINT('Ctrl Pts',(-32.2769304040622,30.2644263107144,168.037379469028));
#27705=CARTESIAN_POINT('Ctrl Pts',(-32.7667172084993,30.5177816770287,168.000336205955));
#27706=CARTESIAN_POINT('Ctrl Pts',(-33.2565040129364,30.7711370433429,167.963292942882));
#27707=CARTESIAN_POINT('Ctrl Pts',(-33.6082933047646,31.2912693140819,167.926249679809));
#27708=CARTESIAN_POINT('Ctrl Pts',(-33.661108198445,31.8401688019366,167.889206416735));
#27709=CARTESIAN_POINT('Ctrl Pts',(-33.6661871350657,31.8929536418872,167.885644156694));
#27710=CARTESIAN_POINT('Ctrl Pts',(-33.6685012522917,31.9460045118401,167.882081896652));
#27711=CARTESIAN_POINT('Ctrl Pts',(-33.6681507222124,31.9990863362662,167.87851963661));
#27712=CARTESIAN_POINT('Ctrl Pts',(-33.6644090592112,31.9987501654189,168.07148036339));
#27713=CARTESIAN_POINT('Ctrl Pts',(-33.6657260761899,31.8099083944035,168.084080461082));
#27714=CARTESIAN_POINT('Ctrl Pts',(-33.6360689501427,31.6214679305664,168.096680558775));
#27715=CARTESIAN_POINT('Ctrl Pts',(-33.573642203788,31.4445932896112,168.109280656467));
#27716=CARTESIAN_POINT('Ctrl Pts',(-33.3901126435801,30.9245962216557,168.14632391954));
#27717=CARTESIAN_POINT('Ctrl Pts',(-32.9233512546222,30.5045639727946,168.183367182613));
#27718=CARTESIAN_POINT('Ctrl Pts',(-32.3869455163211,30.3767010230759,168.220410445686));
#27719=CARTESIAN_POINT('Ctrl Pts',(-31.8505397780201,30.2488380733572,168.25745370876));
#27720=CARTESIAN_POINT('Ctrl Pts',(-31.2444896903759,30.4131444227807,168.294496971833));
#27721=CARTESIAN_POINT('Ctrl Pts',(-30.8461204879495,30.7944343765193,168.331540234906));
#27722=CARTESIAN_POINT('Ctrl Pts',(-30.4477512855231,31.1757243302579,168.36858349798));
#27723=CARTESIAN_POINT('Ctrl Pts',(-30.2570629683146,31.7739978883115,168.405626761053));
#27724=CARTESIAN_POINT('Ctrl Pts',(-30.3613134760073,32.3154883146385,168.442670024126));
#27725=CARTESIAN_POINT('Ctrl Pts',(-30.4655639837,32.8569787409655,168.479713287199));
#27726=CARTESIAN_POINT('Ctrl Pts',(-30.864753316294,33.3416860355659,168.516756550272));
#27727=CARTESIAN_POINT('Ctrl Pts',(-31.376214599859,33.5478107685873,168.553799813346));
#27728=CARTESIAN_POINT('Ctrl Pts',(-31.887675883424,33.7539355016086,168.590843076419));
#27729=CARTESIAN_POINT('Ctrl Pts',(-32.51140911796,33.681477673051,168.627886339492));
#27730=CARTESIAN_POINT('Ctrl Pts',(-32.9619973573219,33.3635935924051,168.664929602565));
#27731=CARTESIAN_POINT('Ctrl Pts',(-33.3940194106328,33.0588077119969,168.70044652284));
#27732=CARTESIAN_POINT('Ctrl Pts',(-33.6668711504497,32.5284041436776,168.735963443115));
#27733=CARTESIAN_POINT('Ctrl Pts',(-33.668651770133,31.9995820784764,168.77148036339));
#27734=CARTESIAN_POINT('Origin',(-32.,32.,172.));
#27735=CARTESIAN_POINT('',(-33.6656352839714,32.0015150181746,169.47148036339));
#27736=CARTESIAN_POINT('',(-33.6633165285087,31.9999843286219,169.27851963661));
#27737=CARTESIAN_POINT('',(-33.666,32.,172.));
#27738=CARTESIAN_POINT('Ctrl Pts',(-33.6633165285087,31.9999843286219,169.27851963661));
#27739=CARTESIAN_POINT('Ctrl Pts',(-33.6632931177575,32.278986154171,169.259934386864));
#27740=CARTESIAN_POINT('Ctrl Pts',(-33.5968742307684,32.5579984542452,169.241349137118));
#27741=CARTESIAN_POINT('Ctrl Pts',(-33.4641220334618,32.8007328620376,169.222763887372));
#27742=CARTESIAN_POINT('Ctrl Pts',(-33.1995264732404,33.2845398943726,169.185720624299));
#27743=CARTESIAN_POINT('Ctrl Pts',(-32.6714110598214,33.6242271051177,169.148677361225));
#27744=CARTESIAN_POINT('Ctrl Pts',(-32.1214385428041,33.6643554685053,169.111634098152));
#27745=CARTESIAN_POINT('Ctrl Pts',(-31.5714660257869,33.7044838318928,169.074590835079));
#27746=CARTESIAN_POINT('Ctrl Pts',(-30.9996364051713,33.4450533479228,169.037547572006));
#27747=CARTESIAN_POINT('Ctrl Pts',(-30.6676158147234,33.0047779993727,169.000504308933));
#27748=CARTESIAN_POINT('Ctrl Pts',(-30.3355952242756,32.5645026508225,168.963461045859));
#27749=CARTESIAN_POINT('Ctrl Pts',(-30.2433836639953,31.9433824376922,168.926417782786));
#27750=CARTESIAN_POINT('Ctrl Pts',(-30.4331766438925,31.4256386015936,168.889374519713));
#27751=CARTESIAN_POINT('Ctrl Pts',(-30.6229696237896,30.907894765495,168.85233125664));
#27752=CARTESIAN_POINT('Ctrl Pts',(-31.094767143864,30.4935273064282,168.815287993566));
#27753=CARTESIAN_POINT('Ctrl Pts',(-31.6326772171009,30.3721485269141,168.778244730493));
#27754=CARTESIAN_POINT('Ctrl Pts',(-32.1705872903377,30.2507697473999,168.74120146742));
#27755=CARTESIAN_POINT('Ctrl Pts',(-32.774609916737,30.4223796474386,168.704158204347));
#27756=CARTESIAN_POINT('Ctrl Pts',(-33.1683476177251,30.8084504671538,168.667114941273));
#27757=CARTESIAN_POINT('Ctrl Pts',(-33.4822446548877,31.1162352846591,168.637583173052));
#27758=CARTESIAN_POINT('Ctrl Pts',(-33.6624918125908,31.5603241002161,168.608051404831));
#27759=CARTESIAN_POINT('Ctrl Pts',(-33.6665541529016,32.0014790085921,168.57851963661));
#27760=CARTESIAN_POINT('Ctrl Pts',(-33.668651770133,31.9995820784764,168.77148036339));
#27761=CARTESIAN_POINT('Ctrl Pts',(-33.6687282924218,31.9768559033307,168.773006706189));
#27762=CARTESIAN_POINT('Ctrl Pts',(-33.6683041847769,31.954132648997,168.774533048987));
#27763=CARTESIAN_POINT('Ctrl Pts',(-33.6673705657548,31.9314303480246,168.776059391785));
#27764=CARTESIAN_POINT('Ctrl Pts',(-33.6447122906379,31.3804615170241,168.813102654858));
#27765=CARTESIAN_POINT('Ctrl Pts',(-33.3219524962164,30.8418341877571,168.850145917932));
#27766=CARTESIAN_POINT('Ctrl Pts',(-32.8467843143074,30.5620213055182,168.887189181005));
#27767=CARTESIAN_POINT('Ctrl Pts',(-32.3716161323985,30.2822084232793,168.924232444078));
#27768=CARTESIAN_POINT('Ctrl Pts',(-31.7440395630021,30.2612099880684,168.961275707151));
#27769=CARTESIAN_POINT('Ctrl Pts',(-31.2512302413907,30.5086347699753,168.998318970225));
#27770=CARTESIAN_POINT('Ctrl Pts',(-30.7584209197793,30.7560595518823,169.035362233298));
#27771=CARTESIAN_POINT('Ctrl Pts',(-30.4003788459528,31.2719075509071,169.072405496371));
#27772=CARTESIAN_POINT('Ctrl Pts',(-30.3409421314876,31.8201295197669,169.109448759444));
#27773=CARTESIAN_POINT('Ctrl Pts',(-30.2815054170224,32.3683514886268,169.146492022518));
#27774=CARTESIAN_POINT('Ctrl Pts',(-30.5206740619185,32.9489474273217,169.183535285591));
#27775=CARTESIAN_POINT('Ctrl Pts',(-30.9490057911116,33.2962397824545,169.220578548664));
#27776=CARTESIAN_POINT('Ctrl Pts',(-31.3773375203046,33.6435321375873,169.257621811737));
#27777=CARTESIAN_POINT('Ctrl Pts',(-31.9948323337946,33.7575209091579,169.294665074811));
#27778=CARTESIAN_POINT('Ctrl Pts',(-32.5189279531536,33.5860454533744,169.331708337884));
#27779=CARTESIAN_POINT('Ctrl Pts',(-33.0430235725127,33.414569997591,169.368751600957));
#27780=CARTESIAN_POINT('Ctrl Pts',(-33.4737199977408,32.9576303144533,169.40579486403));
#27781=CARTESIAN_POINT('Ctrl Pts',(-33.6139328800083,32.4243195253129,169.442838127104));
#27782=CARTESIAN_POINT('Ctrl Pts',(-33.6500708996387,32.2868657089774,169.452385539199));
#27783=CARTESIAN_POINT('Ctrl Pts',(-33.6669126034726,32.1443386930928,169.461932951295));
#27784=CARTESIAN_POINT('Ctrl Pts',(-33.6656352839714,32.0015150181746,169.47148036339));
#27785=CARTESIAN_POINT('Origin',(-32.,32.,172.));
#27786=CARTESIAN_POINT('',(-33.6634608884496,31.9994923848796,170.17148036339));
#27787=CARTESIAN_POINT('',(-33.6666116665711,31.998529220922,169.97851963661));
#27788=CARTESIAN_POINT('',(-33.666,32.,172.));
#27789=CARTESIAN_POINT('Ctrl Pts',(-33.6666116665711,31.998529220922,169.97851963661));
#27790=CARTESIAN_POINT('Ctrl Pts',(-33.6625394383818,32.441545489247,169.94886063197));
#27791=CARTESIAN_POINT('Ctrl Pts',(-33.4805649416139,32.8875165690686,169.91920162733));
#27792=CARTESIAN_POINT('Ctrl Pts',(-33.1642582641494,33.1955455405692,169.88954262269));
#27793=CARTESIAN_POINT('Ctrl Pts',(-32.7692001154543,33.5802650672038,169.852499359617));
#27794=CARTESIAN_POINT('Ctrl Pts',(-32.164593063158,33.7498044530175,169.815456096544));
#27795=CARTESIAN_POINT('Ctrl Pts',(-31.6271020160461,33.6265833943509,169.778412833471));
#27796=CARTESIAN_POINT('Ctrl Pts',(-31.0896109689343,33.5033623356844,169.741369570397));
#27797=CARTESIAN_POINT('Ctrl Pts',(-30.6192359270069,33.0873808325376,169.704326307324));
#27798=CARTESIAN_POINT('Ctrl Pts',(-30.4312179589473,32.568989765185,169.667283044251));
#27799=CARTESIAN_POINT('Ctrl Pts',(-30.2431999908877,32.0505986978324,169.630239781178));
#27800=CARTESIAN_POINT('Ctrl Pts',(-30.3375390966959,31.4297980662739,169.593196518104));
#27801=CARTESIAN_POINT('Ctrl Pts',(-30.6710662130869,30.990662873359,169.556153255031));
#27802=CARTESIAN_POINT('Ctrl Pts',(-31.0045933294779,30.5515276804442,169.519109991958));
#27803=CARTESIAN_POINT('Ctrl Pts',(-31.5773084564517,30.2940579261729,169.482066728885));
#27804=CARTESIAN_POINT('Ctrl Pts',(-32.1271402573229,30.3360703740291,169.445023465812));
#27805=CARTESIAN_POINT('Ctrl Pts',(-32.6769720581941,30.3780828218853,169.407980202738));
#27806=CARTESIAN_POINT('Ctrl Pts',(-33.2039205329627,30.7195774718689,169.370936939665));
#27807=CARTESIAN_POINT('Ctrl Pts',(-33.466856916835,31.2042882238232,169.333893676592));
#27808=CARTESIAN_POINT('Ctrl Pts',(-33.5978735410497,31.4458111561248,169.315435663264));
#27809=CARTESIAN_POINT('Ctrl Pts',(-33.6633397789876,31.7228925765749,169.296977649937));
#27810=CARTESIAN_POINT('Ctrl Pts',(-33.6633165285087,31.9999843286219,169.27851963661));
#27811=CARTESIAN_POINT('Ctrl Pts',(-33.6656352839714,32.0015150181746,169.47148036339));
#27812=CARTESIAN_POINT('Ctrl Pts',(-33.6619566969046,31.590193244031,169.498976214368));
#27813=CARTESIAN_POINT('Ctrl Pts',(-33.5079992892159,31.1764109857402,169.526472065345));
#27814=CARTESIAN_POINT('Ctrl Pts',(-33.2318839374529,30.8742609692386,169.553967916323));
#27815=CARTESIAN_POINT('Ctrl Pts',(-32.8598927733233,30.4671950974478,169.591011179396));
#27816=CARTESIAN_POINT('Ctrl Pts',(-32.2661811057571,30.2627452490095,169.62805444247));
#27817=CARTESIAN_POINT('Ctrl Pts',(-31.7224281745655,30.3544665659857,169.665097705543));
#27818=CARTESIAN_POINT('Ctrl Pts',(-31.1786752433738,30.4461878829619,169.702140968616));
#27819=CARTESIAN_POINT('Ctrl Pts',(-30.6848810485567,30.8340803653528,169.739184231689));
#27820=CARTESIAN_POINT('Ctrl Pts',(-30.4670031361747,31.3406465164756,169.776227494763));
#27821=CARTESIAN_POINT('Ctrl Pts',(-30.2491252237927,31.8472126675985,169.813270757836));
#27822=CARTESIAN_POINT('Ctrl Pts',(-30.307163593846,32.4724524874533,169.850314020909));
#27823=CARTESIAN_POINT('Ctrl Pts',(-30.6145602028981,32.9302596246963,169.887357283982));
#27824=CARTESIAN_POINT('Ctrl Pts',(-30.9219568119501,33.3880667619393,169.924400547056));
#27825=CARTESIAN_POINT('Ctrl Pts',(-31.4787116600011,33.6784412165704,169.961443810129));
#27826=CARTESIAN_POINT('Ctrl Pts',(-32.0300567474602,33.6685092126404,169.998487073202));
#27827=CARTESIAN_POINT('Ctrl Pts',(-32.5814018349192,33.6585772087105,170.035530336275));
#27828=CARTESIAN_POINT('Ctrl Pts',(-33.1273371617865,33.3483387462194,170.072573599349));
#27829=CARTESIAN_POINT('Ctrl Pts',(-33.4180456826985,32.879757263405,170.109616862422));
#27830=CARTESIAN_POINT('Ctrl Pts',(-33.5798767002072,32.6189082937509,170.130238029411));
#27831=CARTESIAN_POINT('Ctrl Pts',(-33.6626154018631,32.308990355304,170.150859196401));
#27832=CARTESIAN_POINT('Ctrl Pts',(-33.6634608884496,31.9994923848796,170.17148036339));
#27833=CARTESIAN_POINT('Origin',(-32.,32.,172.));
#27834=CARTESIAN_POINT('',(-33.6674948241645,31.9987546321869,170.87148036339));
#27835=CARTESIAN_POINT('',(-33.6681095326863,32.0009409351981,170.67851963661));
#27836=CARTESIAN_POINT('',(-33.666,32.,172.));
#27837=CARTESIAN_POINT('Ctrl Pts',(-33.6681095326863,32.0009409351981,170.67851963661));
#27838=CARTESIAN_POINT('Ctrl Pts',(-33.6684812247459,32.0559223054817,170.674830140149));
#27839=CARTESIAN_POINT('Ctrl Pts',(-33.665998456693,32.1108696974031,170.671140643689));
#27840=CARTESIAN_POINT('Ctrl Pts',(-33.6605508302034,32.1655215560754,170.667451147228));
#27841=CARTESIAN_POINT('Ctrl Pts',(-33.6058555992036,32.7142368617943,170.630407884155));
#27842=CARTESIAN_POINT('Ctrl Pts',(-33.2522862982848,33.2331607873135,170.593364621082));
#27843=CARTESIAN_POINT('Ctrl Pts',(-32.7616343223977,33.4848365580631,170.556321358009));
#27844=CARTESIAN_POINT('Ctrl Pts',(-32.2709823465107,33.7365123288128,170.519278094935));
#27845=CARTESIAN_POINT('Ctrl Pts',(-31.6432476956554,33.720939944793,170.482234831862));
#27846=CARTESIAN_POINT('Ctrl Pts',(-31.1656783423139,33.4452452444934,170.445191568789));
#27847=CARTESIAN_POINT('Ctrl Pts',(-30.6881089889724,33.1695505441939,170.408148305716));
#27848=CARTESIAN_POINT('Ctrl Pts',(-30.3607049331446,32.6337335276146,170.371105042642));
#27849=CARTESIAN_POINT('Ctrl Pts',(-30.3332844955028,32.0829811561954,170.334061779569));
#27850=CARTESIAN_POINT('Ctrl Pts',(-30.305864057861,31.5322287847762,170.297018516496));
#27851=CARTESIAN_POINT('Ctrl Pts',(-30.5784272384051,30.9665410585172,170.259975253423));
#27852=CARTESIAN_POINT('Ctrl Pts',(-31.0262506036305,30.6447736136405,170.22293199035));
#27853=CARTESIAN_POINT('Ctrl Pts',(-31.4740739688559,30.3230061687638,170.185888727276));
#27854=CARTESIAN_POINT('Ctrl Pts',(-32.0971575187626,30.2451590052694,170.148845464203));
#27855=CARTESIAN_POINT('Ctrl Pts',(-32.6103815994432,30.4468545630637,170.11180220113));
#27856=CARTESIAN_POINT('Ctrl Pts',(-33.1236056801237,30.6485501208579,170.074758938057));
#27857=CARTESIAN_POINT('Ctrl Pts',(-33.526970291578,31.1297883999409,170.037715674983));
#27858=CARTESIAN_POINT('Ctrl Pts',(-33.6358979747582,31.67035737321,170.00067241191));
#27859=CARTESIAN_POINT('Ctrl Pts',(-33.6576117790083,31.7781151857933,169.993288153477));
#27860=CARTESIAN_POINT('Ctrl Pts',(-33.6676255369189,31.8882306234047,169.985903895043));
#27861=CARTESIAN_POINT('Ctrl Pts',(-33.6666116665711,31.998529220922,169.97851963661));
#27862=CARTESIAN_POINT('Ctrl Pts',(-33.6634608884496,31.9994923848796,170.17148036339));
#27863=CARTESIAN_POINT('Ctrl Pts',(-33.6641342093131,31.7530172260951,170.187902459474));
#27864=CARTESIAN_POINT('Ctrl Pts',(-33.6128703196196,31.5068084137666,170.204324555558));
#27865=CARTESIAN_POINT('Ctrl Pts',(-33.5082545871963,31.2858610072716,170.220746651642));
#27866=CARTESIAN_POINT('Ctrl Pts',(-33.2722732558253,30.78747073709,170.257789914715));
#27867=CARTESIAN_POINT('Ctrl Pts',(-32.7648288781263,30.4176146998644,170.294833177788));
#27868=CARTESIAN_POINT('Ctrl Pts',(-32.2181252498319,30.3455370127683,170.331876440861));
#27869=CARTESIAN_POINT('Ctrl Pts',(-31.6714216215375,30.2734593256722,170.368919703935));
#27870=CARTESIAN_POINT('Ctrl Pts',(-31.0854587426478,30.4991599887057,170.405962967008));
#27871=CARTESIAN_POINT('Ctrl Pts',(-30.7283700492912,30.9193596022755,170.443006230081));
#27872=CARTESIAN_POINT('Ctrl Pts',(-30.3712813559346,31.3395592158453,170.480049493154));
#27873=CARTESIAN_POINT('Ctrl Pts',(-30.2430668481111,31.9542577799514,170.517092756227));
#27874=CARTESIAN_POINT('Ctrl Pts',(-30.4023967893865,32.482172564723,170.554136019301));
#27875=CARTESIAN_POINT('Ctrl Pts',(-30.561726730662,33.0100873494947,170.591179282374));
#27876=CARTESIAN_POINT('Ctrl Pts',(-31.0086011210365,33.4512183549319,170.628222545447));
#27877=CARTESIAN_POINT('Ctrl Pts',(-31.53853266255,33.6037064248798,170.66526580852));
#27878=CARTESIAN_POINT('Ctrl Pts',(-32.0684642040635,33.7561944948277,170.702309071594));
#27879=CARTESIAN_POINT('Ctrl Pts',(-32.6814528967161,33.6200396292864,170.739352334667));
#27880=CARTESIAN_POINT('Ctrl Pts',(-33.0969984385428,33.2575455564586,170.77639559774));
#27881=CARTESIAN_POINT('Ctrl Pts',(-33.4525471239035,32.9473887190672,170.808090519624));
#27882=CARTESIAN_POINT('Ctrl Pts',(-33.6635508428324,32.4715325754067,170.839785441507));
#27883=CARTESIAN_POINT('Ctrl Pts',(-33.6674948241645,31.9987546321869,170.87148036339));
#27884=CARTESIAN_POINT('Origin',(-32.,32.,172.));
#27885=CARTESIAN_POINT('',(-33.6673389950091,32.0013000932747,171.57148036339));
#27886=CARTESIAN_POINT('',(-33.6637721760092,32.0008713647136,171.37851963661));
#27887=CARTESIAN_POINT('',(-33.666,32.,172.));
#27888=CARTESIAN_POINT('Ctrl Pts',(-33.6637721760092,32.0008713647136,171.37851963661));
#27889=CARTESIAN_POINT('Ctrl Pts',(-33.6648225918241,32.2223457019845,171.363756385255));
#27890=CARTESIAN_POINT('Ctrl Pts',(-33.6237242828597,32.4434460300688,171.348993133901));
#27891=CARTESIAN_POINT('Ctrl Pts',(-33.5386395641721,32.646076417136,171.334229882547));
#27892=CARTESIAN_POINT('Ctrl Pts',(-33.3251489487098,33.1545071519798,171.297186619474));
#27893=CARTESIAN_POINT('Ctrl Pts',(-32.8347264499723,33.5466538895163,171.2601433564));
#27894=CARTESIAN_POINT('Ctrl Pts',(-32.2917867441766,33.6430724089759,171.223100093327));
#27895=CARTESIAN_POINT('Ctrl Pts',(-31.7488470383809,33.7394909284354,171.186056830254));
#27896=CARTESIAN_POINT('Ctrl Pts',(-31.153390125527,33.5401812298181,171.149013567181));
#27897=CARTESIAN_POINT('Ctrl Pts',(-30.7778938602062,33.1363463504994,171.111970304107));
#27898=CARTESIAN_POINT('Ctrl Pts',(-30.4023975948853,32.7325114711806,171.074927041034));
#27899=CARTESIAN_POINT('Ctrl Pts',(-30.2468619770976,32.1241514111603,171.037883777961));
#27900=CARTESIAN_POINT('Ctrl Pts',(-30.3824592621858,31.5896484352088,171.000840514888));
#27901=CARTESIAN_POINT('Ctrl Pts',(-30.5180565472741,31.0551454592573,170.963797251814));
#27902=CARTESIAN_POINT('Ctrl Pts',(-30.9447867352383,30.5944995673746,170.926753988741));
#27903=CARTESIAN_POINT('Ctrl Pts',(-31.4673804059142,30.4184998219378,170.889710725668));
#27904=CARTESIAN_POINT('Ctrl Pts',(-31.9899740765901,30.242500076501,170.852667462595));
#27905=CARTESIAN_POINT('Ctrl Pts',(-32.6084312299776,30.3511464775101,170.815624199521));
#27906=CARTESIAN_POINT('Ctrl Pts',(-33.0397492261309,30.694723020974,170.778580936448));
#27907=CARTESIAN_POINT('Ctrl Pts',(-33.4281080958976,31.0040794570328,170.745227169835));
#27908=CARTESIAN_POINT('Ctrl Pts',(-33.6647493640718,31.5038986390065,170.711873403223));
#27909=CARTESIAN_POINT('Ctrl Pts',(-33.6681095326863,32.0009409351981,170.67851963661));
#27910=CARTESIAN_POINT('Ctrl Pts',(-33.6674948241645,31.9987546321869,170.87148036339));
#27911=CARTESIAN_POINT('Ctrl Pts',(-33.6681603490043,31.9189759926714,170.87682870458));
#27912=CARTESIAN_POINT('Ctrl Pts',(-33.6629299142687,31.8392850039256,170.88217704577));
#27913=CARTESIAN_POINT('Ctrl Pts',(-33.6515031400339,31.7604926322801,170.88752538696));
#27914=CARTESIAN_POINT('Ctrl Pts',(-33.5723599086977,31.214767061044,170.924568650033));
#27915=CARTESIAN_POINT('Ctrl Pts',(-33.1959710550246,30.7121491986861,170.961611913106));
#27916=CARTESIAN_POINT('Ctrl Pts',(-32.6945700775718,30.4826342536897,170.99865517618));
#27917=CARTESIAN_POINT('Ctrl Pts',(-32.193169100119,30.2531193086932,171.035698439253));
#27918=CARTESIAN_POINT('Ctrl Pts',(-31.5667559988865,30.2967072810581,171.072741702326));
#27919=CARTESIAN_POINT('Ctrl Pts',(-31.1019740124148,30.5934525509761,171.109784965399));
#27920=CARTESIAN_POINT('Ctrl Pts',(-30.6371920259431,30.8901978208941,171.146828228473));
#27921=CARTESIAN_POINT('Ctrl Pts',(-30.334041154232,31.4401003883653,171.183871491546));
#27922=CARTESIAN_POINT('Ctrl Pts',(-30.3312415924095,31.9915278202373,171.220914754619));
#27923=CARTESIAN_POINT('Ctrl Pts',(-30.328442030587,32.5429552521093,171.257958017692));
#27924=CARTESIAN_POINT('Ctrl Pts',(-30.625993778653,33.0959075483822,171.295001280766));
#27925=CARTESIAN_POINT('Ctrl Pts',(-31.0877387700997,33.3973567365404,171.332044543839));
#27926=CARTESIAN_POINT('Ctrl Pts',(-31.5494837615464,33.6988059246985,171.369087806912));
#27927=CARTESIAN_POINT('Ctrl Pts',(-32.1754219963737,33.7487520047421,171.406131069985));
#27928=CARTESIAN_POINT('Ctrl Pts',(-32.6791275323335,33.5243399212644,171.443174333058));
#27929=CARTESIAN_POINT('Ctrl Pts',(-33.1828330682934,33.2999278377868,171.480217596132));
#27930=CARTESIAN_POINT('Ctrl Pts',(-33.5643059053856,32.8011575907879,171.517260859205));
#27931=CARTESIAN_POINT('Ctrl Pts',(-33.6489861418072,32.2562637408254,171.554304122278));
#27932=CARTESIAN_POINT('Ctrl Pts',(-33.6620743350666,32.1720448449463,171.560029535982));
#27933=CARTESIAN_POINT('Ctrl Pts',(-33.6680724939006,32.0867241091558,171.565754949686));
#27934=CARTESIAN_POINT('Ctrl Pts',(-33.6673389950091,32.0013000932747,171.57148036339));
#27935=CARTESIAN_POINT('Origin',(-32.,32.,172.));
#27936=CARTESIAN_POINT('',(-33.6634138707132,32.0004190115247,172.27148036339));
#27937=CARTESIAN_POINT('',(-33.6649323100607,31.9985848365388,172.07851963661));
#27938=CARTESIAN_POINT('',(-33.666,32.,172.));
#27939=CARTESIAN_POINT('Ctrl Pts',(-33.6649323100607,31.9985848365388,172.07851963661));
#27940=CARTESIAN_POINT('Ctrl Pts',(-33.6618075397867,32.3855055154906,172.052682630362));
#27941=CARTESIAN_POINT('Ctrl Pts',(-33.5274443256813,32.7743832740356,172.026845624113));
#27942=CARTESIAN_POINT('Ctrl Pts',(-33.2809243517091,33.069607054209,172.001008617865));
#27943=CARTESIAN_POINT('Ctrl Pts',(-32.9274815355819,33.4928779258177,171.963965354792));
#27944=CARTESIAN_POINT('Ctrl Pts',(-32.3434916821162,33.7236356820849,171.926922091719));
#27945=CARTESIAN_POINT('Ctrl Pts',(-31.7961853817046,33.6562868249745,171.889878828646));
#27946=CARTESIAN_POINT('Ctrl Pts',(-31.248879081293,33.5889379678641,171.852835565572));
#27947=CARTESIAN_POINT('Ctrl Pts',(-30.7382563339356,33.2234824973761,171.815792302499));
#27948=CARTESIAN_POINT('Ctrl Pts',(-30.4979753400865,32.727150855206,171.778749039426));
#27949=CARTESIAN_POINT('Ctrl Pts',(-30.2576943462375,32.230819213036,171.741705776352));
#27950=CARTESIAN_POINT('Ctrl Pts',(-30.2877551058968,31.6036113991838,171.704662513279));
#27951=CARTESIAN_POINT('Ctrl Pts',(-30.5744019784421,31.1325343083757,171.667619250206));
#27952=CARTESIAN_POINT('Ctrl Pts',(-30.8610488509874,30.6614572175675,171.630575987133));
#27953=CARTESIAN_POINT('Ctrl Pts',(-31.4042818364187,30.3465108498032,171.59353272406));
#27954=CARTESIAN_POINT('Ctrl Pts',(-31.9555204661607,30.3318129552462,171.556489460986));
#27955=CARTESIAN_POINT('Ctrl Pts',(-32.5067590959028,30.3171150606892,171.519446197913));
#27956=CARTESIAN_POINT('Ctrl Pts',(-33.0660033699556,30.6026656393395,171.48240293484));
#27957=CARTESIAN_POINT('Ctrl Pts',(-33.3773461408885,31.0577982947402,171.445359671767));
#27958=CARTESIAN_POINT('Ctrl Pts',(-33.5646061177235,31.3315420217963,171.423079660048));
#27959=CARTESIAN_POINT('Ctrl Pts',(-33.662186937358,31.66663260447,171.400799648329));
#27960=CARTESIAN_POINT('Ctrl Pts',(-33.6637721760092,32.0008713647136,171.37851963661));
#27961=CARTESIAN_POINT('Ctrl Pts',(-33.6673389950091,32.0013000932747,171.57148036339));
#27962=CARTESIAN_POINT('Ctrl Pts',(-33.6633267770306,31.5340331672145,171.60279821276));
#27963=CARTESIAN_POINT('Ctrl Pts',(-33.4578994056388,31.0636760401785,171.634116062129));
#27964=CARTESIAN_POINT('Ctrl Pts',(-33.109710516809,30.7536577638475,171.665433911498));
#27965=CARTESIAN_POINT('Ctrl Pts',(-32.6978670196382,30.3869630897581,171.702477174571));
#27966=CARTESIAN_POINT('Ctrl Pts',(-32.0862923895458,30.2445911945054,171.739520437645));
#27967=CARTESIAN_POINT('Ctrl Pts',(-31.5548398611366,30.3916906853776,171.776563700718));
#27968=CARTESIAN_POINT('Ctrl Pts',(-31.0233873327274,30.5387901762498,171.813606963791));
#27969=CARTESIAN_POINT('Ctrl Pts',(-30.5720569060016,30.9753610532468,171.850650226864));
#27970=CARTESIAN_POINT('Ctrl Pts',(-30.4073749369914,31.5016308502619,171.887693489937));
#27971=CARTESIAN_POINT('Ctrl Pts',(-30.2426929679812,32.0279006472769,171.924736753011));
#27972=CARTESIAN_POINT('Ctrl Pts',(-30.3646594566867,32.64386936431,171.961780016084));
#27973=CARTESIAN_POINT('Ctrl Pts',(-30.717463199212,33.0676730563981,171.998823279157));
#27974=CARTESIAN_POINT('Ctrl Pts',(-31.0702669417373,33.4914767484861,172.03586654223));
#27975=CARTESIAN_POINT('Ctrl Pts',(-31.6539079380824,33.7231154156292,172.072909805304));
#27976=CARTESIAN_POINT('Ctrl Pts',(-32.2013152329814,33.6565924597509,172.109953068377));
#27977=CARTESIAN_POINT('Ctrl Pts',(-32.7487225278803,33.5900695038727,172.14699633145));
#27978=CARTESIAN_POINT('Ctrl Pts',(-33.259896121333,33.2253849249731,172.184039594523));
#27979=CARTESIAN_POINT('Ctrl Pts',(-33.500925748699,32.7294164089369,172.221082857597));
#27980=CARTESIAN_POINT('Ctrl Pts',(-33.6102330021986,32.5044940336146,172.237882026195));
#27981=CARTESIAN_POINT('Ctrl Pts',(-33.6639815170623,32.2525713515443,172.254681194792));
#27982=CARTESIAN_POINT('Ctrl Pts',(-33.6634138707132,32.0004190115247,172.27148036339));
#27983=CARTESIAN_POINT('Origin',(-32.,32.,172.));
#27984=CARTESIAN_POINT('',(-33.6658030887413,31.9984781517552,172.97148036339));
#27985=CARTESIAN_POINT('',(-33.6687792891636,31.9999631491883,172.77851963661));
#27986=CARTESIAN_POINT('',(-33.666,32.,172.));
#27987=CARTESIAN_POINT('Ctrl Pts',(-33.668778895518,31.9999631544077,172.77851963661));
#27988=CARTESIAN_POINT('Ctrl Pts',(-33.6686001028313,32.5494261614689,172.741608875468));
#27989=CARTESIAN_POINT('Ctrl Pts',(-33.3706978019218,33.0990553069806,172.704698114326));
#27990=CARTESIAN_POINT('Ctrl Pts',(-32.9101517435485,33.3987316572276,172.667787353184));
#27991=CARTESIAN_POINT('Ctrl Pts',(-32.4479524209175,33.6994837830451,172.63074409011));
#27992=CARTESIAN_POINT('Ctrl Pts',(-31.8219395305894,33.74848533579,172.593700827037));
#27993=CARTESIAN_POINT('Ctrl Pts',(-31.3185731767646,33.5233134706259,172.556657563964));
#27994=CARTESIAN_POINT('Ctrl Pts',(-30.8152068229398,33.2981416054618,172.519614300891));
#27995=CARTESIAN_POINT('Ctrl Pts',(-30.4344870056185,32.7987963223888,172.482571037817));
#27996=CARTESIAN_POINT('Ctrl Pts',(-30.3506290488396,32.2537753153541,172.445527774744));
#27997=CARTESIAN_POINT('Ctrl Pts',(-30.2667710920606,31.7087543083194,172.408484511671));
#27998=CARTESIAN_POINT('Ctrl Pts',(-30.4797749958241,31.1180575773228,172.371441248598));
#27999=CARTESIAN_POINT('Ctrl Pts',(-30.8921713287334,30.7519847435489,172.334397985524));
#28000=CARTESIAN_POINT('Ctrl Pts',(-31.3045676616427,30.385911909775,172.297354722451));
#28001=CARTESIAN_POINT('Ctrl Pts',(-31.9163564236978,30.2444629732237,172.260311459378));
#28002=CARTESIAN_POINT('Ctrl Pts',(-32.4475863946687,30.3923642002859,172.223268196305));
#28003=CARTESIAN_POINT('Ctrl Pts',(-32.9788163656397,30.5402654273481,172.186224933231));
#28004=CARTESIAN_POINT('Ctrl Pts',(-33.4294875455265,30.9775168180239,172.149181670158));
#28005=CARTESIAN_POINT('Ctrl Pts',(-33.5933752460756,31.5040345068369,172.112138407085));
#28006=CARTESIAN_POINT('Ctrl Pts',(-33.6429542385954,31.6633156271879,172.10093215026));
#28007=CARTESIAN_POINT('Ctrl Pts',(-33.666287613298,31.8307661481971,172.089725893435));
#28008=CARTESIAN_POINT('Ctrl Pts',(-33.6649323100607,31.9985848365388,172.07851963661));
#28009=CARTESIAN_POINT('Ctrl Pts',(-33.6634138707132,32.0004190115247,172.27148036339));
#28010=CARTESIAN_POINT('Ctrl Pts',(-33.6627298198179,31.6965589863211,172.291724457866));
#28011=CARTESIAN_POINT('Ctrl Pts',(-33.5831688020356,31.3923654559128,172.311968552341));
#28012=CARTESIAN_POINT('Ctrl Pts',(-33.4269052960693,31.1346863708554,172.332212646816));
#28013=CARTESIAN_POINT('Ctrl Pts',(-33.1409695547944,30.6631773019829,172.36925590989));
#28014=CARTESIAN_POINT('Ctrl Pts',(-32.5982124109655,30.347411617411,172.406299172963));
#28015=CARTESIAN_POINT('Ctrl Pts',(-32.0469965906205,30.3318819822315,172.443342436036));
#28016=CARTESIAN_POINT('Ctrl Pts',(-31.4957807702756,30.316352347052,172.480385699109));
#28017=CARTESIAN_POINT('Ctrl Pts',(-30.9361062734147,30.6010587612649,172.517428962183));
#28018=CARTESIAN_POINT('Ctrl Pts',(-30.6240771150927,31.0557211134827,172.554472225256));
#28019=CARTESIAN_POINT('Ctrl Pts',(-30.3120479567707,31.5103834657005,172.591515488329));
#28020=CARTESIAN_POINT('Ctrl Pts',(-30.2476641369877,32.1350017559232,172.628558751402));
#28021=CARTESIAN_POINT('Ctrl Pts',(-30.4603873425697,32.6437540413965,172.665602014475));
#28022=CARTESIAN_POINT('Ctrl Pts',(-30.6731105481516,33.1525063268697,172.702645277549));
#28023=CARTESIAN_POINT('Ctrl Pts',(-31.1629407790985,33.5453926075936,172.739688540622));
#28024=CARTESIAN_POINT('Ctrl Pts',(-31.7057343777229,33.642630251846,172.776731803695));
#28025=CARTESIAN_POINT('Ctrl Pts',(-32.2485279763472,33.7398678960985,172.813775066769));
#28026=CARTESIAN_POINT('Ctrl Pts',(-32.844284942649,33.5414569038794,172.850818329842));
#28027=CARTESIAN_POINT('Ctrl Pts',(-33.2203901192063,33.1381890693894,172.887861592915));
#28028=CARTESIAN_POINT('Ctrl Pts',(-33.5033876183818,32.8347532334267,172.915734516407));
#28029=CARTESIAN_POINT('Ctrl Pts',(-33.6620249438784,32.4153336737998,172.943607439899));
#28030=CARTESIAN_POINT('Ctrl Pts',(-33.6658030887413,31.9984781517552,172.97148036339));
#28031=CARTESIAN_POINT('Origin',(-32.,32.,172.));
#28032=CARTESIAN_POINT('',(-33.6685842971392,32.0005168033655,173.67148036339));
#28033=CARTESIAN_POINT('',(-33.6650396791624,32.0014384974592,173.47851963661));
#28034=CARTESIAN_POINT('',(-33.666,32.,172.));
#28035=CARTESIAN_POINT('Ctrl Pts',(-33.6650396791624,32.0014384974592,173.47851963661));
#28036=CARTESIAN_POINT('Ctrl Pts',(-33.666391096427,32.1652619019991,173.467578383647));
#28037=CARTESIAN_POINT('Ctrl Pts',(-33.6441694407878,32.3287266927861,173.456637130684));
#28038=CARTESIAN_POINT('Ctrl Pts',(-33.5968738601931,32.4845826243756,173.445695877722));
#28039=CARTESIAN_POINT('Ctrl Pts',(-33.4367475346125,33.0122564013253,173.408652614648));
#28040=CARTESIAN_POINT('Ctrl Pts',(-32.9892080319931,33.4527126246025,173.371609351575));
#28041=CARTESIAN_POINT('Ctrl Pts',(-32.4590470020517,33.60440091471,173.334566088502));
#28042=CARTESIAN_POINT('Ctrl Pts',(-31.9288859721102,33.7560892048175,173.297522825429));
#28043=CARTESIAN_POINT('Ctrl Pts',(-31.3161034148467,33.6190095617553,173.260479562355));
#28044=CARTESIAN_POINT('Ctrl Pts',(-30.9011053057899,33.2558888869052,173.223436299282));
#28045=CARTESIAN_POINT('Ctrl Pts',(-30.4861071967331,32.8927682120551,173.186393036209));
#28046=CARTESIAN_POINT('Ctrl Pts',(-30.268893535883,32.3036065054172,173.149349773136));
#28047=CARTESIAN_POINT('Ctrl Pts',(-30.3488601166525,31.7580009693526,173.112306510063));
#28048=CARTESIAN_POINT('Ctrl Pts',(-30.4288266974221,31.212395433288,173.075263246989));
#28049=CARTESIAN_POINT('Ctrl Pts',(-30.8059735198113,30.7103460677967,173.038219983916));
#28050=CARTESIAN_POINT('Ctrl Pts',(-31.3077202428883,30.4815879402783,173.001176720843));
#28051=CARTESIAN_POINT('Ctrl Pts',(-31.8094669659654,30.2528298127598,172.96413345777));
#28052=CARTESIAN_POINT('Ctrl Pts',(-32.4358135897303,30.2973629232142,172.927090194696));
#28053=CARTESIAN_POINT('Ctrl Pts',(-32.9001472953714,30.5948091617682,172.890046931623));
#28054=CARTESIAN_POINT('Ctrl Pts',(-33.3644810010125,30.8922554003222,172.85300366855));
#28055=CARTESIAN_POINT('Ctrl Pts',(-33.6668017885297,31.4426147669758,172.815960405477));
#28056=CARTESIAN_POINT('Ctrl Pts',(-33.6687693048215,31.9940457997478,172.778917142403));
#28057=CARTESIAN_POINT('Ctrl Pts',(-33.6687763425305,31.9960182414464,172.778784640472));
#28058=CARTESIAN_POINT('Ctrl Pts',(-33.6687795373464,31.9979906968566,172.778652138541));
#28059=CARTESIAN_POINT('Ctrl Pts',(-33.668778895518,31.9999631544077,172.77851963661));
#28060=CARTESIAN_POINT('Ctrl Pts',(-33.6658030887413,31.9984781517552,172.97148036339));
#28061=CARTESIAN_POINT('Ctrl Pts',(-33.6670461184289,31.8613304752761,172.980650702972));
#28062=CARTESIAN_POINT('Ctrl Pts',(-33.6515264953894,31.7244603417323,172.989821042553));
#28063=CARTESIAN_POINT('Ctrl Pts',(-33.6181580581719,31.5920895937741,172.998991382135));
#28064=CARTESIAN_POINT('Ctrl Pts',(-33.4833674337676,31.0573826294095,173.036034645208));
#28065=CARTESIAN_POINT('Ctrl Pts',(-33.0573327981464,30.596093377441,173.073077908281));
#28066=CARTESIAN_POINT('Ctrl Pts',(-32.535005290492,30.4193052983326,173.110121171354));
#28067=CARTESIAN_POINT('Ctrl Pts',(-32.0126777828375,30.2425172192242,173.147164434428));
#28068=CARTESIAN_POINT('Ctrl Pts',(-31.3940574031498,30.3502303129759,173.184207697501));
#28069=CARTESIAN_POINT('Ctrl Pts',(-30.9622214828446,30.6931556519368,173.221250960574));
#28070=CARTESIAN_POINT('Ctrl Pts',(-30.5303855625394,31.0360809908978,173.258294223647));
#28071=CARTESIAN_POINT('Ctrl Pts',(-30.2853341016167,31.614218575068,173.295337486721));
#28072=CARTESIAN_POINT('Ctrl Pts',(-30.3392013198585,32.1630157807517,173.332380749794));
#28073=CARTESIAN_POINT('Ctrl Pts',(-30.3930685381003,32.7118129864354,173.369424012867));
#28074=CARTESIAN_POINT('Ctrl Pts',(-30.7458544355066,33.2312698136326,173.40646727594));
#28075=CARTESIAN_POINT('Ctrl Pts',(-31.2361260983262,33.4836856348551,173.443510539014));
#28076=CARTESIAN_POINT('Ctrl Pts',(-31.7263977611457,33.7361014560777,173.480553802087));
#28077=CARTESIAN_POINT('Ctrl Pts',(-32.3541551893786,33.7214762713257,173.51759706516));
#28078=CARTESIAN_POINT('Ctrl Pts',(-32.8321399877382,33.4465024858399,173.554640328233));
#28079=CARTESIAN_POINT('Ctrl Pts',(-33.3101247860979,33.171528700354,173.591683591307));
#28080=CARTESIAN_POINT('Ctrl Pts',(-33.6383369545844,32.6362063141344,173.62872685438));
#28081=CARTESIAN_POINT('Ctrl Pts',(-33.6665883845547,32.0854959484502,173.665770117453));
#28082=CARTESIAN_POINT('Ctrl Pts',(-33.6680400440452,32.0571984806852,173.667673532765));
#28083=CARTESIAN_POINT('Ctrl Pts',(-33.6686997256412,32.028860384471,173.669576948078));
#28084=CARTESIAN_POINT('Ctrl Pts',(-33.6685842971392,32.0005168033655,173.67148036339));
#28085=CARTESIAN_POINT('Origin',(-32.,32.,172.));
#28086=CARTESIAN_POINT('',(-33.6642813207824,32.0011936551981,174.37148036339));
#28087=CARTESIAN_POINT('',(-33.6637114105544,31.9991832659222,174.17851963661));
#28088=CARTESIAN_POINT('',(-33.666,32.,172.));
#28089=CARTESIAN_POINT('Ctrl Pts',(-33.6637114105544,31.9991832659222,174.17851963661));
#28090=CARTESIAN_POINT('Ctrl Pts',(-33.6622464012834,32.329476700965,174.156504628753));
#28091=CARTESIAN_POINT('Ctrl Pts',(-33.5671323371198,32.6605477978972,174.134489620897));
#28092=CARTESIAN_POINT('Ctrl Pts',(-33.3840345732138,32.9323490469583,174.11247461304));
#28093=CARTESIAN_POINT('Ctrl Pts',(-33.0759475318338,33.3896918395745,174.075431349967));
#28094=CARTESIAN_POINT('Ctrl Pts',(-32.5187551705316,33.6792258851286,174.038388086894));
#28095=CARTESIAN_POINT('Ctrl Pts',(-31.9674256925893,33.668461974308,174.00134482382));
#28096=CARTESIAN_POINT('Ctrl Pts',(-31.416096214647,33.6576980634873,173.964301560747));
#28097=CARTESIAN_POINT('Ctrl Pts',(-30.8706296200645,33.346636196292,173.927258297674));
#28098=CARTESIAN_POINT('Ctrl Pts',(-30.5806284648534,32.8776165964877,173.890215034601));
#28099=CARTESIAN_POINT('Ctrl Pts',(-30.2906273096424,32.4085969966835,173.853171771527));
#28100=CARTESIAN_POINT('Ctrl Pts',(-30.2560915938026,31.7816196642703,173.816128508454));
#28101=CARTESIAN_POINT('Ctrl Pts',(-30.4928246736404,31.2835860269176,173.779085245381));
#28102=CARTESIAN_POINT('Ctrl Pts',(-30.7295577534781,30.7855523895648,173.742041982308));
#28103=CARTESIAN_POINT('Ctrl Pts',(-31.2375596289934,30.4164624472723,173.704998719234));
#28104=CARTESIAN_POINT('Ctrl Pts',(-31.7843713964759,30.3452097563264,173.667955456161));
#28105=CARTESIAN_POINT('Ctrl Pts',(-32.3311831639583,30.2739570653805,173.630912193088));
#28106=CARTESIAN_POINT('Ctrl Pts',(-32.9168048234079,30.5005416257811,173.593868930015));
#28107=CARTESIAN_POINT('Ctrl Pts',(-33.2732590788618,30.9212795712924,173.556825666941));
#28108=CARTESIAN_POINT('Ctrl Pts',(-33.5244295160179,31.217746599208,173.530723656831));
#28109=CARTESIAN_POINT('Ctrl Pts',(-33.6618156693323,31.6106130429878,173.50462164672));
#28110=CARTESIAN_POINT('Ctrl Pts',(-33.6650396791624,32.0014384974592,173.47851963661));
#28111=CARTESIAN_POINT('Ctrl Pts',(-33.6685842971392,32.0005168033655,173.67148036339));
#28112=CARTESIAN_POINT('Ctrl Pts',(-33.6664533171258,31.4772525853206,173.706620211151));
#28113=CARTESIAN_POINT('Ctrl Pts',(-33.400144713866,30.9521189740352,173.741760058912));
#28114=CARTESIAN_POINT('Ctrl Pts',(-32.9757931652251,30.6462444462039,173.776899906673));
#28115=CARTESIAN_POINT('Ctrl Pts',(-32.5284558244712,30.3238016547903,173.813943169746));
#28116=CARTESIAN_POINT('Ctrl Pts',(-31.9054904515093,30.2450144171118,173.850986432819));
#28117=CARTESIAN_POINT('Ctrl Pts',(-31.3919626231178,30.4459353459241,173.888029695893));
#28118=CARTESIAN_POINT('Ctrl Pts',(-30.8784347947262,30.6468562747363,173.925072958966));
#28119=CARTESIAN_POINT('Ctrl Pts',(-30.4743445109049,31.1274853700393,173.962116222039));
#28120=CARTESIAN_POINT('Ctrl Pts',(-30.3646012944423,31.6678893639252,173.999159485112));
#28121=CARTESIAN_POINT('Ctrl Pts',(-30.2548580779796,32.208293357811,174.036202748185));
#28122=CARTESIAN_POINT('Ctrl Pts',(-30.4394619288755,32.8084722502797,174.073246011259));
#28123=CARTESIAN_POINT('Ctrl Pts',(-30.8339391259327,33.1937874344721,174.110289274332));
#28124=CARTESIAN_POINT('Ctrl Pts',(-31.22841632299,33.5791026186644,174.147332537405));
#28125=CARTESIAN_POINT('Ctrl Pts',(-31.8327668662085,33.7495540945805,174.184375800478));
#28126=CARTESIAN_POINT('Ctrl Pts',(-32.3704432239659,33.6271441910758,174.221419063552));
#28127=CARTESIAN_POINT('Ctrl Pts',(-32.9081195817234,33.504734287571,174.258462326625));
#28128=CARTESIAN_POINT('Ctrl Pts',(-33.3791217540197,33.0894630046454,174.295505589698));
#28129=CARTESIAN_POINT('Ctrl Pts',(-33.567921700715,32.5713562296509,174.332548852771));
#28130=CARTESIAN_POINT('Ctrl Pts',(-33.6340629863343,32.389850626572,174.345526022978));
#28131=CARTESIAN_POINT('Ctrl Pts',(-33.6655703268436,32.1957242910376,174.358503193184));
#28132=CARTESIAN_POINT('Ctrl Pts',(-33.6642813207824,32.0011936551981,174.37148036339));
#28133=CARTESIAN_POINT('Origin',(-32.,32.,172.));
#28134=CARTESIAN_POINT('',(-33.6642763188368,31.998808699364,175.07148036339));
#28135=CARTESIAN_POINT('',(-33.668020664445,31.9990039308852,174.87851963661));
#28136=CARTESIAN_POINT('',(-33.666,32.,172.));
#28137=CARTESIAN_POINT('Ctrl Pts',(-33.668020664445,31.9990039308852,174.87851963661));
#28138=CARTESIAN_POINT('Ctrl Pts',(-33.6645338936159,32.4921662157297,174.845430873859));
#28139=CARTESIAN_POINT('Ctrl Pts',(-33.4321105820849,32.9881841512697,174.812342111109));
#28140=CARTESIAN_POINT('Ctrl Pts',(-33.0490371398972,33.2978241500031,174.779253348358));
#28141=CARTESIAN_POINT('Ctrl Pts',(-32.6201818695343,33.6444698078531,174.742210085285));
#28142=CARTESIAN_POINT('Ctrl Pts',(-32.0025157577357,33.7575267199113,174.705166822212));
#28143=CARTESIAN_POINT('Ctrl Pts',(-31.4786794681056,33.5852606562456,174.668123559139));
#28144=CARTESIAN_POINT('Ctrl Pts',(-30.9548431784755,33.4129945925799,174.631080296066));
#28145=CARTESIAN_POINT('Ctrl Pts',(-30.5248367110139,32.9554055531903,174.594037032992));
#28146=CARTESIAN_POINT('Ctrl Pts',(-30.3854286936181,32.4218838013281,174.556993769919));
#28147=CARTESIAN_POINT('Ctrl Pts',(-30.2460206762223,31.888362049466,174.519950506846));
#28148=CARTESIAN_POINT('Ctrl Pts',(-30.3972111088923,31.2789075851313,174.482907243773));
#28149=CARTESIAN_POINT('Ctrl Pts',(-30.7698160694345,30.8724034665744,174.445863980699));
#28150=CARTESIAN_POINT('Ctrl Pts',(-31.1424210299766,30.4658993480176,174.408820717626));
#28151=CARTESIAN_POINT('Ctrl Pts',(-31.7364405183908,30.2623455752385,174.371777454553));
#28152=CARTESIAN_POINT('Ctrl Pts',(-32.2800544377153,30.3548872509366,174.334734191479));
#28153=CARTESIAN_POINT('Ctrl Pts',(-32.8236683570397,30.4474289266347,174.297690928406));
#28154=CARTESIAN_POINT('Ctrl Pts',(-33.3168767072744,30.8360660508099,174.260647665333));
#28155=CARTESIAN_POINT('Ctrl Pts',(-33.5339900216629,31.3429603827367,174.22360440226));
#28156=CARTESIAN_POINT('Ctrl Pts',(-33.6220717409518,31.5486047227887,174.208576147043));
#28157=CARTESIAN_POINT('Ctrl Pts',(-33.6647114798417,31.7737128018398,174.193547891827));
#28158=CARTESIAN_POINT('Ctrl Pts',(-33.6637114105544,31.9991832659222,174.17851963661));
#28159=CARTESIAN_POINT('Ctrl Pts',(-33.6642813207824,32.0011936551981,174.37148036339));
#28160=CARTESIAN_POINT('Ctrl Pts',(-33.6618908659233,31.640437629564,174.395546456257));
#28161=CARTESIAN_POINT('Ctrl Pts',(-33.5467088410307,31.2782911543542,174.419612549124));
#28162=CARTESIAN_POINT('Ctrl Pts',(-33.3304552403725,30.9926692429498,174.443678641991));
#28163=CARTESIAN_POINT('Ctrl Pts',(-32.9975911122403,30.5530312983066,174.480721905064));
#28164=CARTESIAN_POINT('Ctrl Pts',(-32.4252651348816,30.2946976760834,174.517765168138));
#28165=CARTESIAN_POINT('Ctrl Pts',(-31.8753705722274,30.3358804410539,174.554808431211));
#28166=CARTESIAN_POINT('Ctrl Pts',(-31.3254760095731,30.3770632060244,174.591851694284));
#28167=CARTESIAN_POINT('Ctrl Pts',(-30.7980128616233,30.7177623581885,174.628894957357));
#28168=CARTESIAN_POINT('Ctrl Pts',(-30.5343454048299,31.2020758128803,174.665938220431));
#28169=CARTESIAN_POINT('Ctrl Pts',(-30.2706779480365,31.686389267572,174.702981483504));
#28170=CARTESIAN_POINT('Ctrl Pts',(-30.2708061823995,32.3143170247913,174.740024746577));
#28171=CARTESIAN_POINT('Ctrl Pts',(-30.5346714285698,32.7985227476312,174.77706800965));
#28172=CARTESIAN_POINT('Ctrl Pts',(-30.7985366747401,33.282728470471,174.814111272724));
#28173=CARTESIAN_POINT('Ctrl Pts',(-31.3261389327177,33.6232121589313,174.851154535797));
#28174=CARTESIAN_POINT('Ctrl Pts',(-31.876050270056,33.6641703233686,174.88819779887));
#28175=CARTESIAN_POINT('Ctrl Pts',(-32.4259616073944,33.7051284878059,174.925241061943));
#28176=CARTESIAN_POINT('Ctrl Pts',(-32.9981820240936,33.4465611282202,174.962284325017));
#28177=CARTESIAN_POINT('Ctrl Pts',(-33.3308665602081,33.0067872663347,174.99932758809));
#28178=CARTESIAN_POINT('Ctrl Pts',(-33.5468672630685,32.7212571230455,175.02337851319));
#28179=CARTESIAN_POINT('Ctrl Pts',(-33.6618925440441,32.3593400811699,175.04742943829));
#28180=CARTESIAN_POINT('Ctrl Pts',(-33.6642763188368,31.998808699364,175.07148036339));
#28181=CARTESIAN_POINT('Origin',(-32.,32.,172.));
#28182=CARTESIAN_POINT('',(-33.6685813165324,31.9994792732742,175.77148036339));
#28183=CARTESIAN_POINT('',(-33.6667309775204,32.001451384792,175.57851963661));
#28184=CARTESIAN_POINT('',(-33.666,32.,172.));
#28185=CARTESIAN_POINT('Ctrl Pts',(-33.6667309775204,32.001451384792,175.57851963661));
#28186=CARTESIAN_POINT('Ctrl Pts',(-33.6677032442523,32.1077720165447,175.571400382039));
#28187=CARTESIAN_POINT('Ctrl Pts',(-33.6584012903311,32.2139231749333,175.564281127468));
#28188=CARTESIAN_POINT('Ctrl Pts',(-33.638208635078,32.3179605528532,175.557161872896));
#28189=CARTESIAN_POINT('Ctrl Pts',(-33.5331411967364,32.859293064739,175.520118609823));
#28190=CARTESIAN_POINT('Ctrl Pts',(-33.1332209461614,33.3433974793115,175.48307534675));
#28191=CARTESIAN_POINT('Ctrl Pts',(-32.6214492215387,33.5487502414089,175.446032083677));
#28192=CARTESIAN_POINT('Ctrl Pts',(-32.1096774969161,33.7541030035063,175.408988820604));
#28193=CARTESIAN_POINT('Ctrl Pts',(-31.4860542982457,33.6807041131287,175.37194555753));
#28194=CARTESIAN_POINT('Ctrl Pts',(-31.0359462197833,33.362140504524,175.334902294457));
#28195=CARTESIAN_POINT('Ctrl Pts',(-30.5858381413209,33.0435768959193,175.297859031384));
#28196=CARTESIAN_POINT('Ctrl Pts',(-30.3092451830665,32.4798485690876,175.26081576831));
#28197=CARTESIAN_POINT('Ctrl Pts',(-30.3327347829544,31.9289145496975,175.223772505237));
#28198=CARTESIAN_POINT('Ctrl Pts',(-30.3562243828422,31.3779805303073,175.186729242164));
#28199=CARTESIAN_POINT('Ctrl Pts',(-30.6797965408723,30.8398408183586,175.149685979091));
#28200=CARTESIAN_POINT('Ctrl Pts',(-31.1553863920272,30.5607452280982,175.112642716018));
#28201=CARTESIAN_POINT('Ctrl Pts',(-31.630976243182,30.2816496378377,175.075599452944));
#28202=CARTESIAN_POINT('Ctrl Pts',(-32.2585837874615,30.2615981692654,175.038556189871));
#28203=CARTESIAN_POINT('Ctrl Pts',(-32.7510192156636,30.5097662656754,175.001512926798));
#28204=CARTESIAN_POINT('Ctrl Pts',(-33.2434546438656,30.7579343620854,174.964469663725));
#28205=CARTESIAN_POINT('Ctrl Pts',(-33.6007179559903,31.2743220234776,174.927426400651));
#28206=CARTESIAN_POINT('Ctrl Pts',(-33.6593273975889,31.8226330559946,174.890383137578));
#28207=CARTESIAN_POINT('Ctrl Pts',(-33.6655841643122,31.8811672124153,174.886428637255));
#28208=CARTESIAN_POINT('Ctrl Pts',(-33.6684373749903,31.9400651778922,174.882474136933));
#28209=CARTESIAN_POINT('Ctrl Pts',(-33.668020664445,31.9990039308852,174.87851963661));
#28210=CARTESIAN_POINT('Ctrl Pts',(-33.6642763188368,31.998808699364,175.07148036339));
#28211=CARTESIAN_POINT('Ctrl Pts',(-33.6655640367782,31.8040492236754,175.084472701363));
#28212=CARTESIAN_POINT('Ctrl Pts',(-33.6339810135813,31.6096941075785,175.097465039336));
#28213=CARTESIAN_POINT('Ctrl Pts',(-33.5676882071046,31.4280034213046,175.11045737731));
#28214=CARTESIAN_POINT('Ctrl Pts',(-33.3786766623567,30.909973802345,175.147500640383));
#28215=CARTESIAN_POINT('Ctrl Pts',(-32.9075049173313,30.494894928611,175.184543903456));
#28216=CARTESIAN_POINT('Ctrl Pts',(-32.3697786077296,30.3727046420518,175.221587166529));
#28217=CARTESIAN_POINT('Ctrl Pts',(-31.8320522981278,30.2505143554927,175.258630429603));
#28218=CARTESIAN_POINT('Ctrl Pts',(-31.2277714239497,30.4212126561084,175.295673692676));
#28219=CARTESIAN_POINT('Ctrl Pts',(-30.8334516366425,30.80668892711,175.332716955749));
#28220=CARTESIAN_POINT('Ctrl Pts',(-30.4391318493354,31.1921651981116,175.369760218822));
#28221=CARTESIAN_POINT('Ctrl Pts',(-30.2547731488991,31.7924194394991,175.406803481895));
#28222=CARTESIAN_POINT('Ctrl Pts',(-30.36473707701,32.3327785651572,175.443846744969));
#28223=CARTESIAN_POINT('Ctrl Pts',(-30.4747010051209,32.8731376908152,175.480890008042));
#28224=CARTESIAN_POINT('Ctrl Pts',(-30.878987561779,33.3536017007438,175.517933271115));
#28225=CARTESIAN_POINT('Ctrl Pts',(-31.39259741081,33.5543128692062,175.554976534188));
#28226=CARTESIAN_POINT('Ctrl Pts',(-31.906207259841,33.7550240376686,175.592019797262));
#28227=CARTESIAN_POINT('Ctrl Pts',(-32.5291404012448,33.6759823646648,175.629063060335));
#28228=CARTESIAN_POINT('Ctrl Pts',(-32.9763460072298,33.3533568911779,175.666106323408));
#28229=CARTESIAN_POINT('Ctrl Pts',(-33.4003894769072,33.0474411706394,175.701231003402));
#28230=CARTESIAN_POINT('Ctrl Pts',(-33.6664369441154,32.5225201209083,175.736355683396));
#28231=CARTESIAN_POINT('Ctrl Pts',(-33.6685813165324,31.9994792732742,175.77148036339));
#28232=CARTESIAN_POINT('Origin',(-32.,32.,172.));
#28233=CARTESIAN_POINT('',(-33.665809879668,32.0015219961349,176.47148036339));
#28234=CARTESIAN_POINT('',(-33.6633199598622,32.0000809155407,176.27851963661));
#28235=CARTESIAN_POINT('',(-33.666,32.,172.));
#28236=CARTESIAN_POINT('Ctrl Pts',(-33.6633199598622,32.0000809155407,176.27851963661));
#28237=CARTESIAN_POINT('Ctrl Pts',(-33.6634382983753,32.2731930234702,176.260326627145));
#28238=CARTESIAN_POINT('Ctrl Pts',(-33.599931290633,32.5462533007021,176.24213361768));
#28239=CARTESIAN_POINT('Ctrl Pts',(-33.472497725772,32.7852241035491,176.223940608215));
#28240=CARTESIAN_POINT('Ctrl Pts',(-33.2130269066871,33.2717988142213,176.186897345141));
#28241=CARTESIAN_POINT('Ctrl Pts',(-32.6885287363003,33.6170450456087,176.149854082068));
#28242=CARTESIAN_POINT('Ctrl Pts',(-32.1390107333948,33.6629799942341,176.112810818995));
#28243=CARTESIAN_POINT('Ctrl Pts',(-31.5894927304893,33.7089149428595,176.075767555922));
#28244=CARTESIAN_POINT('Ctrl Pts',(-31.0149548950651,33.4555386087229,176.038724292849));
#28245=CARTESIAN_POINT('Ctrl Pts',(-30.6783026253169,33.0187946284562,176.001681029775));
#28246=CARTESIAN_POINT('Ctrl Pts',(-30.3416503555688,32.5820506481895,175.964637766702));
#28247=CARTESIAN_POINT('Ctrl Pts',(-30.2428836514968,31.9619390217927,175.927594503629));
#28248=CARTESIAN_POINT('Ctrl Pts',(-30.4271976213409,31.4422194670863,175.890551240556));
#28249=CARTESIAN_POINT('Ctrl Pts',(-30.6115115911851,30.9224999123798,175.853507977482));
#28250=CARTESIAN_POINT('Ctrl Pts',(-31.0789062349454,30.5031724293638,175.816464714409));
#28251=CARTESIAN_POINT('Ctrl Pts',(-31.6155042979806,30.3761190005593,175.779421451336));
#28252=CARTESIAN_POINT('Ctrl Pts',(-32.1521023610158,30.2490655717549,175.742378188263));
#28253=CARTESIAN_POINT('Ctrl Pts',(-32.757903843326,30.414286197162,175.705334925189));
#28254=CARTESIAN_POINT('Ctrl Pts',(-33.1556972714269,30.7961768144651,175.668291662116));
#28255=CARTESIAN_POINT('Ctrl Pts',(-33.4770397487634,31.1046728035055,175.638367653614));
#28256=CARTESIAN_POINT('Ctrl Pts',(-33.6626442971441,31.5545591635997,175.608443645112));
#28257=CARTESIAN_POINT('Ctrl Pts',(-33.6667309775204,32.001451384792,175.57851963661));
#28258=CARTESIAN_POINT('Ctrl Pts',(-33.6685813165324,31.9994792732742,175.77148036339));
#28259=CARTESIAN_POINT('Ctrl Pts',(-33.668698446614,31.9709096942721,175.773398946469));
#28260=CARTESIAN_POINT('Ctrl Pts',(-33.6680282029118,31.9423457249876,175.775317529549));
#28261=CARTESIAN_POINT('Ctrl Pts',(-33.6665533258647,31.9138233628901,175.777236112628));
#28262=CARTESIAN_POINT('Ctrl Pts',(-33.6380769679487,31.3631245820592,175.814279375701));
#28263=CARTESIAN_POINT('Ctrl Pts',(-33.3096461815507,30.8279362943673,175.851322638774));
#28264=CARTESIAN_POINT('Ctrl Pts',(-32.8315491136859,30.553157758334,175.888365901848));
#28265=CARTESIAN_POINT('Ctrl Pts',(-32.3534520458211,30.2783792223007,175.925409164921));
#28266=CARTESIAN_POINT('Ctrl Pts',(-31.7256886964896,30.264010437926,175.962452427994));
#28267=CARTESIAN_POINT('Ctrl Pts',(-31.2355201704377,30.5166264830092,175.999495691067));
#28268=CARTESIAN_POINT('Ctrl Pts',(-30.7453516443858,30.7692425280923,176.036538954141));
#28269=CARTESIAN_POINT('Ctrl Pts',(-30.3927779416135,31.2888434026335,176.073582217214));
#28270=CARTESIAN_POINT('Ctrl Pts',(-30.3391348767637,31.8376625638996,176.110625480287));
#28271=CARTESIAN_POINT('Ctrl Pts',(-30.2854918119139,32.3864817251657,176.14766874336));
#28272=CARTESIAN_POINT('Ctrl Pts',(-30.5307793849866,32.9645191731569,176.184712006434));
#28273=CARTESIAN_POINT('Ctrl Pts',(-30.9627553325488,33.3072681058711,176.221755269507));
#28274=CARTESIAN_POINT('Ctrl Pts',(-31.3947312801111,33.6500170385854,176.25879853258));
#28275=CARTESIAN_POINT('Ctrl Pts',(-32.0133956021629,33.7574774560227,176.295841795653));
#28276=CARTESIAN_POINT('Ctrl Pts',(-32.535650859524,33.5804760540039,176.332885058727));
#28277=CARTESIAN_POINT('Ctrl Pts',(-33.0579061168852,33.4034746519851,176.3699283218));
#28278=CARTESIAN_POINT('Ctrl Pts',(-33.4837523095557,32.9420114305103,176.406971584873));
#28279=CARTESIAN_POINT('Ctrl Pts',(-33.6183245287774,32.4072494572197,176.444014847946));
#28280=CARTESIAN_POINT('Ctrl Pts',(-33.6515837960838,32.2750840554909,176.453170019761));
#28281=CARTESIAN_POINT('Ctrl Pts',(-33.6670514141996,32.1384414062313,176.462325191576));
#28282=CARTESIAN_POINT('Ctrl Pts',(-33.665809879668,32.0015219961349,176.47148036339));
#28283=CARTESIAN_POINT('Origin',(-32.,32.,172.));
#28284=CARTESIAN_POINT('',(-33.6634121676067,31.9995845740168,177.17148036339));
#28285=CARTESIAN_POINT('',(-33.6664340315428,31.9985061125431,176.97851963661));
#28286=CARTESIAN_POINT('',(-33.666,32.,172.));
#28287=CARTESIAN_POINT('Ctrl Pts',(-33.6664340315428,31.9985061125431,176.97851963661));
#28288=CARTESIAN_POINT('Ctrl Pts',(-33.662398201977,32.435783313381,176.949252872251));
#28289=CARTESIAN_POINT('Ctrl Pts',(-33.4857164328592,32.875946937287,176.919986107892));
#28290=CARTESIAN_POINT('Ctrl Pts',(-33.1768207039935,33.1831819279473,176.890719343533));
#28291=CARTESIAN_POINT('Ctrl Pts',(-32.785848008609,33.5720526088596,176.85367608046));
#28292=CARTESIAN_POINT('Ctrl Pts',(-32.183065360919,33.747968413286,176.816632817387));
#28293=CARTESIAN_POINT('Ctrl Pts',(-31.6443028311243,33.6304312219835,176.779589554314));
#28294=CARTESIAN_POINT('Ctrl Pts',(-31.1055403013296,33.512894030681,176.74254629124));
#28295=CARTESIAN_POINT('Ctrl Pts',(-30.6307978894302,33.1019038436494,176.705503028167));
#28296=CARTESIAN_POINT('Ctrl Pts',(-30.4373151493842,32.5855275424649,176.668459765094));
#28297=CARTESIAN_POINT('Ctrl Pts',(-30.2438324093381,32.0691512412803,176.63141650202));
#28298=CARTESIAN_POINT('Ctrl Pts',(-30.3316093411455,31.4473888259428,176.594373238947));
#28299=CARTESIAN_POINT('Ctrl Pts',(-30.6604796965375,31.0047554061028,176.557329975874));
#28300=CARTESIAN_POINT('Ctrl Pts',(-30.9893500519296,30.5621219862628,176.520286712801));
#28301=CARTESIAN_POINT('Ctrl Pts',(-31.5593138309064,30.2986175619204,176.483243449727));
#28302=CARTESIAN_POINT('Ctrl Pts',(-32.1095586988182,30.3348203289801,176.446200186654));
#28303=CARTESIAN_POINT('Ctrl Pts',(-32.65980356673,30.3710230960397,176.409156923581));
#28304=CARTESIAN_POINT('Ctrl Pts',(-33.1903295235767,30.7069330545014,176.372113660508));
#28305=CARTESIAN_POINT('Ctrl Pts',(-33.4583707681085,31.1888396287107,176.335070397435));
#28306=CARTESIAN_POINT('Ctrl Pts',(-33.594769265911,31.4340680558438,176.316220143826));
#28307=CARTESIAN_POINT('Ctrl Pts',(-33.6631973462292,31.7171023073089,176.297369890218));
#28308=CARTESIAN_POINT('Ctrl Pts',(-33.6633199598622,32.0000809155407,176.27851963661));
#28309=CARTESIAN_POINT('Ctrl Pts',(-33.665809879668,32.0015219961349,176.47148036339));
#28310=CARTESIAN_POINT('Ctrl Pts',(-33.6620279704892,31.5844439684211,176.499368454649));
#28311=CARTESIAN_POINT('Ctrl Pts',(-33.5032006168982,31.1647978567452,176.527256545907));
#28312=CARTESIAN_POINT('Ctrl Pts',(-33.2199251392459,30.8613125733022,176.555144637166));
#28313=CARTESIAN_POINT('Ctrl Pts',(-32.8436552847201,30.4581983877814,176.592187900239));
#28314=CARTESIAN_POINT('Ctrl Pts',(-32.2478173298955,30.2600307418458,176.629231163313));
#28315=CARTESIAN_POINT('Ctrl Pts',(-31.7050634919084,30.3574900744037,176.666274426386));
#28316=CARTESIAN_POINT('Ctrl Pts',(-31.1623096539213,30.4549494069617,176.703317689459));
#28317=CARTESIAN_POINT('Ctrl Pts',(-30.6726399327717,30.8480357180132,176.740360952532));
#28318=CARTESIAN_POINT('Ctrl Pts',(-30.4601245381307,31.3568748457966,176.777404215605));
#28319=CARTESIAN_POINT('Ctrl Pts',(-30.2476091434896,31.86571397358,176.814447478679));
#28320=CARTESIAN_POINT('Ctrl Pts',(-30.3122480753572,32.4903059180951,176.851490741752));
#28321=CARTESIAN_POINT('Ctrl Pts',(-30.6244629081934,32.9448407866344,176.888534004825));
#28322=CARTESIAN_POINT('Ctrl Pts',(-30.9366777410296,33.3993756551737,176.925577267898));
#28323=CARTESIAN_POINT('Ctrl Pts',(-31.4964684748346,33.6838534477371,176.962620530972));
#28324=CARTESIAN_POINT('Ctrl Pts',(-32.0476779068016,33.6680986803785,176.999663794045));
#28325=CARTESIAN_POINT('Ctrl Pts',(-32.5988873387685,33.6523439130199,177.036707057118));
#28326=CARTESIAN_POINT('Ctrl Pts',(-33.1415154688975,33.3363565857395,177.073750320191));
#28327=CARTESIAN_POINT('Ctrl Pts',(-33.4272586037737,32.8647307628914,177.110793583265));
#28328=CARTESIAN_POINT('Ctrl Pts',(-33.5832998499633,32.6071809842615,177.131022509973));
#28329=CARTESIAN_POINT('Ctrl Pts',(-33.6627345384754,32.3032177147393,177.151251436682));
#28330=CARTESIAN_POINT('Ctrl Pts',(-33.6634121676067,31.9995845740168,177.17148036339));
#28331=CARTESIAN_POINT('Origin',(-32.,32.,172.));
#28332=CARTESIAN_POINT('',(-33.6673324606655,31.9986966424362,177.87148036339));
#28333=CARTESIAN_POINT('',(-33.6682332709748,32.0008552724336,177.67851963661));
#28334=CARTESIAN_POINT('',(-33.666,32.,172.));
#28335=CARTESIAN_POINT('Ctrl Pts',(-33.6682332709748,32.0008552724336,177.67851963661));
#28336=CARTESIAN_POINT('Ctrl Pts',(-33.6685408240927,32.049981824342,177.67522238043));
#28337=CARTESIAN_POINT('Ctrl Pts',(-33.6665588175026,32.0990832102901,177.671925124251));
#28338=CARTESIAN_POINT('Ctrl Pts',(-33.6622064848019,32.1479735833227,177.668627868071));
#28339=CARTESIAN_POINT('Ctrl Pts',(-33.613309888227,32.6972360159009,177.631584604998));
#28340=CARTESIAN_POINT('Ctrl Pts',(-33.2652411222702,33.2198653234349,177.594541341925));
#28341=CARTESIAN_POINT('Ctrl Pts',(-32.7772747016725,33.4767093138507,177.557498078852));
#28342=CARTESIAN_POINT('Ctrl Pts',(-32.2893082810747,33.7335533042664,177.520454815778));
#28343=CARTESIAN_POINT('Ctrl Pts',(-31.6614442058359,33.7246119775639,177.483411552705));
#28344=CARTESIAN_POINT('Ctrl Pts',(-31.1809896061435,33.4539767650361,177.446368289632));
#28345=CARTESIAN_POINT('Ctrl Pts',(-30.700535006451,33.1833415525083,177.409325026559));
#28346=CARTESIAN_POINT('Ctrl Pts',(-30.3674898823049,32.6510124541552,177.372281763485));
#28347=CARTESIAN_POINT('Ctrl Pts',(-30.3342539091629,32.1005804139805,177.335238500412));
#28348=CARTESIAN_POINT('Ctrl Pts',(-30.3010179360208,31.5501483738058,177.298195237339));
#28349=CARTESIAN_POINT('Ctrl Pts',(-30.5675911138828,30.9816133918094,177.261151974266));
#28350=CARTESIAN_POINT('Ctrl Pts',(-31.0119909860241,30.6551339757941,177.224108711192));
#28351=CARTESIAN_POINT('Ctrl Pts',(-31.4563908581654,30.3286545597788,177.187065448119));
#28352=CARTESIAN_POINT('Ctrl Pts',(-32.0786174245861,30.2442307097446,177.150022185046));
#28353=CARTESIAN_POINT('Ctrl Pts',(-32.593943190218,30.4404943301489,177.112978921973));
#28354=CARTESIAN_POINT('Ctrl Pts',(-33.1092689558498,30.6367579505533,177.075935658899));
#28355=CARTESIAN_POINT('Ctrl Pts',(-33.5176939206928,31.1137090413961,177.038892395826));
#28356=CARTESIAN_POINT('Ctrl Pts',(-33.6323250315748,31.6530973655166,177.001849132753));
#28357=CARTESIAN_POINT('Ctrl Pts',(-33.6563895607886,31.766331251008,176.994072634039));
#28358=CARTESIAN_POINT('Ctrl Pts',(-33.6675063955064,31.8823167877364,176.986296135324));
#28359=CARTESIAN_POINT('Ctrl Pts',(-33.6664340315428,31.9985061125431,176.97851963661));
#28360=CARTESIAN_POINT('Ctrl Pts',(-33.6634121676067,31.9995845740168,177.17148036339));
#28361=CARTESIAN_POINT('Ctrl Pts',(-33.6639754146988,31.7472039196625,177.188294699755));
#28362=CARTESIAN_POINT('Ctrl Pts',(-33.6101255864195,31.4950513505542,177.20510903612));
#28363=CARTESIAN_POINT('Ctrl Pts',(-33.500627701242,31.2699706058666,177.221923372484));
#28364=CARTESIAN_POINT('Ctrl Pts',(-33.2593955242106,30.7741005901055,177.258966635558));
#28365=CARTESIAN_POINT('Ctrl Pts',(-32.7480730305246,30.4096248769989,177.296009898631));
#28366=CARTESIAN_POINT('Ctrl Pts',(-32.2006386068928,30.3433254802472,177.333053161704));
#28367=CARTESIAN_POINT('Ctrl Pts',(-31.6532041832609,30.2770260834956,177.370096424777));
#28368=CARTESIAN_POINT('Ctrl Pts',(-31.0696578296832,30.5089030030988,177.407139687851));
#28369=CARTESIAN_POINT('Ctrl Pts',(-30.7170272216495,30.9328508140707,177.444182950924));
#28370=CARTESIAN_POINT('Ctrl Pts',(-30.3643966136158,31.3567986250425,177.481226213997));
#28371=CARTESIAN_POINT('Ctrl Pts',(-30.2426817511261,31.972817327383,177.51826947707));
#28372=CARTESIAN_POINT('Ctrl Pts',(-30.4075786377867,32.4990197038229,177.555312740144));
#28373=CARTESIAN_POINT('Ctrl Pts',(-30.5724755244473,33.0252220802628,177.592356003217));
#28374=CARTESIAN_POINT('Ctrl Pts',(-31.0239841602582,33.4616081308021,177.62939926629));
#28375=CARTESIAN_POINT('Ctrl Pts',(-31.5554967587389,33.608490777879,177.666442529363));
#28376=CARTESIAN_POINT('Ctrl Pts',(-32.0870093572195,33.7553734249558,177.703485792437));
#28377=CARTESIAN_POINT('Ctrl Pts',(-32.6985259183698,33.6127526685702,177.74052905551));
#28378=CARTESIAN_POINT('Ctrl Pts',(-33.1102195412827,33.2458893383607,177.777572318583));
#28379=CARTESIAN_POINT('Ctrl Pts',(-33.4581131480177,32.9358786896109,177.808875000185));
#28380=CARTESIAN_POINT('Ctrl Pts',(-33.663317931488,32.4657417347074,177.840177681788));
#28381=CARTESIAN_POINT('Ctrl Pts',(-33.6673324606655,31.9986966424362,177.87148036339));
#28382=CARTESIAN_POINT('Origin',(-32.,32.,172.));
#28383=CARTESIAN_POINT('',(-33.6674973548511,32.0012179185931,178.57148036339));
#28384=CARTESIAN_POINT('',(-33.6638666530066,32.0009462971081,178.37851963661));
#28385=CARTESIAN_POINT('',(-33.666,32.,172.));
#28386=CARTESIAN_POINT('',(-30.7309291201471,33.0793586530479,179.));
#28387=CARTESIAN_POINT('Ctrl Pts',(-33.6674973548511,32.0012179185931,178.57148036339));
#28388=CARTESIAN_POINT('Ctrl Pts',(-33.6635706604874,31.5283160997714,178.60319045304));
#28389=CARTESIAN_POINT('Ctrl Pts',(-33.4523668182224,31.0524200665679,178.634900542691));
#28390=CARTESIAN_POINT('Ctrl Pts',(-33.0965044878972,30.7421391403554,178.666610632341));
#28391=CARTESIAN_POINT('Ctrl Pts',(-32.6807913169313,30.3796734991954,178.703653895414));
#28392=CARTESIAN_POINT('Ctrl Pts',(-32.067668916338,30.2432156860183,178.740697158487));
#28393=CARTESIAN_POINT('Ctrl Pts',(-31.5378405764127,30.3962148457825,178.777740421561));
#28394=CARTESIAN_POINT('Ctrl Pts',(-31.0080122364874,30.5492140055468,178.814783684634));
#28395=CARTESIAN_POINT('Ctrl Pts',(-30.5614779572301,30.9916701382525,178.851826947707));
#28396=CARTESIAN_POINT('Ctrl Pts',(-30.402485611048,31.5187149254341,178.88887021078));
#28397=CARTESIAN_POINT('Ctrl Pts',(-30.243493264866,32.0457597126157,178.925913473853));
#28398=CARTESIAN_POINT('Ctrl Pts',(-30.3720428517591,32.6573931542732,178.962956736927));
#28399=CARTESIAN_POINT('Ctrl Pts',(-30.7309291201472,33.079358653048,179.));
#28400=CARTESIAN_POINT('',(-33.2714881269984,33.0811958775516,179.));
#28401=CARTESIAN_POINT('Origin',(-32.,32.,179.));
#28402=CARTESIAN_POINT('Ctrl Pts',(-33.2714899453064,33.0811972595532,179.));
#28403=CARTESIAN_POINT('Ctrl Pts',(-32.9207087126724,33.49260263365,178.963685183163));
#28404=CARTESIAN_POINT('Ctrl Pts',(-32.3509044879416,33.7187060857981,178.927370366326));
#28405=CARTESIAN_POINT('Ctrl Pts',(-31.8135987875986,33.6582492875696,178.891055549488));
#28406=CARTESIAN_POINT('Ctrl Pts',(-31.2655151638324,33.5965797742307,178.854012286415));
#28407=CARTESIAN_POINT('Ctrl Pts',(-30.7512469298483,33.2367383670875,178.816969023342));
#28408=CARTESIAN_POINT('Ctrl Pts',(-30.5057843969245,32.7430232880388,178.779925760268));
#28409=CARTESIAN_POINT('Ctrl Pts',(-30.2603218640006,32.2493082089901,178.742882497195));
#28410=CARTESIAN_POINT('Ctrl Pts',(-30.283665032137,31.6217194580359,178.705839234122));
#28411=CARTESIAN_POINT('Ctrl Pts',(-30.5652971510249,31.147616030279,178.668795971049));
#28412=CARTESIAN_POINT('Ctrl Pts',(-30.8469292699128,30.673512602522,178.631752707976));
#28413=CARTESIAN_POINT('Ctrl Pts',(-31.3868503395524,30.3528944979624,178.594709444902));
#28414=CARTESIAN_POINT('Ctrl Pts',(-31.9379143943192,30.3323875246469,178.557666181829));
#28415=CARTESIAN_POINT('Ctrl Pts',(-32.488978449086,30.3118805513313,178.520622918756));
#28416=CARTESIAN_POINT('Ctrl Pts',(-33.05118548898,30.5914847092598,178.483579655683));
#28417=CARTESIAN_POINT('Ctrl Pts',(-33.3673124104994,31.0432975272097,178.44653639261));
#28418=CARTESIAN_POINT('Ctrl Pts',(-33.5607972342972,31.3198286212731,178.42386414061));
#28419=CARTESIAN_POINT('Ctrl Pts',(-33.6620997929986,31.6608695361818,178.40119188861));
#28420=CARTESIAN_POINT('Ctrl Pts',(-33.6638666530066,32.0009462971081,178.37851963661));
#28421=CARTESIAN_POINT('Origin',(-32.,32.,180.545925280538));
#28422=CARTESIAN_POINT('',(-34.0533144349913,32.0018139164182,166.254074719462));
#28423=CARTESIAN_POINT('',(-34.0546693143771,31.9981396895887,166.195925280538));
#28424=CARTESIAN_POINT('',(-34.05475,32.0000000000002,180.545925280538));
#28425=CARTESIAN_POINT('',(-31.6163320011528,34.0186125009919,166.));
#28426=CARTESIAN_POINT('Ctrl Pts',(-34.0546693143771,31.9981396895887,166.195925280538));
#28427=CARTESIAN_POINT('Ctrl Pts',(-34.0494207118803,32.5195349242374,166.167660116765));
#28428=CARTESIAN_POINT('Ctrl Pts',(-33.5818272109704,33.7318555427796,166.102351689919));
#28429=CARTESIAN_POINT('Ctrl Pts',(-32.2875197530244,34.146181938655,166.037043263073));
#28430=CARTESIAN_POINT('Ctrl Pts',(-31.6163320011528,34.0186125009919,166.));
#28431=CARTESIAN_POINT('',(-30.6584058692254,33.5612502425942,166.));
#28432=CARTESIAN_POINT('Origin',(-32.,32.,166.));
#28433=CARTESIAN_POINT('Ctrl Pts',(-34.0533144349913,32.0018139164182,166.254074719462));
#28434=CARTESIAN_POINT('Ctrl Pts',(-34.0549811521398,32.2111665085478,166.242741226219));
#28435=CARTESIAN_POINT('Ctrl Pts',(-33.9292853981704,33.1027772342694,166.194364469902));
#28436=CARTESIAN_POINT('Ctrl Pts',(-32.6547057991862,34.3307279683718,166.109672896748));
#28437=CARTESIAN_POINT('Ctrl Pts',(-31.1647193509792,33.9951595187684,166.036314816837));
#28438=CARTESIAN_POINT('Ctrl Pts',(-30.6584039191552,33.5612522752606,166.));
#28439=CARTESIAN_POINT('Origin',(-32.,32.,180.545925280538));
#28440=CARTESIAN_POINT('',(-34.0520397258479,31.9988941582834,166.954074719462));
#28441=CARTESIAN_POINT('',(-34.0578396023064,32.0007586512867,166.895925280538));
#28442=CARTESIAN_POINT('',(-34.05475,32.0000000000002,180.545925280538));
#28443=CARTESIAN_POINT('Ctrl Pts',(-34.0578396023064,32.0007586512867,166.895925280538));
#28444=CARTESIAN_POINT('Ctrl Pts',(-34.0580398859891,32.0429254328027,166.893629624944));
#28445=CARTESIAN_POINT('Ctrl Pts',(-34.0377495998064,32.7653095502187,166.854290706278));
#28446=CARTESIAN_POINT('Ctrl Pts',(-33.1886966129007,34.1178213986476,166.777908524538));
#28447=CARTESIAN_POINT('Ctrl Pts',(-30.8656448664525,34.1473555806342,166.666778735318));
#28448=CARTESIAN_POINT('Ctrl Pts',(-29.580472395857,32.2117592705426,166.555648946099));
#28449=CARTESIAN_POINT('Ctrl Pts',(-30.5101755690543,30.0821472363061,166.444519156879));
#28450=CARTESIAN_POINT('Ctrl Pts',(-32.8022294248721,29.7081731264144,166.333389367659));
#28451=CARTESIAN_POINT('Ctrl Pts',(-33.9655640366591,30.9926240191872,166.250524742212));
#28452=CARTESIAN_POINT('Ctrl Pts',(-34.0562993333743,31.8362138935308,166.204703379838));
#28453=CARTESIAN_POINT('Ctrl Pts',(-34.0546693143771,31.9981396895887,166.195925280538));
#28454=CARTESIAN_POINT('Ctrl Pts',(-34.0520397258479,31.9988941582834,166.954074719462));
#28455=CARTESIAN_POINT('Ctrl Pts',(-34.0500128717713,32.413460949173,166.931667471325));
#28456=CARTESIAN_POINT('Ctrl Pts',(-33.7267813329344,33.5162878439086,166.872216960114));
#28457=CARTESIAN_POINT('Ctrl Pts',(-31.9269554489549,34.4275128925295,166.77572318583));
#28458=CARTESIAN_POINT('Ctrl Pts',(-29.9209653652486,33.2553461090702,166.66459339661));
#28459=CARTESIAN_POINT('Ctrl Pts',(-29.8177243014505,30.9342420640658,166.553463607391));
#28460=CARTESIAN_POINT('Ctrl Pts',(-31.7115987485412,29.5886264481624,166.442333818171));
#28461=CARTESIAN_POINT('Ctrl Pts',(-33.6494969660935,30.3618237184509,166.342537522195));
#28462=CARTESIAN_POINT('Ctrl Pts',(-34.0495335253161,31.5269023563923,166.279784489292));
#28463=CARTESIAN_POINT('Ctrl Pts',(-34.0533144349913,32.0018139164182,166.254074719462));
#28464=CARTESIAN_POINT('Origin',(-32.,32.,180.545925280538));
#28465=CARTESIAN_POINT('',(-34.0574025789111,31.998873138922,167.654074719462));
#28466=CARTESIAN_POINT('',(-34.0524751566312,32.0013942609758,167.595925280538));
#28467=CARTESIAN_POINT('',(-34.05475,32.0000000000002,180.545925280538));
#28468=CARTESIAN_POINT('Ctrl Pts',(-34.0524751566312,32.0013942609758,167.595925280538));
#28469=CARTESIAN_POINT('Ctrl Pts',(-34.0540188898388,32.2486160605419,167.582555870051));
#28470=CARTESIAN_POINT('Ctrl Pts',(-33.898241798428,33.1789471714754,167.53214319649));
#28471=CARTESIAN_POINT('Ctrl Pts',(-32.5140741057304,34.3735883477403,167.444687259856));
#28472=CARTESIAN_POINT('Ctrl Pts',(-30.2847464657706,33.7193294309385,167.333557470637));
#28473=CARTESIAN_POINT('Ctrl Pts',(-29.6251964648778,31.4915603532478,167.222427681417));
#28474=CARTESIAN_POINT('Ctrl Pts',(-31.1390486307216,29.7291066950132,167.111297892197));
#28475=CARTESIAN_POINT('Ctrl Pts',(-33.3932697819141,30.038431497626,167.002463758571));
#28476=CARTESIAN_POINT('Ctrl Pts',(-34.0548080592417,31.3625118789545,166.930672888018));
#28477=CARTESIAN_POINT('Ctrl Pts',(-34.0578396023064,32.0007586512867,166.895925280538));
#28478=CARTESIAN_POINT('Ctrl Pts',(-34.0574025789111,31.9988731389219,167.654074719462));
#28479=CARTESIAN_POINT('Ctrl Pts',(-34.0533392486364,32.6141954663041,167.620593716431));
#28480=CARTESIAN_POINT('Ctrl Pts',(-33.4332618733263,33.9174120761424,167.550069450326));
#28481=CARTESIAN_POINT('Ctrl Pts',(-31.2169834524517,34.2989297408903,167.442501921148));
#28482=CARTESIAN_POINT('Ctrl Pts',(-29.6439176314904,32.5891267679911,167.331372131929));
#28483=CARTESIAN_POINT('Ctrl Pts',(-30.2271133920415,30.3401605499161,167.220242342709));
#28484=CARTESIAN_POINT('Ctrl Pts',(-32.4328346333002,29.6102630575578,167.109112553489));
#28485=CARTESIAN_POINT('Ctrl Pts',(-33.8775609285965,30.7736143033716,167.020390012407));
#28486=CARTESIAN_POINT('Ctrl Pts',(-34.0533636307896,31.7281065226901,166.968710734398));
#28487=CARTESIAN_POINT('Ctrl Pts',(-34.0520397258479,31.9988941582834,166.954074719462));
#28488=CARTESIAN_POINT('Origin',(-32.,32.,180.545925280538));
#28489=CARTESIAN_POINT('',(-34.0554334607891,32.0018241253936,168.354074719462));
#28490=CARTESIAN_POINT('',(-34.052787823778,31.9984585248469,168.295925280538));
#28491=CARTESIAN_POINT('',(-34.05475,32.0000000000002,180.545925280538));
#28492=CARTESIAN_POINT('Ctrl Pts',(-34.052787823778,31.9984585248469,168.295925280538));
#28493=CARTESIAN_POINT('Ctrl Pts',(-34.0496367476198,32.450278669858,168.271482115157));
#28494=CARTESIAN_POINT('Ctrl Pts',(-33.6800738256301,33.5915111338001,168.209995686702));
#28495=CARTESIAN_POINT('Ctrl Pts',(-31.7940424397143,34.4198708436861,168.111465995175));
#28496=CARTESIAN_POINT('Ctrl Pts',(-29.8553132008219,33.1395226443526,168.000336205955));
#28497=CARTESIAN_POINT('Ctrl Pts',(-29.8793780091033,30.8162956994218,167.889206416735));
#28498=CARTESIAN_POINT('Ctrl Pts',(-31.8442131747296,29.5763820510783,167.778076627516));
#28499=CARTESIAN_POINT('Ctrl Pts',(-33.6980917649276,30.4368608971767,167.680316248783));
#28500=CARTESIAN_POINT('Ctrl Pts',(-34.0497415946373,31.5636268332647,167.619599133124));
#28501=CARTESIAN_POINT('Ctrl Pts',(-34.0524751566312,32.0013942609758,167.595925280538));
#28502=CARTESIAN_POINT('Ctrl Pts',(-34.0554334607891,32.0018241253936,168.354074719462));
#28503=CARTESIAN_POINT('Ctrl Pts',(-34.0567078357127,32.140216458308,168.34656322461));
#28504=CARTESIAN_POINT('Ctrl Pts',(-33.980880674796,32.9597080078657,168.302008466685));
#28505=CARTESIAN_POINT('Ctrl Pts',(-32.880554936408,34.2633639788494,168.220410445686));
#28506=CARTESIAN_POINT('Ctrl Pts',(-30.5761275089639,33.9674299515833,168.109280656467));
#28507=CARTESIAN_POINT('Ctrl Pts',(-29.5748127402796,31.870925374144,167.998150867247));
#28508=CARTESIAN_POINT('Ctrl Pts',(-30.7930030593313,29.8925484830768,167.887021078027));
#28509=CARTESIAN_POINT('Ctrl Pts',(-33.1158238734678,29.8428883892604,167.775891288808));
#28510=CARTESIAN_POINT('Ctrl Pts',(-34.025301548937,31.1875816460392,167.698242502619));
#28511=CARTESIAN_POINT('Ctrl Pts',(-34.057834902849,31.9334050244322,167.657636979504));
#28512=CARTESIAN_POINT('Ctrl Pts',(-34.0574025789111,31.9988731389219,167.654074719462));
#28513=CARTESIAN_POINT('Origin',(-32.,32.,180.545925280538));
#28514=CARTESIAN_POINT('',(-34.0514403583153,31.9999806718109,169.054074719462));
#28515=CARTESIAN_POINT('',(-34.0580205430257,31.9994845592736,168.995925280538));
#28516=CARTESIAN_POINT('',(-34.05475,32.0000000000002,180.545925280538));
#28517=CARTESIAN_POINT('Ctrl Pts',(-34.0580205430257,31.9994845592736,168.995925280538));
#28518=CARTESIAN_POINT('Ctrl Pts',(-34.055824427603,32.6517037300251,168.960408360263));
#28519=CARTESIAN_POINT('Ctrl Pts',(-33.3683227053502,33.9881561453664,168.887848176915));
#28520=CARTESIAN_POINT('Ctrl Pts',(-31.0921885701096,34.2525700451136,168.778244730493));
#28521=CARTESIAN_POINT('Ctrl Pts',(-29.6151760590397,32.4591385080545,168.667114941274));
#28522=CARTESIAN_POINT('Ctrl Pts',(-30.32072855565,30.2455083878672,168.555985152054));
#28523=CARTESIAN_POINT('Ctrl Pts',(-32.5631320687118,29.637569963837,168.444855362834));
#28524=CARTESIAN_POINT('Ctrl Pts',(-33.910300100793,30.8498682204949,168.358168738995));
#28525=CARTESIAN_POINT('Ctrl Pts',(-34.0544121578939,31.7655517847545,168.30852537823));
#28526=CARTESIAN_POINT('Ctrl Pts',(-34.052787823778,31.9984585248469,168.295925280538));
#28527=CARTESIAN_POINT('Ctrl Pts',(-34.0514403583153,31.9999806718109,169.054074719462));
#28528=CARTESIAN_POINT('Ctrl Pts',(-34.0514114848212,32.3440857144559,169.035489469716));
#28529=CARTESIAN_POINT('Ctrl Pts',(-33.8062204233054,33.3740837335787,168.979860956897));
#28530=CARTESIAN_POINT('Ctrl Pts',(-32.1767327307596,34.4221806365661,168.887189181005));
#28531=CARTESIAN_POINT('Ctrl Pts',(-30.0609459727286,33.4622800598482,168.776059391785));
#28532=CARTESIAN_POINT('Ctrl Pts',(-29.7197604322381,31.1641166302031,168.664929602565));
#28533=CARTESIAN_POINT('Ctrl Pts',(-31.4654254161029,29.6309445956577,168.553799813346));
#28534=CARTESIAN_POINT('Ctrl Pts',(-33.5492655722574,30.2229879815584,168.450181518978));
#28535=CARTESIAN_POINT('Ctrl Pts',(-34.050423200433,31.4577286584152,168.383606487684));
#28536=CARTESIAN_POINT('Ctrl Pts',(-34.0554334607891,32.0018241253936,168.354074719462));
#28537=CARTESIAN_POINT('Origin',(-32.,32.,180.545925280538));
#28538=CARTESIAN_POINT('',(-34.0555043948901,31.9981860244241,169.754074719462));
#28539=CARTESIAN_POINT('',(-34.0543001799161,32.0018685375719,169.695925280538));
#28540=CARTESIAN_POINT('',(-34.05475,32.0000000000002,180.545925280538));
#28541=CARTESIAN_POINT('Ctrl Pts',(-34.0543001799161,32.0018685375718,169.695925280538));
#28542=CARTESIAN_POINT('Ctrl Pts',(-34.0558755534125,32.1780191654457,169.686377868442));
#28543=CARTESIAN_POINT('Ctrl Pts',(-33.9545116436601,33.0358359111826,169.639787193273));
#28544=CARTESIAN_POINT('Ctrl Pts',(-32.7552096073727,34.3082139954844,169.556153255031));
#28545=CARTESIAN_POINT('Ctrl Pts',(-30.4704602652025,33.8864521196416,169.445023465811));
#28546=CARTESIAN_POINT('Ctrl Pts',(-29.5855291011564,31.7382297216221,169.333893676592));
#28547=CARTESIAN_POINT('Ctrl Pts',(-30.9102955198749,29.8295766435978,169.222763887372));
#28548=CARTESIAN_POINT('Ctrl Pts',(-33.2323476614723,29.9072714840831,169.111634098152));
#28549=CARTESIAN_POINT('Ctrl Pts',(-34.0448973027964,31.2632688876247,169.036021229208));
#28550=CARTESIAN_POINT('Ctrl Pts',(-34.0581149212807,31.9714553825744,168.997451623336));
#28551=CARTESIAN_POINT('Ctrl Pts',(-34.0580205430257,31.9994845592736,168.995925280538));
#28552=CARTESIAN_POINT('Ctrl Pts',(-34.0555043948901,31.9981860244241,169.754074719462));
#28553=CARTESIAN_POINT('Ctrl Pts',(-34.0504819393845,32.5445771872936,169.724415714822));
#28554=CARTESIAN_POINT('Ctrl Pts',(-33.5457293608021,33.7815914750713,169.65771344711));
#28555=CARTESIAN_POINT('Ctrl Pts',(-31.4573116781621,34.3672099356773,169.553967916323));
#28556=CARTESIAN_POINT('Ctrl Pts',(-29.7169099061327,32.8280658895954,169.442838127104));
#28557=CARTESIAN_POINT('Ctrl Pts',(-30.0659674289288,30.5310849213574,169.331708337884));
#28558=CARTESIAN_POINT('Ctrl Pts',(-32.1850305870609,29.5784391033703,169.220578548664));
#28559=CARTESIAN_POINT('Ctrl Pts',(-33.8086854086604,30.6306661455679,169.12803400919));
#28560=CARTESIAN_POINT('Ctrl Pts',(-34.0514690341387,31.658231405593,169.07253273279));
#28561=CARTESIAN_POINT('Ctrl Pts',(-34.0514403583153,31.9999806718109,169.054074719462));
#28562=CARTESIAN_POINT('Origin',(-32.,32.,180.545925280538));
#28563=CARTESIAN_POINT('',(-34.0573517780835,32.0011604961581,170.454074719462));
#28564=CARTESIAN_POINT('',(-34.0516184036866,31.9993739362734,170.395925280538));
#28565=CARTESIAN_POINT('',(-34.05475,32.0000000000002,180.545925280538));
#28566=CARTESIAN_POINT('Ctrl Pts',(-34.0516184036866,31.9993739362734,170.395925280538));
#28567=CARTESIAN_POINT('Ctrl Pts',(-34.0505756284383,32.3810911960151,170.375304113548));
#28568=CARTESIAN_POINT('Ctrl Pts',(-33.765219332864,33.4499626319616,170.317639683486));
#28569=CARTESIAN_POINT('Ctrl Pts',(-32.0437423814044,34.4282256905171,170.22293199035));
#28570=CARTESIAN_POINT('Ctrl Pts',(-29.9837327342869,33.3538314936623,170.11180220113));
#28571=CARTESIAN_POINT('Ctrl Pts',(-29.768989023242,31.0404253954989,170.00067241191));
#28572=CARTESIAN_POINT('Ctrl Pts',(-31.5960423638194,29.6052115692218,169.88954262269));
#28573=CARTESIAN_POINT('Ctrl Pts',(-33.6040654953814,30.2966920425492,169.787960245566));
#28574=CARTESIAN_POINT('Ctrl Pts',(-34.0497632190666,31.494567567931,169.723421131515));
#28575=CARTESIAN_POINT('Ctrl Pts',(-34.0543001799161,32.0018685375718,169.695925280538));
#28576=CARTESIAN_POINT('Ctrl Pts',(-34.0573517780835,32.0011604961581,170.454074719462));
#28577=CARTESIAN_POINT('Ctrl Pts',(-34.0578102020088,32.0689714028747,170.450385223002));
#28578=CARTESIAN_POINT('Ctrl Pts',(-34.0240039615804,32.8171543593945,170.409652463468));
#28579=CARTESIAN_POINT('Ctrl Pts',(-33.1084266208509,34.1609220070185,170.331876440861));
#28580=CARTESIAN_POINT('Ctrl Pts',(-30.7857895731111,34.1033037187868,170.220746651641));
#28581=CARTESIAN_POINT('Ctrl Pts',(-29.5743847404962,32.1207646765004,170.109616862422));
#28582=CARTESIAN_POINT('Ctrl Pts',(-30.582876688677,30.0277031119193,169.998487073202));
#28583=CARTESIAN_POINT('Ctrl Pts',(-32.8883045233183,29.7396662706405,169.887357283983));
#28584=CARTESIAN_POINT('Ctrl Pts',(-33.9824484353958,31.0450458660859,169.805886499402));
#28585=CARTESIAN_POINT('Ctrl Pts',(-34.0567548451285,31.8621499840586,169.761458977896));
#28586=CARTESIAN_POINT('Ctrl Pts',(-34.0555043948901,31.9981860244241,169.754074719462));
#28587=CARTESIAN_POINT('Origin',(-32.,32.,180.545925280538));
#28588=CARTESIAN_POINT('',(-34.0520023281243,32.0010746918646,171.154074719462));
#28589=CARTESIAN_POINT('',(-34.0565936314237,31.9984640339053,171.095925280538));
#28590=CARTESIAN_POINT('',(-34.05475,32.0000000000002,180.545925280538));
#28591=CARTESIAN_POINT('Ctrl Pts',(-34.0565936314237,31.9984640339053,171.095925280538));
#28592=CARTESIAN_POINT('Ctrl Pts',(-34.0517293483252,32.5815615602143,171.064230358654));
#28593=CARTESIAN_POINT('Ctrl Pts',(-33.4873352336299,33.854384656826,170.995492173698));
#28594=CARTESIAN_POINT('Ctrl Pts',(-31.3284143499829,34.3339164755211,170.889710725668));
#28595=CARTESIAN_POINT('Ctrl Pts',(-29.6749656940012,32.7017185161778,170.778580936448));
#28596=CARTESIAN_POINT('Ctrl Pts',(-30.1493632209224,30.4273153806489,170.667451147228));
#28597=CARTESIAN_POINT('Ctrl Pts',(-32.3174434587353,29.5922161536956,170.556321358009));
#28598=CARTESIAN_POINT('Ctrl Pts',(-33.8466042542176,30.7067606771023,170.465812735778));
#28599=CARTESIAN_POINT('Ctrl Pts',(-34.0524488394874,31.695385441368,170.412347376621));
#28600=CARTESIAN_POINT('Ctrl Pts',(-34.0516184036866,31.9993739362734,170.395925280538));
#28601=CARTESIAN_POINT('Ctrl Pts',(-34.0520023281243,32.0010746918646,171.154074719462));
#28602=CARTESIAN_POINT('Ctrl Pts',(-34.0532978514709,32.2742285901281,171.139311468108));
#28603=CARTESIAN_POINT('Ctrl Pts',(-33.8754247390233,33.2311488262767,171.087504953681));
#28604=CARTESIAN_POINT('Ctrl Pts',(-32.4246449842735,34.3912068357963,170.99865517618));
#28605=CARTESIAN_POINT('Ctrl Pts',(-30.2214365358583,33.6537549692286,170.88752538696));
#28606=CARTESIAN_POINT('Ctrl Pts',(-29.645950082108,31.4028044890487,170.77639559774));
#28607=CARTESIAN_POINT('Ctrl Pts',(-31.224864584604,29.6984008641758,170.665265808521));
#28608=CARTESIAN_POINT('Ctrl Pts',(-33.4372029785745,30.0870496218184,170.557825515761));
#28609=CARTESIAN_POINT('Ctrl Pts',(-34.0532075365108,31.3881366917763,170.487428486075));
#28610=CARTESIAN_POINT('Ctrl Pts',(-34.0573517780835,32.0011604961581,170.454074719462));
#28611=CARTESIAN_POINT('Origin',(-32.,32.,180.545925280538));
#28612=CARTESIAN_POINT('',(-34.0534331717271,31.9982546175746,171.854074719462));
#28613=CARTESIAN_POINT('',(-34.0564014405732,32.0016034613785,171.795925280538));
#28614=CARTESIAN_POINT('',(-34.05475,32.0000000000002,180.545925280538));
#28615=CARTESIAN_POINT('Ctrl Pts',(-34.0564014405732,32.0016034613785,171.795925280538));
#28616=CARTESIAN_POINT('Ctrl Pts',(-34.0573060965439,32.1069606022137,171.790199866834));
#28617=CARTESIAN_POINT('Ctrl Pts',(-34.0020448223411,32.8930239103454,171.747431190057));
#28618=CARTESIAN_POINT('Ctrl Pts',(-32.9883523019571,34.2184122987475,171.667619250206));
#28619=CARTESIAN_POINT('Ctrl Pts',(-30.6723620474344,34.0336103036043,171.556489460986));
#28620=CARTESIAN_POINT('Ctrl Pts',(-29.5714116494658,31.9876702121879,171.445359671767));
#28621=CARTESIAN_POINT('Ctrl Pts',(-30.693078972962,29.9530142088661,171.334229882547));
#28622=CARTESIAN_POINT('Ctrl Pts',(-33.0108262474351,29.7917374029535,171.223100093327));
#28623=CARTESIAN_POINT('Ctrl Pts',(-34.0062836592036,31.121039988534,171.143665225991));
#28624=CARTESIAN_POINT('Ctrl Pts',(-34.0574144520508,31.9000695803972,171.101273621728));
#28625=CARTESIAN_POINT('Ctrl Pts',(-34.0565936314237,31.9984640339053,171.095925280538));
#28626=CARTESIAN_POINT('Ctrl Pts',(-34.0534331717271,31.9982546175746,171.854074719462));
#28627=CARTESIAN_POINT('Ctrl Pts',(-34.0495792571287,32.4754606590366,171.828237713214));
#28628=CARTESIAN_POINT('Ctrl Pts',(-33.6462714964515,33.64272521891,171.765357443893));
#28629=CARTESIAN_POINT('Ctrl Pts',(-31.7033831827247,34.4104381257226,171.665433911498));
#28630=CARTESIAN_POINT('Ctrl Pts',(-29.81406369269,33.0582419168657,171.554304122278));
#28631=CARTESIAN_POINT('Ctrl Pts',(-29.9252894056131,30.7375541818489,171.443174333058));
#28632=CARTESIAN_POINT('Ctrl Pts',(-31.9352677552198,29.5722431689493,171.332044543839));
#28633=CARTESIAN_POINT('Ctrl Pts',(-33.729598748851,30.4884300255591,171.235678005973));
#28634=CARTESIAN_POINT('Ctrl Pts',(-34.0500471845957,31.5888435438389,171.176354731181));
#28635=CARTESIAN_POINT('Ctrl Pts',(-34.0520023281243,32.0010746918646,171.154074719462));
#28636=CARTESIAN_POINT('Origin',(-32.,32.,180.545925280538));
#28637=CARTESIAN_POINT('',(-34.0581778177724,31.9999545502976,172.554074719462));
#28638=CARTESIAN_POINT('',(-34.0515604146746,32.0005167850725,172.495925280538));
#28639=CARTESIAN_POINT('',(-34.05475,32.0000000000002,180.545925280538));
#28640=CARTESIAN_POINT('Ctrl Pts',(-34.0515604146746,32.0005167850725,172.495925280538));
#28641=CARTESIAN_POINT('Ctrl Pts',(-34.0522605175172,32.311507193629,172.47912611194));
#28642=CARTESIAN_POINT('Ctrl Pts',(-33.839795546903,33.307343922864,172.425283680269));
#28643=CARTESIAN_POINT('Ctrl Pts',(-32.2929793955673,34.4108829241154,172.334397985524));
#28644=CARTESIAN_POINT('Ctrl Pts',(-30.1334901928539,33.5538129037453,172.223268196305));
#28645=CARTESIAN_POINT('Ctrl Pts',(-29.6822105241847,31.2747101642669,172.112138407085));
#28646=CARTESIAN_POINT('Ctrl Pts',(-31.3521466484014,29.6593848170106,172.001008617865));
#28647=CARTESIAN_POINT('Ctrl Pts',(-33.49840924462,30.1590253490049,171.895604242349));
#28648=CARTESIAN_POINT('Ctrl Pts',(-34.0514529982616,31.4253029113651,171.827243129907));
#28649=CARTESIAN_POINT('Ctrl Pts',(-34.0564014405732,32.0016034613785,171.795925280538));
#28650=CARTESIAN_POINT('Ctrl Pts',(-34.0581773322723,31.9999545567349,172.554074719462));
#28651=CARTESIAN_POINT('Ctrl Pts',(-34.0579568195032,32.6776310956056,172.51716395832));
#28652=CARTESIAN_POINT('Ctrl Pts',(-33.32180623737,34.0358274377969,172.443209934105));
#28653=CARTESIAN_POINT('Ctrl Pts',(-31.0083014790376,34.2169184779213,172.332212646816));
#28654=CARTESIAN_POINT('Ctrl Pts',(-29.5996267287836,32.3693259441983,172.221082857597));
#28655=CARTESIAN_POINT('Ctrl Pts',(-30.3877475653827,30.183730311518,172.109953068377));
#28656=CARTESIAN_POINT('Ctrl Pts',(-32.6513843459939,29.660365001112,171.998823279157));
#28657=CARTESIAN_POINT('Ctrl Pts',(-33.9311982594295,30.902069459774,171.913530496186));
#28658=CARTESIAN_POINT('Ctrl Pts',(-34.0551047259449,31.7912765564278,171.865280976287));
#28659=CARTESIAN_POINT('Ctrl Pts',(-34.0534331717271,31.9982546175746,171.854074719462));
#28660=CARTESIAN_POINT('Origin',(-32.,32.,180.545925280538));
#28661=CARTESIAN_POINT('',(-34.0535655946932,32.0017741612571,173.254074719462));
#28662=CARTESIAN_POINT('',(-34.054507140811,31.998123038607,173.195925280538));
#28663=CARTESIAN_POINT('',(-34.05475,32.0000000000002,180.545925280538));
#28664=CARTESIAN_POINT('Ctrl Pts',(-34.054507140811,31.998123038607,173.195925280538));
#28665=CARTESIAN_POINT('Ctrl Pts',(-34.0498473910169,32.5122490193519,173.168052357046));
#28666=CARTESIAN_POINT('Ctrl Pts',(-33.5941675160557,33.7170162573815,173.103136170481));
#28667=CARTESIAN_POINT('Ctrl Pts',(-31.5717474387099,34.3905633528034,173.001176720843));
#28668=CARTESIAN_POINT('Ctrl Pts',(-29.7593608834192,32.93687232282,172.890046931623));
#28669=CARTESIAN_POINT('Ctrl Pts',(-29.9975829489038,30.625765902949,172.778917142403));
#28670=CARTESIAN_POINT('Ctrl Pts',(-32.068395384243,29.5723436257509,172.667787353184));
#28671=CARTESIAN_POINT('Ctrl Pts',(-33.7730366450004,30.5640711797273,172.573456732562));
#28672=CARTESIAN_POINT('Ctrl Pts',(-34.0507167450606,31.6257530475051,172.516169375013));
#28673=CARTESIAN_POINT('Ctrl Pts',(-34.0515604146746,32.0005167850725,172.495925280538));
#28674=CARTESIAN_POINT('Ctrl Pts',(-34.0535655946932,32.0017741612571,173.254074719462));
#28675=CARTESIAN_POINT('Ctrl Pts',(-34.0552323561726,32.2038246657458,173.2431334665));
#28676=CARTESIAN_POINT('Ctrl Pts',(-33.9350351245523,33.0880078984862,173.195148950464));
#28677=CARTESIAN_POINT('Ctrl Pts',(-32.6680632717471,34.3349271849826,173.110121171355));
#28678=CARTESIAN_POINT('Ctrl Pts',(-30.4007494190391,33.8277283916173,172.998991382135));
#28679=CARTESIAN_POINT('Ctrl Pts',(-29.5970523548762,31.6478123951331,172.887861592915));
#28680=CARTESIAN_POINT('Ctrl Pts',(-30.9925069166485,29.7902146753074,172.776731803695));
#28681=CARTESIAN_POINT('Ctrl Pts',(-33.3100082224966,29.9549885205165,172.665602014476));
#28682=CARTESIAN_POINT('Ctrl Pts',(-34.0570726014949,31.3149806065769,172.591382986398));
#28683=CARTESIAN_POINT('Ctrl Pts',(-34.0581781238671,31.9975218393558,172.554207221394));
#28684=CARTESIAN_POINT('Ctrl Pts',(-34.0581773322723,31.9999545567349,172.554074719462));
#28685=CARTESIAN_POINT('Origin',(-32.,32.,180.545925280538));
#28686=CARTESIAN_POINT('',(-34.0519273834553,31.9989926864668,173.954074719462));
#28687=CARTESIAN_POINT('',(-34.0579373256583,32.0006373959877,173.895925280538));
#28688=CARTESIAN_POINT('',(-34.05475,32.0000000000002,180.545925280538));
#28689=CARTESIAN_POINT('Ctrl Pts',(-34.0579373256583,32.0006373959877,173.895925280538));
#28690=CARTESIAN_POINT('Ctrl Pts',(-34.0580796886322,32.0355947629004,173.894021865225));
#28691=CARTESIAN_POINT('Ctrl Pts',(-34.041431950888,32.7507355168895,173.85507518684));
#28692=CARTESIAN_POINT('Ctrl Pts',(-33.2110353847761,34.1051334154486,173.779085245381));
#28693=CARTESIAN_POINT('Ctrl Pts',(-30.8883140600557,34.1592470379621,173.667955456161));
#28694=CARTESIAN_POINT('Ctrl Pts',(-29.5829956518403,32.2372411873918,173.556825666941));
#28695=CARTESIAN_POINT('Ctrl Pts',(-30.48969341174,30.098114774894,173.445695877722));
#28696=CARTESIAN_POINT('Ctrl Pts',(-32.7786073826223,29.6995730953269,173.334566088502));
#28697=CARTESIAN_POINT('Ctrl Pts',(-33.9595797099711,30.9782715764583,173.251309222774));
#28698=CARTESIAN_POINT('Ctrl Pts',(-34.0560402231944,31.8289728655904,173.205095620119));
#28699=CARTESIAN_POINT('Ctrl Pts',(-34.054507140811,31.998123038607,173.195925280538));
#28700=CARTESIAN_POINT('Ctrl Pts',(-34.0519273834553,31.9989926864668,173.954074719462));
#28701=CARTESIAN_POINT('Ctrl Pts',(-34.0501205240319,32.4063578939422,173.932059711606));
#28702=CARTESIAN_POINT('Ctrl Pts',(-33.7354249649502,33.501743785199,173.873001440676));
#28703=CARTESIAN_POINT('Ctrl Pts',(-31.9525937468572,34.4281569433195,173.776899906673));
#28704=CARTESIAN_POINT('Ctrl Pts',(-29.9343509763561,33.2772186991064,173.665770117453));
#28705=CARTESIAN_POINT('Ctrl Pts',(-29.8065677912631,30.9573837523311,173.554640328233));
#28706=CARTESIAN_POINT('Ctrl Pts',(-31.6861899768242,29.59173988872,173.443510539014));
#28707=CARTESIAN_POINT('Ctrl Pts',(-33.6396742476966,30.3475681058338,173.343322002757));
#28708=CARTESIAN_POINT('Ctrl Pts',(-34.0495892836497,31.5197521909239,173.280176729573));
#28709=CARTESIAN_POINT('Ctrl Pts',(-34.0535655946932,32.0017741612571,173.254074719462));
#28710=CARTESIAN_POINT('Origin',(-32.,32.,180.545925280538));
#28711=CARTESIAN_POINT('',(-34.0572421730302,31.9987715047938,174.654074719462));
#28712=CARTESIAN_POINT('',(-34.0526302784379,32.0014721866858,174.595925280538));
#28713=CARTESIAN_POINT('',(-34.05475,32.0000000000002,180.545925280538));
#28714=CARTESIAN_POINT('Ctrl Pts',(-34.052630278438,32.0014721866858,174.595925280538));
#28715=CARTESIAN_POINT('Ctrl Pts',(-34.0542200654754,32.2413952503059,174.582948110331));
#28716=CARTESIAN_POINT('Ctrl Pts',(-33.9044368370703,33.1642554087556,174.532927677052));
#28717=CARTESIAN_POINT('Ctrl Pts',(-32.53911584455,34.368026078018,174.445863980699));
#28718=CARTESIAN_POINT('Ctrl Pts',(-30.3030006968699,33.737350501538,174.33473419148));
#28719=CARTESIAN_POINT('Ctrl Pts',(-29.6199609082234,31.516670586832,174.22360440226));
#28720=CARTESIAN_POINT('Ctrl Pts',(-31.1151070859216,29.7383285095682,174.11247461304));
#28721=CARTESIAN_POINT('Ctrl Pts',(-33.3806181097287,30.0248506233853,174.003248239133));
#28722=CARTESIAN_POINT('Ctrl Pts',(-34.0553090956569,31.3552729589962,173.931065128299));
#28723=CARTESIAN_POINT('Ctrl Pts',(-34.0579373256583,32.0006373959877,173.895925280538));
#28724=CARTESIAN_POINT('Ctrl Pts',(-34.0572421730302,31.9987715047937,174.654074719462));
#28725=CARTESIAN_POINT('Ctrl Pts',(-34.0529417874593,32.6070099230316,174.620985956712));
#28726=CARTESIAN_POINT('Ctrl Pts',(-33.445367295585,33.9036433939219,174.550853930888));
#28727=CARTESIAN_POINT('Ctrl Pts',(-31.2413084093575,34.3070718594175,174.443678641991));
#28728=CARTESIAN_POINT('Ctrl Pts',(-29.650271574393,32.6139786805113,174.332548852772));
#28729=CARTESIAN_POINT('Ctrl Pts',(-30.2096807128004,30.3589788715227,174.221419063552));
#28730=CARTESIAN_POINT('Ctrl Pts',(-32.4075706476486,29.6058238031834,174.110289274332));
#28731=CARTESIAN_POINT('Ctrl Pts',(-33.8709432602969,30.7589286188374,174.021174492969));
#28732=CARTESIAN_POINT('Ctrl Pts',(-34.0531608122478,31.720910191825,173.969102974679));
#28733=CARTESIAN_POINT('Ctrl Pts',(-34.0519273834553,31.9989926864668,173.954074719462));
#28734=CARTESIAN_POINT('Origin',(-32.,32.,180.545925280538));
#28735=CARTESIAN_POINT('',(-34.0556515462546,32.0017900557631,175.354074719462));
#28736=CARTESIAN_POINT('',(-34.0526241093217,31.9985307172981,175.295925280538));
#28737=CARTESIAN_POINT('',(-34.05475,32.0000000000002,180.545925280538));
#28738=CARTESIAN_POINT('Ctrl Pts',(-34.0526241093217,31.9985307172981,175.295925280538));
#28739=CARTESIAN_POINT('Ctrl Pts',(-34.0496840965633,32.4431896949484,175.271874355438));
#28740=CARTESIAN_POINT('Ctrl Pts',(-33.6893167705434,33.5770541420994,175.210780167264));
#28741=CARTESIAN_POINT('Ctrl Pts',(-31.8196126720174,34.4219111899327,175.112642716018));
#28742=CARTESIAN_POINT('Ctrl Pts',(-29.867468483099,33.1621113240314,175.001512926798));
#28743=CARTESIAN_POINT('Ctrl Pts',(-29.8669940121071,30.8387597769491,174.890383137578));
#28744=CARTESIAN_POINT('Ctrl Pts',(-31.8186234897481,29.5781626888771,174.779253348358));
#28745=CARTESIAN_POINT('Ctrl Pts',(-33.6889615308727,30.4223864705328,174.681100729345));
#28746=CARTESIAN_POINT('Ctrl Pts',(-34.0496820268643,31.5565361460665,174.619991373405));
#28747=CARTESIAN_POINT('Ctrl Pts',(-34.052630278438,32.0014721866858,174.595925280538));
#28748=CARTESIAN_POINT('Ctrl Pts',(-34.0556515462546,32.0017900557631,175.354074719462));
#28749=CARTESIAN_POINT('Ctrl Pts',(-34.0568506849504,32.1329198985566,175.346955464891));
#28750=CARTESIAN_POINT('Ctrl Pts',(-33.9856838785989,32.94505453146,175.302792947247));
#28751=CARTESIAN_POINT('Ctrl Pts',(-32.9044115271646,34.2539372847887,175.221587166529));
#28752=CARTESIAN_POINT('Ctrl Pts',(-30.5969869759018,33.9823591875437,175.11045737731));
#28753=CARTESIAN_POINT('Ctrl Pts',(-29.5735847292512,31.8965474596491,174.99932758809));
#28754=CARTESIAN_POINT('Ctrl Pts',(-30.7708114250119,29.9054143747875,174.88819779887));
#28755=CARTESIAN_POINT('Ctrl Pts',(-33.0929781746067,29.8312233392852,174.77706800965));
#28756=CARTESIAN_POINT('Ctrl Pts',(-34.0212734697525,31.172979462216,174.699026983181));
#28757=CARTESIAN_POINT('Ctrl Pts',(-34.0577561202048,31.9260797864791,174.658029219785));
#28758=CARTESIAN_POINT('Ctrl Pts',(-34.0572421730302,31.9987715047937,174.654074719462));
#28759=CARTESIAN_POINT('Origin',(-32.,32.,180.545925280538));
#28760=CARTESIAN_POINT('',(-34.0514445903522,32.000099796643,176.054074719462));
#28761=CARTESIAN_POINT('',(-34.0579336495468,31.9993577651623,175.995925280538));
#28762=CARTESIAN_POINT('',(-34.05475,32.0000000000002,180.545925280538));
#28763=CARTESIAN_POINT('Ctrl Pts',(-34.0579336495468,31.9993577651623,175.995925280538));
#28764=CARTESIAN_POINT('Ctrl Pts',(-34.0552889021134,32.6444467097459,175.960800600544));
#28765=CARTESIAN_POINT('Ctrl Pts',(-33.3811101331092,33.9746252333219,175.888632657476));
#28766=CARTESIAN_POINT('Ctrl Pts',(-31.1160309092789,34.2620327244924,175.779421451336));
#28767=CARTESIAN_POINT('Ctrl Pts',(-29.6201585161938,32.4843014680682,175.668291662116));
#28768=CARTESIAN_POINT('Ctrl Pts',(-30.3022912407822,30.2633427601015,175.557161872896));
#28769=CARTESIAN_POINT('Ctrl Pts',(-32.5381486109218,29.631753924825,175.446032083677));
#28770=CARTESIAN_POINT('Ctrl Pts',(-33.9041990981139,30.8351764637911,175.358953219557));
#28771=CARTESIAN_POINT('Ctrl Pts',(-34.0542123076651,31.7583254155745,175.308917618511));
#28772=CARTESIAN_POINT('Ctrl Pts',(-34.0526241093217,31.9985307172981,175.295925280538));
#28773=CARTESIAN_POINT('Ctrl Pts',(-34.0514445903522,32.000099796643,176.054074719462));
#28774=CARTESIAN_POINT('Ctrl Pts',(-34.051590542369,32.3369407953034,176.035881709997));
#28775=CARTESIAN_POINT('Ctrl Pts',(-33.8137830896685,33.3594384891899,175.980645437459));
#28776=CARTESIAN_POINT('Ctrl Pts',(-32.2023060055888,34.4201788723936,175.888365901848));
#28777=CARTESIAN_POINT('Ctrl Pts',(-30.0764987714868,33.4826788317565,175.777236112628));
#28778=CARTESIAN_POINT('Ctrl Pts',(-29.7110590022335,31.1882472032951,175.666106323408));
#28779=CARTESIAN_POINT('Ctrl Pts',(-31.4404332115969,29.6367229312773,175.554976534189));
#28780=CARTESIAN_POINT('Ctrl Pts',(-33.5383217807162,30.2088814213863,175.45096599954));
#28781=CARTESIAN_POINT('Ctrl Pts',(-34.0506112662406,31.4506185122487,175.383998727964));
#28782=CARTESIAN_POINT('Ctrl Pts',(-34.0556515462546,32.0017900557631,175.354074719462));
#28783=CARTESIAN_POINT('Origin',(-32.,32.,180.545925280538));
#28784=CARTESIAN_POINT('',(-34.0552853099115,31.9981575238583,176.754074719462));
#28785=CARTESIAN_POINT('',(-34.0545155163552,32.0018771437926,176.695925280538));
#28786=CARTESIAN_POINT('',(-34.05475,32.0000000000002,180.545925280538));
#28787=CARTESIAN_POINT('Ctrl Pts',(-34.0545155163552,32.0018771437926,176.695925280538));
#28788=CARTESIAN_POINT('Ctrl Pts',(-34.0560467546979,32.1707457859868,176.686770108723));
#28789=CARTESIAN_POINT('Ctrl Pts',(-33.9597818030922,33.0211610160312,176.640571673835));
#28790=CARTESIAN_POINT('Ctrl Pts',(-32.7795468963266,34.3001087007756,176.557329975874));
#28791=CARTESIAN_POINT('Ctrl Pts',(-30.4904703373783,33.9025019311548,176.446200186654));
#28792=CARTESIAN_POINT('Ctrl Pts',(-29.5828989554375,31.7637460255249,176.335070397434));
#28793=CARTESIAN_POINT('Ctrl Pts',(-30.8874322371387,29.8412071954588,176.223940608215));
#28794=CARTESIAN_POINT('Ctrl Pts',(-33.210175470102,29.8943721288814,176.112810818995));
#28795=CARTESIAN_POINT('Ctrl Pts',(-34.0412910121703,31.2487010232944,176.036805709769));
#28796=CARTESIAN_POINT('Ctrl Pts',(-34.0580781111525,31.9641216652496,175.997843863617));
#28797=CARTESIAN_POINT('Ctrl Pts',(-34.0579336495468,31.9993577651623,175.995925280538));
#28798=CARTESIAN_POINT('Ctrl Pts',(-34.0552853099115,31.9981575238583,176.754074719462));
#28799=CARTESIAN_POINT('Ctrl Pts',(-34.0503077464059,32.5374704460802,176.724807955103));
#28800=CARTESIAN_POINT('Ctrl Pts',(-33.5565883061217,33.7674634392079,176.658497927671));
#28801=CARTESIAN_POINT('Ctrl Pts',(-31.4823444807967,34.3728097817195,176.555144637166));
#28802=CARTESIAN_POINT('Ctrl Pts',(-29.7257833087973,32.8521337550634,176.444014847946));
#28803=CARTESIAN_POINT('Ctrl Pts',(-30.0505605908462,30.5515941579779,176.332885058727));
#28804=CARTESIAN_POINT('Ctrl Pts',(-32.1594436788161,29.5766198796149,176.221755269507));
#28805=CARTESIAN_POINT('Ctrl Pts',(-33.8010499920725,30.6160259659334,176.128818489752));
#28806=CARTESIAN_POINT('Ctrl Pts',(-34.051293365645,31.651090015572,176.072924973071));
#28807=CARTESIAN_POINT('Ctrl Pts',(-34.0514445903522,32.000099796643,176.054074719462));
#28808=CARTESIAN_POINT('Origin',(-32.,32.,180.545925280538));
#28809=CARTESIAN_POINT('',(-34.0575043898772,32.0010548445575,177.454074719462));
#28810=CARTESIAN_POINT('',(-34.0515583141596,31.999487637131,177.395925280538));
#28811=CARTESIAN_POINT('',(-34.05475,32.0000000000002,180.545925280538));
#28812=CARTESIAN_POINT('Ctrl Pts',(-34.0515583141596,31.999487637131,177.395925280538));
#28813=CARTESIAN_POINT('Ctrl Pts',(-34.0507225647854,32.3739715482354,177.375696353829));
#28814=CARTESIAN_POINT('Ctrl Pts',(-33.7733489562679,33.4353641275151,177.318424164048));
#28815=CARTESIAN_POINT('Ctrl Pts',(-32.0693869201392,34.4276282208927,177.224108711192));
#28816=CARTESIAN_POINT('Ctrl Pts',(-29.9981444046188,33.3750518506594,177.112978921973));
#28817=CARTESIAN_POINT('Ctrl Pts',(-29.758978416765,31.0640429106968,177.001849132753));
#28818=CARTESIAN_POINT('Ctrl Pts',(-31.5707710809886,29.6096117624978,176.890719343533));
#28819=CARTESIAN_POINT('Ctrl Pts',(-33.5937669922501,30.2824328445151,176.788744726128));
#28820=CARTESIAN_POINT('Ctrl Pts',(-34.0498511238672,31.487476737163,176.723813371796));
#28821=CARTESIAN_POINT('Ctrl Pts',(-34.0545155163552,32.0018771437926,176.695925280538));
#28822=CARTESIAN_POINT('Ctrl Pts',(-34.0575043898772,32.0010548445575,177.454074719462));
#28823=CARTESIAN_POINT('Ctrl Pts',(-34.0578837084661,32.06164475004,177.450777463283));
#28824=CARTESIAN_POINT('Ctrl Pts',(-34.0279763621718,32.8025565918032,177.41043694403));
#28825=CARTESIAN_POINT('Ctrl Pts',(-33.1311884148471,34.1490941434474,177.333053161704));
#28826=CARTESIAN_POINT('Ctrl Pts',(-30.8080724930038,34.1160109663009,177.221923372484));
#28827=CARTESIAN_POINT('Ctrl Pts',(-29.5757955383114,32.1463773261312,177.110793583265));
#28828=CARTESIAN_POINT('Ctrl Pts',(-30.5621242967963,30.0427808298698,176.999663794045));
#28829=CARTESIAN_POINT('Ctrl Pts',(-32.8643812668194,29.7304100510143,176.888534004825));
#28830=CARTESIAN_POINT('Ctrl Pts',(-33.9775854365096,31.0303892118588,176.806670979964));
#28831=CARTESIAN_POINT('Ctrl Pts',(-34.0566079028612,31.8548561942385,176.761851218177));
#28832=CARTESIAN_POINT('Ctrl Pts',(-34.0552853099115,31.9981575238583,176.754074719462));
#28833=CARTESIAN_POINT('Origin',(-32.,32.,180.545925280538));
#28834=CARTESIAN_POINT('',(-34.0521188506995,32.0011671092335,178.154074719462));
#28835=CARTESIAN_POINT('',(-34.0563933814841,31.9983925126321,178.095925280538));
#28836=CARTESIAN_POINT('',(-34.05475,32.0000000000002,180.545925280538));
#28837=CARTESIAN_POINT('Ctrl Pts',(-34.0563933814841,31.9983925126321,178.095925280538));
#28838=CARTESIAN_POINT('Ctrl Pts',(-34.0514420886706,32.5744194654198,178.064622598935));
#28839=CARTESIAN_POINT('Ctrl Pts',(-33.4988525240404,33.840436615865,177.99627665426));
#28840=CARTESIAN_POINT('Ctrl Pts',(-31.3531025346477,34.3408784778579,177.890887446511));
#28841=CARTESIAN_POINT('Ctrl Pts',(-29.6825070314679,32.7262369940422,177.779757657291));
#28842=CARTESIAN_POINT('Ctrl Pts',(-30.1328556755869,30.4469493074261,177.668627868071));
#28843=CARTESIAN_POINT('Ctrl Pts',(-32.2919946972204,29.588997745803,177.557498078852));
#28844=CARTESIAN_POINT('Ctrl Pts',(-33.8395196429225,30.6920887795438,177.46659721634));
#28845=CARTESIAN_POINT('Ctrl Pts',(-34.0522529912079,31.6882156386111,177.412739616902));
#28846=CARTESIAN_POINT('Ctrl Pts',(-34.0515583141596,31.999487637131,177.395925280538));
#28847=CARTESIAN_POINT('Ctrl Pts',(-34.0521188506995,32.0011671092335,178.154074719462));
#28848=CARTESIAN_POINT('Ctrl Pts',(-34.0535001213909,32.2670274833358,178.139703708389));
#28849=CARTESIAN_POINT('Ctrl Pts',(-33.8819824988062,33.2164703631673,178.088289434242));
#28850=CARTESIAN_POINT('Ctrl Pts',(-32.4498708069788,34.3865813639729,177.999831897023));
#28851=CARTESIAN_POINT('Ctrl Pts',(-30.239005926868,33.6724513835904,177.888702107803));
#28852=CARTESIAN_POINT('Ctrl Pts',(-29.6397722337213,31.4276996511778,177.777572318583));
#28853=CARTESIAN_POINT('Ctrl Pts',(-31.2005990409054,29.7067170736135,177.666442529363));
#28854=CARTESIAN_POINT('Ctrl Pts',(-33.4250091228452,30.0733096650126,177.558609996323));
#28855=CARTESIAN_POINT('Ctrl Pts',(-34.0536222263393,31.3809430738059,177.487820726356));
#28856=CARTESIAN_POINT('Ctrl Pts',(-34.0575043898772,32.0010548445575,177.454074719462));
#28857=CARTESIAN_POINT('Origin',(-32.,32.,180.545925280538));
#28858=CARTESIAN_POINT('',(-34.0526600320705,31.9978184065947,178.854074719462));
#28859=CARTESIAN_POINT('',(-34.0565967526292,32.0015021117824,178.795925280538));
#28860=CARTESIAN_POINT('',(-34.05475,32.0000000000002,180.545925280538));
#28861=CARTESIAN_POINT('',(-32.5301702171895,30.0148256743285,179.));
#28862=CARTESIAN_POINT('Ctrl Pts',(-32.5301702171895,30.0148256743285,179.));
#28863=CARTESIAN_POINT('Ctrl Pts',(-33.1902397907536,30.1911070339307,178.962956736927));
#28864=CARTESIAN_POINT('Ctrl Pts',(-33.9248822846665,30.8874020551484,178.914314976748));
#28865=CARTESIAN_POINT('Ctrl Pts',(-34.0542719955,31.7835489011663,178.865673216568));
#28866=CARTESIAN_POINT('Ctrl Pts',(-34.0526600320705,31.9978184065947,178.854074719462));
#28867=CARTESIAN_POINT('',(-31.4686665574919,30.0112662655011,179.));
#28868=CARTESIAN_POINT('Origin',(-32.,32.,179.));
#28869=CARTESIAN_POINT('Ctrl Pts',(-31.4686656825477,30.0112635882183,179.));
#28870=CARTESIAN_POINT('Ctrl Pts',(-32.1131054357931,29.8400086888077,178.963685183163));
#28871=CARTESIAN_POINT('Ctrl Pts',(-33.4929539281089,30.1591334335668,178.895660276675));
#28872=CARTESIAN_POINT('Ctrl Pts',(-34.051753790298,31.4182518043251,178.827635370188));
#28873=CARTESIAN_POINT('Ctrl Pts',(-34.0565967526292,32.0015021117824,178.795925280538));
#28874=CARTESIAN_POINT('Origin',(-32.,-32.,172.));
#28875=CARTESIAN_POINT('',(-33.6685050984025,-31.9993848812913,166.67148036339));
#28876=CARTESIAN_POINT('',(-33.6648360717667,-31.9985292840412,166.47851963661));
#28877=CARTESIAN_POINT('',(-33.666,-32.,172.));
#28878=CARTESIAN_POINT('',(-31.324922814325,-33.5230977622533,166.));
#28879=CARTESIAN_POINT('Ctrl Pts',(-33.6648360717667,-31.9985292840412,
166.47851963661));
#28880=CARTESIAN_POINT('Ctrl Pts',(-33.6661874534241,-31.8287853144728,
166.467186143366));
#28881=CARTESIAN_POINT('Ctrl Pts',(-33.6423113385545,-31.6594223896045,
166.455852650123));
#28882=CARTESIAN_POINT('Ctrl Pts',(-33.5916296652012,-31.4985231924663,
166.444519156879));
#28883=CARTESIAN_POINT('Ctrl Pts',(-33.4259777767092,-30.9726278520149,
166.407475893806));
#28884=CARTESIAN_POINT('Ctrl Pts',(-32.9739636477032,-30.5371500284145,
166.370432630732));
#28885=CARTESIAN_POINT('Ctrl Pts',(-32.4421510491472,-30.390950974798,166.333389367659));
#28886=CARTESIAN_POINT('Ctrl Pts',(-31.9103384505912,-30.2447519211814,
166.296346104586));
#28887=CARTESIAN_POINT('Ctrl Pts',(-31.2987273824852,-30.3878316375487,
166.259302841513));
#28888=CARTESIAN_POINT('Ctrl Pts',(-30.8877524141389,-30.7555629540326,
166.222259578439));
#28889=CARTESIAN_POINT('Ctrl Pts',(-30.4767774457927,-31.1232942705165,
166.185216315366));
#28890=CARTESIAN_POINT('Ctrl Pts',(-30.2664385772063,-31.715677187117,166.148173052293));
#28891=CARTESIAN_POINT('Ctrl Pts',(-30.3518675885088,-32.2595123446316,
166.11112978922));
#28892=CARTESIAN_POINT('Ctrl Pts',(-30.4372965998113,-32.803347502146,166.074086526147));
#28893=CARTESIAN_POINT('Ctrl Pts',(-30.8184934910026,-33.2986349005746,
166.037043263073));
#28894=CARTESIAN_POINT('Ctrl Pts',(-31.3249228143249,-33.5230977622533,
166.));
#28895=CARTESIAN_POINT('',(-33.666,-32.,166.));
#28896=CARTESIAN_POINT('Origin',(-32.,-32.,166.));
#28897=CARTESIAN_POINT('',(-33.666,-32.,165.));
#28898=CARTESIAN_POINT('',(-33.666,-32.,172.));
#28899=CARTESIAN_POINT('Origin',(-32.,-32.,165.));
#28900=CARTESIAN_POINT('',(-33.6146845439263,-32.4224457957945,166.));
#28901=CARTESIAN_POINT('Origin',(-32.,-32.,166.));
#28902=CARTESIAN_POINT('Ctrl Pts',(-33.6146867820777,-32.422446252051,166.));
#28903=CARTESIAN_POINT('Ctrl Pts',(-33.4771459066945,-32.9453079307942,
166.036314816837));
#28904=CARTESIAN_POINT('Ctrl Pts',(-33.0618726640047,-33.3962489478611,
166.072629633674));
#28905=CARTESIAN_POINT('Ctrl Pts',(-32.5515457289897,-33.5749074758773,
166.108944450512));
#28906=CARTESIAN_POINT('Ctrl Pts',(-32.0309820430471,-33.7571497513442,
166.145987713585));
#28907=CARTESIAN_POINT('Ctrl Pts',(-31.4115130155003,-33.6560764402868,
166.183030976658));
#28908=CARTESIAN_POINT('Ctrl Pts',(-30.9761439618779,-33.3177567144518,
166.220074239731));
#28909=CARTESIAN_POINT('Ctrl Pts',(-30.5407749082555,-32.9794369886167,
166.257117502805));
#28910=CARTESIAN_POINT('Ctrl Pts',(-30.2895058285574,-32.4038708480041,
166.294160765878));
#28911=CARTESIAN_POINT('Ctrl Pts',(-30.3375418344799,-31.8545228184461,
166.331204028951));
#28912=CARTESIAN_POINT('Ctrl Pts',(-30.3855778404025,-31.3051747888881,
166.368247292024));
#28913=CARTESIAN_POINT('Ctrl Pts',(-30.7329189319458,-30.7820448703847,
166.405290555098));
#28914=CARTESIAN_POINT('Ctrl Pts',(-31.2205128528787,-30.524470987755,166.442333818171));
#28915=CARTESIAN_POINT('Ctrl Pts',(-31.7081067738115,-30.2668971051253,
166.479377081244));
#28916=CARTESIAN_POINT('Ctrl Pts',(-32.3359535241339,-30.2748792583693,
166.516420344317));
#28917=CARTESIAN_POINT('Ctrl Pts',(-32.8168082811324,-30.5447862155172,
166.553463607391));
#28918=CARTESIAN_POINT('Ctrl Pts',(-33.2976630381309,-30.8146931726652,
166.590506870464));
#28919=CARTESIAN_POINT('Ctrl Pts',(-33.6315258018055,-31.3465249337172,
166.627550133537));
#28920=CARTESIAN_POINT('Ctrl Pts',(-33.6655960406503,-31.89690767857,166.66459339661));
#28921=CARTESIAN_POINT('Ctrl Pts',(-33.6677074511438,-31.9310161539537,
166.666889052204));
#28922=CARTESIAN_POINT('Ctrl Pts',(-33.66866748929,-31.965195875576,166.669184707797));
#28923=CARTESIAN_POINT('Ctrl Pts',(-33.6685050984025,-31.9993848812913,
166.67148036339));
#28924=CARTESIAN_POINT('Origin',(-32.,-32.,172.));
#28925=CARTESIAN_POINT('',(-33.6641555841304,-31.9988695272541,167.37148036339));
#28926=CARTESIAN_POINT('',(-33.6638025332639,-32.0008966213188,167.17851963661));
#28927=CARTESIAN_POINT('',(-33.666,-32.,172.));
#28928=CARTESIAN_POINT('Ctrl Pts',(-33.6638025332639,-32.0008966213188,
167.17851963661));
#28929=CARTESIAN_POINT('Ctrl Pts',(-33.6621591514203,-31.6647641050848,
167.156112388472));
#28930=CARTESIAN_POINT('Ctrl Pts',(-33.5633805945885,-31.3277436228238,
167.133705140335));
#28931=CARTESIAN_POINT('Ctrl Pts',(-33.374109387648,-31.053083959077,167.111297892197));
#28932=CARTESIAN_POINT('Ctrl Pts',(-33.061209603263,-30.5990215004767,167.074254629124));
#28933=CARTESIAN_POINT('Ctrl Pts',(-32.500992385075,-30.3153918625114,167.037211366051));
#28934=CARTESIAN_POINT('Ctrl Pts',(-31.9498062283038,-30.3319766798985,
167.000168102978));
#28935=CARTESIAN_POINT('Ctrl Pts',(-31.3986200715327,-30.3485614972856,
166.963124839904));
#28936=CARTESIAN_POINT('Ctrl Pts',(-30.8564649761784,-30.6653607700251,
166.926081576831));
#28937=CARTESIAN_POINT('Ctrl Pts',(-30.5714360458764,-31.1374205753515,
166.889038313758));
#28938=CARTESIAN_POINT('Ctrl Pts',(-30.2864071155743,-31.6094803806779,
166.851995050685));
#28939=CARTESIAN_POINT('Ctrl Pts',(-30.2585043503244,-32.2368007185912,
166.814951787611));
#28940=CARTESIAN_POINT('Ctrl Pts',(-30.5004798770101,-32.7322993685983,
166.777908524538));
#28941=CARTESIAN_POINT('Ctrl Pts',(-30.7424554036959,-33.2277980186054,
166.740865261465));
#28942=CARTESIAN_POINT('Ctrl Pts',(-31.2543092223174,-33.5914749807064,
166.703821998392));
#28943=CARTESIAN_POINT('Ctrl Pts',(-31.8018524330799,-33.6569621792094,
166.666778735318));
#28944=CARTESIAN_POINT('Ctrl Pts',(-32.3493956438423,-33.7224493777124,
166.629735472245));
#28945=CARTESIAN_POINT('Ctrl Pts',(-32.9326282467458,-33.4897468126174,
166.592692209172));
#28946=CARTESIAN_POINT('Ctrl Pts',(-33.2845997242085,-33.0652391014188,
166.555648946099));
#28947=CARTESIAN_POINT('Ctrl Pts',(-33.5288845123565,-32.770610749585,166.529939176269));
#28948=CARTESIAN_POINT('Ctrl Pts',(-33.6617704934304,-32.383589591023,166.504229406439));
#28949=CARTESIAN_POINT('Ctrl Pts',(-33.6648360717667,-31.9985292840412,
166.47851963661));
#28950=CARTESIAN_POINT('Ctrl Pts',(-33.6685050984025,-31.9993848812913,
166.67148036339));
#28951=CARTESIAN_POINT('Ctrl Pts',(-33.6660471100033,-32.5168780776586,
166.70622797087));
#28952=CARTESIAN_POINT('Ctrl Pts',(-33.4064339640194,-33.0364983148561,
166.74097557835));
#28953=CARTESIAN_POINT('Ctrl Pts',(-32.9900353939139,-33.3433730273871,
166.77572318583));
#28954=CARTESIAN_POINT('Ctrl Pts',(-32.5461267943179,-33.670521902698,166.812766448903));
#28955=CARTESIAN_POINT('Ctrl Pts',(-31.9240318811112,-33.7558859246661,
166.849809711976));
#28956=CARTESIAN_POINT('Ctrl Pts',(-31.4084114626267,-33.560400449204,166.88685297505));
#28957=CARTESIAN_POINT('Ctrl Pts',(-30.8927910441422,-33.3649149737418,
166.923896238123));
#28958=CARTESIAN_POINT('Ctrl Pts',(-30.48364512038,-32.8885800008494,166.960939501196));
#28959=CARTESIAN_POINT('Ctrl Pts',(-30.3681998158689,-32.3493650741656,
166.99798276427));
#28960=CARTESIAN_POINT('Ctrl Pts',(-30.2527545113577,-31.8101501474818,
167.035026027343));
#28961=CARTESIAN_POINT('Ctrl Pts',(-30.4310098260976,-31.2080552670066,
167.072069290416));
#28962=CARTESIAN_POINT('Ctrl Pts',(-30.8213955384865,-30.8185951748872,
167.109112553489));
#28963=CARTESIAN_POINT('Ctrl Pts',(-31.2117812508753,-30.4291350827678,
167.146155816562));
#28964=CARTESIAN_POINT('Ctrl Pts',(-31.8142973609132,-30.2523097790042,
167.183199079636));
#28965=CARTESIAN_POINT('Ctrl Pts',(-32.3532365279495,-30.3690338636197,
167.220242342709));
#28966=CARTESIAN_POINT('Ctrl Pts',(-32.8921756949857,-30.4857579482353,
167.257285605782));
#28967=CARTESIAN_POINT('Ctrl Pts',(-33.3675379190203,-30.8960314212301,
167.294328868855));
#28968=CARTESIAN_POINT('Ctrl Pts',(-33.561799648494,-31.4121152187214,167.331372131929));
#28969=CARTESIAN_POINT('Ctrl Pts',(-33.6319113122031,-31.5983767832275,
167.344741542416));
#28970=CARTESIAN_POINT('Ctrl Pts',(-33.6654072495738,-31.7984210409715,
167.358110952903));
#28971=CARTESIAN_POINT('Ctrl Pts',(-33.6641555841304,-31.9988695272541,
167.37148036339));
#28972=CARTESIAN_POINT('Origin',(-32.,-32.,172.));
#28973=CARTESIAN_POINT('',(-33.6644090960075,-32.0012498346086,168.07148036339));
#28974=CARTESIAN_POINT('',(-33.6681507572914,-32.0009136637507,167.87851963661));
#28975=CARTESIAN_POINT('',(-33.666,-32.,172.));
#28976=CARTESIAN_POINT('Ctrl Pts',(-33.6681507572914,-32.0009136637507,
167.87851963661));
#28977=CARTESIAN_POINT('Ctrl Pts',(-33.6648561918328,-31.5020077048909,
167.845038633578));
#28978=CARTESIAN_POINT('Ctrl Pts',(-33.4261730271947,-31.0003673015641,
167.811557630547));
#28979=CARTESIAN_POINT('Ctrl Pts',(-33.0352709879811,-30.6911682472265,
167.778076627516));
#28980=CARTESIAN_POINT('Ctrl Pts',(-32.6027783574323,-30.3490715095306,
167.741033364442));
#28981=CARTESIAN_POINT('Ctrl Pts',(-31.983952605973,-30.2425447512435,167.703990101369));
#28982=CARTESIAN_POINT('Ctrl Pts',(-31.461964987759,-30.4203339586322,167.666946838296));
#28983=CARTESIAN_POINT('Ctrl Pts',(-30.939977369545,-30.598123166021,167.629903575223));
#28984=CARTESIAN_POINT('Ctrl Pts',(-30.5148278845763,-31.0602283390857,
167.592860312149));
#28985=CARTESIAN_POINT('Ctrl Pts',(-30.3810627423918,-31.5951928206179,
167.555817049076));
#28986=CARTESIAN_POINT('Ctrl Pts',(-30.2472976002073,-32.1301573021501,
167.518773786003));
#28987=CARTESIAN_POINT('Ctrl Pts',(-30.404916800807,-32.7379810921499,167.48173052293));
#28988=CARTESIAN_POINT('Ctrl Pts',(-30.7817944276791,-33.1405269855266,
167.444687259856));
#28989=CARTESIAN_POINT('Ctrl Pts',(-31.1586720545513,-33.5430728789034,
167.407643996783));
#28990=CARTESIAN_POINT('Ctrl Pts',(-31.7548081076959,-33.7403408756571,
167.37060073371));
#28991=CARTESIAN_POINT('Ctrl Pts',(-32.2974144196609,-33.6420628913234,
167.333557470637));
#28992=CARTESIAN_POINT('Ctrl Pts',(-32.8400207316259,-33.5437849069897,
167.296514207564));
#28993=CARTESIAN_POINT('Ctrl Pts',(-33.3290973024113,-33.1499609415685,
167.25947094449));
#28994=CARTESIAN_POINT('Ctrl Pts',(-33.540844412513,-32.6408013192404,167.222427681417));
#28995=CARTESIAN_POINT('Ctrl Pts',(-33.6245069629724,-32.4396293052542,
167.207791666481));
#28996=CARTESIAN_POINT('Ctrl Pts',(-33.6648759609808,-32.2204523872831,
167.193155651546));
#28997=CARTESIAN_POINT('Ctrl Pts',(-33.6638025332639,-32.0008966213188,
167.17851963661));
#28998=CARTESIAN_POINT('Ctrl Pts',(-33.6641555841304,-31.9988695272541,
167.37148036339));
#28999=CARTESIAN_POINT('Ctrl Pts',(-33.6619392004519,-32.3538132190433,
167.395154215976));
#29000=CARTESIAN_POINT('Ctrl Pts',(-33.5507700631386,-32.7100243885523,
167.418828068562));
#29001=CARTESIAN_POINT('Ctrl Pts',(-33.341020485644,-32.9932222788685,167.442501921148));
#29002=CARTESIAN_POINT('Ctrl Pts',(-33.0128183584076,-33.4363514195366,
167.479545184222));
#29003=CARTESIAN_POINT('Ctrl Pts',(-32.4432528690221,-33.7007155788849,
167.516588447295));
#29004=CARTESIAN_POINT('Ctrl Pts',(-31.8929540065354,-33.6653431155281,
167.553631710368));
#29005=CARTESIAN_POINT('Ctrl Pts',(-31.3426551440488,-33.6299706521713,
167.590674973441));
#29006=CARTESIAN_POINT('Ctrl Pts',(-30.8116229084611,-33.2948615661094,
167.627718236515));
#29007=CARTESIAN_POINT('Ctrl Pts',(-30.5428548158509,-32.8133599755179,
167.664761499588));
#29008=CARTESIAN_POINT('Ctrl Pts',(-30.2740867232407,-32.3318583849265,
167.701804762661));
#29009=CARTESIAN_POINT('Ctrl Pts',(-30.267582773608,-31.7039642898055,167.738848025734));
#29010=CARTESIAN_POINT('Ctrl Pts',(-30.526319117194,-31.2169986148992,167.775891288808));
#29011=CARTESIAN_POINT('Ctrl Pts',(-30.78505546078,-30.7300329399929,167.812934551881));
#29012=CARTESIAN_POINT('Ctrl Pts',(-31.3090320975848,-30.3839956853014,
167.849977814954));
#29013=CARTESIAN_POINT('Ctrl Pts',(-31.8584801704804,-30.3372316264713,
167.887021078027));
#29014=CARTESIAN_POINT('Ctrl Pts',(-32.407928243376,-30.2904675676412,167.924064341101));
#29015=CARTESIAN_POINT('Ctrl Pts',(-32.9828477523625,-30.5429767046725,
167.961107604174));
#29016=CARTESIAN_POINT('Ctrl Pts',(-33.3201586422293,-30.9792122235664,
167.998150867247));
#29017=CARTESIAN_POINT('Ctrl Pts',(-33.542734764898,-31.2670642119921,168.022594032628));
#29018=CARTESIAN_POINT('Ctrl Pts',(-33.6618541900598,-31.6349121398867,
168.047037198009));
#29019=CARTESIAN_POINT('Ctrl Pts',(-33.6644090960075,-32.0012498346086,
168.07148036339));
#29020=CARTESIAN_POINT('Origin',(-32.,-32.,172.));
#29021=CARTESIAN_POINT('',(-33.6686518070233,-32.0004179215328,168.77148036339));
#29022=CARTESIAN_POINT('',(-33.666554187948,-31.9985209913767,168.57851963661));
#29023=CARTESIAN_POINT('',(-33.666,-32.,172.));
#29024=CARTESIAN_POINT('Ctrl Pts',(-33.666554187948,-31.9985209913767,168.57851963661));
#29025=CARTESIAN_POINT('Ctrl Pts',(-33.6675874565537,-31.8863118995242,
168.571008141758));
#29026=CARTESIAN_POINT('Ctrl Pts',(-33.6572223660562,-31.7742926181679,
168.563496646906));
#29027=CARTESIAN_POINT('Ctrl Pts',(-33.6347589832767,-31.6647543750453,
168.555985152054));
#29028=CARTESIAN_POINT('Ctrl Pts',(-33.5239798355562,-31.1245617720414,
168.51894188898));
#29029=CARTESIAN_POINT('Ctrl Pts',(-33.1189687606806,-30.6447083180542,
168.481898625907));
#29030=CARTESIAN_POINT('Ctrl Pts',(-32.6050566308058,-30.4447723522878,
168.444855362834));
#29031=CARTESIAN_POINT('Ctrl Pts',(-32.091144500931,-30.2448363865214,168.407812099761));
#29032=CARTESIAN_POINT('Ctrl Pts',(-31.4683313160572,-30.3248179089757,
168.370768836688));
#29033=CARTESIAN_POINT('Ctrl Pts',(-31.0216130117569,-30.6481178075245,
168.333725573614));
#29034=CARTESIAN_POINT('Ctrl Pts',(-30.5748947074566,-30.9714177060733,
168.296682310541));
#29035=CARTESIAN_POINT('Ctrl Pts',(-30.3042712837298,-31.5380359807166,
168.259639047468));
#29036=CARTESIAN_POINT('Ctrl Pts',(-30.3335785534306,-32.0886911836439,
168.222595784395));
#29037=CARTESIAN_POINT('Ctrl Pts',(-30.3628858231313,-32.6393463865712,
168.185552521321));
#29038=CARTESIAN_POINT('Ctrl Pts',(-30.6921237862596,-33.1740385177825,
168.148509258248));
#29039=CARTESIAN_POINT('Ctrl Pts',(-31.1706349329485,-33.4480953525865,
168.111465995175));
#29040=CARTESIAN_POINT('Ctrl Pts',(-31.6491460796373,-33.7221521873905,
168.074422732102));
#29041=CARTESIAN_POINT('Ctrl Pts',(-32.2769304098868,-33.7355737257871,
168.037379469028));
#29042=CARTESIAN_POINT('Ctrl Pts',(-32.7667172246232,-33.4822183541435,
168.000336205955));
#29043=CARTESIAN_POINT('Ctrl Pts',(-33.2565040393596,-33.2288629824998,
167.963292942882));
#29044=CARTESIAN_POINT('Ctrl Pts',(-33.6082933385829,-32.7087307008159,
167.926249679809));
#29045=CARTESIAN_POINT('Ctrl Pts',(-33.6611082333754,-32.1598312014215,
167.889206416735));
#29046=CARTESIAN_POINT('Ctrl Pts',(-33.666187170103,-32.107046360361,167.885644156694));
#29047=CARTESIAN_POINT('Ctrl Pts',(-33.6685012873779,-32.0539954892927,
167.882081896652));
#29048=CARTESIAN_POINT('Ctrl Pts',(-33.6681507572914,-32.0009136637507,
167.87851963661));
#29049=CARTESIAN_POINT('Ctrl Pts',(-33.6644090960075,-32.0012498346086,
168.07148036339));
#29050=CARTESIAN_POINT('Ctrl Pts',(-33.6657261130155,-32.1900916097992,
168.084080461082));
#29051=CARTESIAN_POINT('Ctrl Pts',(-33.6360689863127,-32.3785320778026,
168.096680558775));
#29052=CARTESIAN_POINT('Ctrl Pts',(-33.5736422385779,-32.5554067226683,
168.109280656467));
#29053=CARTESIAN_POINT('Ctrl Pts',(-33.3901126743126,-33.0754038021199,
168.14632391954));
#29054=CARTESIAN_POINT('Ctrl Pts',(-32.923351275035,-33.4954360602665,168.183367182613));
#29055=CARTESIAN_POINT('Ctrl Pts',(-32.386945524875,-33.6232990128118,168.220410445686));
#29056=CARTESIAN_POINT('Ctrl Pts',(-31.850539774715,-33.7511619653571,168.25745370876));
#29057=CARTESIAN_POINT('Ctrl Pts',(-31.2444896736727,-33.586855612301,168.294496971833));
#29058=CARTESIAN_POINT('Ctrl Pts',(-30.8461204624394,-33.2055656501328,
168.331540234906));
#29059=CARTESIAN_POINT('Ctrl Pts',(-30.4477512512061,-32.8242756879646,
168.36858349798));
#29060=CARTESIAN_POINT('Ctrl Pts',(-30.2570629297819,-32.2260021166843,
168.405626761053));
#29061=CARTESIAN_POINT('Ctrl Pts',(-30.3613134397796,-31.6845116783861,
168.442670024126));
#29062=CARTESIAN_POINT('Ctrl Pts',(-30.4655639497772,-31.1430212400879,
168.479713287199));
#29063=CARTESIAN_POINT('Ctrl Pts',(-30.8647532911966,-30.6583139347719,
168.516756550272));
#29064=CARTESIAN_POINT('Ctrl Pts',(-31.376214586069,-30.4521891971938,168.553799813346));
#29065=CARTESIAN_POINT('Ctrl Pts',(-31.8876758809413,-30.2460644596156,
168.590843076419));
#29066=CARTESIAN_POINT('Ctrl Pts',(-32.5114091292667,-30.3185222897753,
168.627886339492));
#29067=CARTESIAN_POINT('Ctrl Pts',(-32.96199737859,-30.6364063774491,168.664929602565));
#29068=CARTESIAN_POINT('Ctrl Pts',(-33.3940194414518,-30.9411922645955,
168.70044652284));
#29069=CARTESIAN_POINT('Ctrl Pts',(-33.6668711873007,-31.4715958446407,
168.735963443115));
#29070=CARTESIAN_POINT('Ctrl Pts',(-33.6686518070233,-32.0004179215328,
168.77148036339));
#29071=CARTESIAN_POINT('Origin',(-32.,-32.,172.));
#29072=CARTESIAN_POINT('',(-33.665635320795,-31.9984849817919,169.47148036339));
#29073=CARTESIAN_POINT('',(-33.6633165634872,-32.0000156713784,169.27851963661));
#29074=CARTESIAN_POINT('',(-33.666,-32.,172.));
#29075=CARTESIAN_POINT('Ctrl Pts',(-33.6633165634872,-32.0000156713784,
169.27851963661));
#29076=CARTESIAN_POINT('Ctrl Pts',(-33.6632931527355,-31.7210138399623,
169.259934386864));
#29077=CARTESIAN_POINT('Ctrl Pts',(-33.5968742643497,-31.4420015340208,
169.241349137118));
#29078=CARTESIAN_POINT('Ctrl Pts',(-33.4641220642516,-31.199267121124,169.222763887372));
#29079=CARTESIAN_POINT('Ctrl Pts',(-33.199526498466,-30.7154600786147,169.185720624299));
#29080=CARTESIAN_POINT('Ctrl Pts',(-32.6714110739412,-30.3757728607261,
169.148677361226));
#29081=CARTESIAN_POINT('Ctrl Pts',(-32.1214385453584,-30.3356444964945,
169.111634098152));
#29082=CARTESIAN_POINT('Ctrl Pts',(-31.5714660167756,-30.2955161322629,
169.074590835079));
#29083=CARTESIAN_POINT('Ctrl Pts',(-30.9996363841348,-30.5549466216884,
169.037547572006));
#29084=CARTESIAN_POINT('Ctrl Pts',(-30.6676157867046,-30.9952219794971,
169.000504308933));
#29085=CARTESIAN_POINT('Ctrl Pts',(-30.3355951892744,-31.4354973373059,
168.96346104586));
#29086=CARTESIAN_POINT('Ctrl Pts',(-30.2433836270549,-32.0566175634979,
168.926417782786));
#29087=CARTESIAN_POINT('Ctrl Pts',(-30.4331766109431,-32.5743614104843,
168.889374519713));
#29088=CARTESIAN_POINT('Ctrl Pts',(-30.6229695948312,-33.0921052574707,
168.85233125664));
#29089=CARTESIAN_POINT('Ctrl Pts',(-31.0947671248271,-33.5064727252516,
168.815287993566));
#29090=CARTESIAN_POINT('Ctrl Pts',(-31.6326772093758,-33.6278515073184,
168.778244730493));
#29091=CARTESIAN_POINT('Ctrl Pts',(-32.1705872939245,-33.7492302893852,
168.74120146742));
#29092=CARTESIAN_POINT('Ctrl Pts',(-32.7746099330261,-33.577620385738,168.704158204347));
#29093=CARTESIAN_POINT('Ctrl Pts',(-33.1683476422943,-33.1915495579041,
168.667114941273));
#29094=CARTESIAN_POINT('Ctrl Pts',(-33.4822446860581,-32.8837647339262,
168.637583173052));
#29095=CARTESIAN_POINT('Ctrl Pts',(-33.6624918475518,-32.4396759090301,
168.608051404831));
#29096=CARTESIAN_POINT('Ctrl Pts',(-33.666554187948,-31.9985209913767,168.57851963661));
#29097=CARTESIAN_POINT('Ctrl Pts',(-33.6686518070233,-32.0004179215328,
168.77148036339));
#29098=CARTESIAN_POINT('Ctrl Pts',(-33.6687283293138,-32.0231440971812,
168.773006706188));
#29099=CARTESIAN_POINT('Ctrl Pts',(-33.6683042216595,-32.0458673520174,
168.774533048987));
#29100=CARTESIAN_POINT('Ctrl Pts',(-33.6673706026167,-32.0685696534919,
168.776059391785));
#29101=CARTESIAN_POINT('Ctrl Pts',(-33.6447123269988,-32.6195384966732,
168.813102654858));
#29102=CARTESIAN_POINT('Ctrl Pts',(-33.3219525254415,-33.1581658378479,
168.850145917932));
#29103=CARTESIAN_POINT('Ctrl Pts',(-32.8467843330275,-33.4379787262727,
168.887189181005));
#29104=CARTESIAN_POINT('Ctrl Pts',(-32.3716161406135,-33.7177916146976,
168.924232444078));
#29105=CARTESIAN_POINT('Ctrl Pts',(-31.7440395573428,-33.7387900503725,
168.961275707151));
#29106=CARTESIAN_POINT('Ctrl Pts',(-31.2512302248365,-33.4913652629953,
168.998318970225));
#29107=CARTESIAN_POINT('Ctrl Pts',(-30.7584208923303,-33.2439404756181,
169.035362233298));
#29108=CARTESIAN_POINT('Ctrl Pts',(-30.4003788105884,-32.728092465189,169.072405496371));
#29109=CARTESIAN_POINT('Ctrl Pts',(-30.3409420948093,-32.179870484209,169.109448759444));
#29110=CARTESIAN_POINT('Ctrl Pts',(-30.2815053790303,-31.6316485032291,
169.146492022518));
#29111=CARTESIAN_POINT('Ctrl Pts',(-30.5206740292141,-31.0510525516985,
169.183535285591));
#29112=CARTESIAN_POINT('Ctrl Pts',(-30.9490057678768,-30.703760188888,169.220578548664));
#29113=CARTESIAN_POINT('Ctrl Pts',(-31.3773375065395,-30.3564678260775,
169.257621811737));
#29114=CARTESIAN_POINT('Ctrl Pts',(-31.9948323336809,-30.2424790519871,
169.294665074811));
#29115=CARTESIAN_POINT('Ctrl Pts',(-32.5189279646265,-30.4139545115617,
169.331708337884));
#29116=CARTESIAN_POINT('Ctrl Pts',(-33.0430235955722,-30.5854299711363,
169.368751600957));
#29117=CARTESIAN_POINT('Ctrl Pts',(-33.473720030322,-31.042369664376,169.40579486403));
#29118=CARTESIAN_POINT('Ctrl Pts',(-33.613932915689,-31.5756804653068,169.442838127103));
#29119=CARTESIAN_POINT('Ctrl Pts',(-33.6500709361183,-31.713134284681,169.452385539199));
#29120=CARTESIAN_POINT('Ctrl Pts',(-33.6669126403244,-31.8556613037164,
169.461932951295));
#29121=CARTESIAN_POINT('Ctrl Pts',(-33.665635320795,-31.9984849817919,169.47148036339));
#29122=CARTESIAN_POINT('Origin',(-32.,-32.,172.));
#29123=CARTESIAN_POINT('',(-33.6634609252252,-32.0005076151317,170.17148036339));
#29124=CARTESIAN_POINT('',(-33.6666117016187,-32.001470779109,169.97851963661));
#29125=CARTESIAN_POINT('',(-33.666,-32.,172.));
#29126=CARTESIAN_POINT('Ctrl Pts',(-33.6666117016187,-32.001470779109,169.97851963661));
#29127=CARTESIAN_POINT('Ctrl Pts',(-33.6625394733438,-31.5584545014678,
169.94886063197));
#29128=CARTESIAN_POINT('Ctrl Pts',(-33.4805649727493,-31.1124834122679,
169.91920162733));
#29129=CARTESIAN_POINT('Ctrl Pts',(-33.1642582886333,-30.8044544342897,
169.88954262269));
#29130=CARTESIAN_POINT('Ctrl Pts',(-32.7692001316305,-30.4197348995646,
169.852499359617));
#29131=CARTESIAN_POINT('Ctrl Pts',(-32.1645930666198,-30.2501955101854,
169.815456096544));
#29132=CARTESIAN_POINT('Ctrl Pts',(-31.6271020082049,-30.373416571443,169.778412833471));
#29133=CARTESIAN_POINT('Ctrl Pts',(-31.0896109497899,-30.4966376327006,
169.741369570397));
#29134=CARTESIAN_POINT('Ctrl Pts',(-30.6192358979707,-30.912619144595,169.704326307324));
#29135=CARTESIAN_POINT('Ctrl Pts',(-30.4312179259571,-31.431010222849,169.667283044251));
#29136=CARTESIAN_POINT('Ctrl Pts',(-30.2431999539434,-31.949401301103,169.630239781178));
#29137=CARTESIAN_POINT('Ctrl Pts',(-30.3375390617353,-32.5702019457165,
169.593196518104));
#29138=CARTESIAN_POINT('Ctrl Pts',(-30.6710661851401,-33.0093371478662,
169.556153255031));
#29139=CARTESIAN_POINT('Ctrl Pts',(-31.0045933085448,-33.4484723500159,
169.519109991958));
#29140=CARTESIAN_POINT('Ctrl Pts',(-31.5773084475623,-33.7059421097018,
169.482066728885));
#29141=CARTESIAN_POINT('Ctrl Pts',(-32.1271402599961,-33.6639296609623,
169.445023465812));
#29142=CARTESIAN_POINT('Ctrl Pts',(-32.6769720724299,-33.6219172122228,
169.407980202738));
#29143=CARTESIAN_POINT('Ctrl Pts',(-33.20392055828,-33.2804225550579,169.370936939665));
#29144=CARTESIAN_POINT('Ctrl Pts',(-33.4668569476818,-32.7957117929105,
169.333893676592));
#29145=CARTESIAN_POINT('Ctrl Pts',(-33.5978735746518,-32.5541888555298,
169.315435663264));
#29146=CARTESIAN_POINT('Ctrl Pts',(-33.6633398139666,-32.2771074292527,
169.296977649937));
#29147=CARTESIAN_POINT('Ctrl Pts',(-33.6633165634872,-32.0000156713784,
169.27851963661));
#29148=CARTESIAN_POINT('Ctrl Pts',(-33.665635320795,-31.9984849817919,169.47148036339));
#29149=CARTESIAN_POINT('Ctrl Pts',(-33.6619567336469,-32.4098067650291,
169.498976214368));
#29150=CARTESIAN_POINT('Ctrl Pts',(-33.5079993225544,-32.8235890324679,
169.526472065346));
#29151=CARTESIAN_POINT('Ctrl Pts',(-33.2318839646868,-33.1257390556495,
169.553967916323));
#29152=CARTESIAN_POINT('Ctrl Pts',(-32.8598927923331,-33.5328049364395,
169.591011179397));
#29153=CARTESIAN_POINT('Ctrl Pts',(-32.2661811116412,-33.7372547893976,
169.62805444247));
#29154=CARTESIAN_POINT('Ctrl Pts',(-31.7224281684284,-33.6455334703934,
169.665097705543));
#29155=CARTESIAN_POINT('Ctrl Pts',(-31.1786752252156,-33.5538121513892,
169.702140968616));
#29156=CARTESIAN_POINT('Ctrl Pts',(-30.6848810194818,-33.1659196604227,
169.739184231689));
#29157=CARTESIAN_POINT('Ctrl Pts',(-30.4670031022832,-32.6593534981007,
169.776227494763));
#29158=CARTESIAN_POINT('Ctrl Pts',(-30.2491251850846,-32.1527873357787,
169.813270757836));
#29159=CARTESIAN_POINT('Ctrl Pts',(-30.3071635564212,-31.5275475021012,
169.850314020909));
#29160=CARTESIAN_POINT('Ctrl Pts',(-30.6145601722693,-31.0697403547372,
169.887357283982));
#29161=CARTESIAN_POINT('Ctrl Pts',(-30.9219567881174,-30.6119332073732,
169.924400547056));
#29162=CARTESIAN_POINT('Ctrl Pts',(-31.4787116484771,-30.3215587463227,
169.961443810129));
#29163=CARTESIAN_POINT('Ctrl Pts',(-32.0300567481252,-30.3314907504724,
169.998487073202));
#29164=CARTESIAN_POINT('Ctrl Pts',(-32.5814018477734,-30.3414227546222,
170.035530336275));
#29165=CARTESIAN_POINT('Ctrl Pts',(-33.12733718671,-30.6516612239722,170.072573599349));
#29166=CARTESIAN_POINT('Ctrl Pts',(-33.4180457140488,-31.1202427171459,
170.109616862422));
#29167=CARTESIAN_POINT('Ctrl Pts',(-33.5798767351351,-31.3810916925667,
170.130238029411));
#29168=CARTESIAN_POINT('Ctrl Pts',(-33.66261543862,-31.6910096378651,170.150859196401));
#29169=CARTESIAN_POINT('Ctrl Pts',(-33.6634609252252,-32.0005076151317,
170.17148036339));
#29170=CARTESIAN_POINT('Origin',(-32.,-32.,172.));
#29171=CARTESIAN_POINT('',(-33.6674948610292,-32.0012453678407,170.87148036339));
#29172=CARTESIAN_POINT('',(-33.6681095677655,-31.9990590647821,170.67851963661));
#29173=CARTESIAN_POINT('',(-33.666,-32.,172.));
#29174=CARTESIAN_POINT('Ctrl Pts',(-33.6681095677655,-31.9990590647821,
170.67851963661));
#29175=CARTESIAN_POINT('Ctrl Pts',(-33.668481259833,-31.9440776933425,170.674830140149));
#29176=CARTESIAN_POINT('Ctrl Pts',(-33.6659984917278,-31.8891303002658,
170.671140643689));
#29177=CARTESIAN_POINT('Ctrl Pts',(-33.6605508651237,-31.8344784404443,
170.667451147228));
#29178=CARTESIAN_POINT('Ctrl Pts',(-33.6058556329738,-31.2857631231863,
170.630407884155));
#29179=CARTESIAN_POINT('Ctrl Pts',(-33.2522863246199,-30.7668391867544,
170.593364621082));
#29180=CARTESIAN_POINT('Ctrl Pts',(-32.7616343384148,-30.515163410712,170.556321358009));
#29181=CARTESIAN_POINT('Ctrl Pts',(-32.2709823522098,-30.2634876346696,
170.519278094936));
#29182=CARTESIAN_POINT('Ctrl Pts',(-31.6432476881537,-30.2790600190167,
170.482234831862));
#29183=CARTESIAN_POINT('Ctrl Pts',(-31.1656783247691,-30.5547547251138,
170.445191568789));
#29184=CARTESIAN_POINT('Ctrl Pts',(-30.6881089613846,-30.8304494312109,
170.408148305716));
#29185=CARTESIAN_POINT('Ctrl Pts',(-30.3607048986715,-31.3662664590579,
170.371105042643));
#29186=CARTESIAN_POINT('Ctrl Pts',(-30.3332844604529,-31.917018842059,170.334061779569));
#29187=CARTESIAN_POINT('Ctrl Pts',(-30.3058640222343,-32.4677712250601,
170.297018516496));
#29188=CARTESIAN_POINT('Ctrl Pts',(-30.5784272085101,-33.0334589632152,
170.259975253423));
#29189=CARTESIAN_POINT('Ctrl Pts',(-31.0262505831528,-33.3552264148587,
170.22293199035));
#29190=CARTESIAN_POINT('Ctrl Pts',(-31.4740739577955,-33.6769938665021,
170.185888727276));
#29191=CARTESIAN_POINT('Ctrl Pts',(-32.0971575208052,-33.7548410316338,
170.148845464203));
#29192=CARTESIAN_POINT('Ctrl Pts',(-32.6103816122786,-33.5531454695981,
170.11180220113));
#29193=CARTESIAN_POINT('Ctrl Pts',(-33.1236057037519,-33.3514499075625,
170.074758938057));
#29194=CARTESIAN_POINT('Ctrl Pts',(-33.5269703236889,-32.8702116183596,
170.037715674983));
#29195=CARTESIAN_POINT('Ctrl Pts',(-33.6358980091599,-32.3296426337226,
170.00067241191));
#29196=CARTESIAN_POINT('Ctrl Pts',(-33.6576118138667,-32.2218848188732,
169.993288153477));
#29197=CARTESIAN_POINT('Ctrl Pts',(-33.6676255719879,-32.1117693789459,
169.985903895043));
#29198=CARTESIAN_POINT('Ctrl Pts',(-33.6666117016187,-32.001470779109,169.97851963661));
#29199=CARTESIAN_POINT('Ctrl Pts',(-33.6634609252252,-32.0005076151317,
170.17148036339));
#29200=CARTESIAN_POINT('Ctrl Pts',(-33.6641342461035,-32.2469827793654,
170.187902459474));
#29201=CARTESIAN_POINT('Ctrl Pts',(-33.6128703552766,-32.4931915971372,
170.204324555558));
#29202=CARTESIAN_POINT('Ctrl Pts',(-33.5082546205404,-32.714139008517,170.220746651642));
#29203=CARTESIAN_POINT('Ctrl Pts',(-33.2722732839521,-33.2125292897169,
170.257789914715));
#29204=CARTESIAN_POINT('Ctrl Pts',(-32.7648288950345,-33.5823853351191,
170.294833177788));
#29205=CARTESIAN_POINT('Ctrl Pts',(-32.2181252546536,-33.6544630238084,
170.331876440861));
#29206=CARTESIAN_POINT('Ctrl Pts',(-31.6714216142728,-33.7265407124978,
170.368919703935));
#29207=CARTESIAN_POINT('Ctrl Pts',(-31.0854587224287,-33.5008400444744,
170.405962967008));
#29208=CARTESIAN_POINT('Ctrl Pts',(-30.7283700211778,-33.0806404216147,
170.443006230081));
#29209=CARTESIAN_POINT('Ctrl Pts',(-30.3712813199269,-32.6604407987551,
170.480049493154));
#29210=CARTESIAN_POINT('Ctrl Pts',(-30.2430668092691,-32.0457422210593,
170.517092756228));
#29211=CARTESIAN_POINT('Ctrl Pts',(-30.4023967540672,-31.5178274246166,
170.554136019301));
#29212=CARTESIAN_POINT('Ctrl Pts',(-30.5617266988653,-30.989912628174,170.591179282374));
#29213=CARTESIAN_POINT('Ctrl Pts',(-31.0086010991193,-30.5487816129845,
170.628222545447));
#29214=CARTESIAN_POINT('Ctrl Pts',(-31.5385326523485,-30.3962935396656,
170.66526580852));
#29215=CARTESIAN_POINT('Ctrl Pts',(-32.0684642055777,-30.2438054663466,
170.702309071594));
#29216=CARTESIAN_POINT('Ctrl Pts',(-32.6814529117821,-30.3799603348982,
170.739352334667));
#29217=CARTESIAN_POINT('Ctrl Pts',(-33.0969984627955,-30.7424544157402,
170.77639559774));
#29218=CARTESIAN_POINT('Ctrl Pts',(-33.4525471560164,-31.0526112599884,
170.808090519624));
#29219=CARTESIAN_POINT('Ctrl Pts',(-33.6635508796099,-31.528467414169,170.839785441507));
#29220=CARTESIAN_POINT('Ctrl Pts',(-33.6674948610292,-32.0012453678407,
170.87148036339));
#29221=CARTESIAN_POINT('Origin',(-32.,-32.,172.));
#29222=CARTESIAN_POINT('',(-33.6673390318703,-31.9986999066965,171.57148036339));
#29223=CARTESIAN_POINT('',(-33.6637722109972,-31.999128635268,171.37851963661));
#29224=CARTESIAN_POINT('',(-33.666,-32.,172.));
#29225=CARTESIAN_POINT('Ctrl Pts',(-33.6637722109972,-31.999128635268,171.37851963661));
#29226=CARTESIAN_POINT('Ctrl Pts',(-33.6648226268342,-31.7776542933398,
171.363756385255));
#29227=CARTESIAN_POINT('Ctrl Pts',(-33.6237243170056,-31.5565539606062,
171.348993133901));
#29228=CARTESIAN_POINT('Ctrl Pts',(-33.5386395965288,-31.3539235692779,
171.334229882547));
#29229=CARTESIAN_POINT('Ctrl Pts',(-33.3251489765771,-30.8454928237421,
171.297186619474));
#29230=CARTESIAN_POINT('Ctrl Pts',(-32.8347264675265,-30.4533460779589,
171.2601433564));
#29231=CARTESIAN_POINT('Ctrl Pts',(-32.2917867503132,-30.3569275564715,
171.223100093327));
#29232=CARTESIAN_POINT('Ctrl Pts',(-31.7488470330999,-30.2605090349842,
171.186056830254));
#29233=CARTESIAN_POINT('Ctrl Pts',(-31.1533901077238,-30.4598187377927,
171.149013567181));
#29234=CARTESIAN_POINT('Ctrl Pts',(-30.7778938345064,-30.8636536256037,
171.111970304108));
#29235=CARTESIAN_POINT('Ctrl Pts',(-30.4023975612891,-31.2674885134147,
171.074927041034));
#29236=CARTESIAN_POINT('Ctrl Pts',(-30.2468619402303,-31.8758485862283,
171.037883777961));
#29237=CARTESIAN_POINT('Ctrl Pts',(-30.3824592281699,-32.4103515734201,
171.000840514888));
#29238=CARTESIAN_POINT('Ctrl Pts',(-30.5180565161095,-32.9448545606118,
170.963797251814));
#29239=CARTESIAN_POINT('Ctrl Pts',(-30.9447867130474,-33.4055004621818,
170.926753988741));
#29240=CARTESIAN_POINT('Ctrl Pts',(-31.467380394713,-33.5815002113199,170.889710725668));
#29241=CARTESIAN_POINT('Ctrl Pts',(-31.9899740763786,-33.757499960458,170.852667462595));
#29242=CARTESIAN_POINT('Ctrl Pts',(-32.6084312427719,-33.6488535571644,
170.815624199522));
#29243=CARTESIAN_POINT('Ctrl Pts',(-33.0397492479957,-33.3052770064754,
170.778580936448));
#29244=CARTESIAN_POINT('Ctrl Pts',(-33.4281081259296,-32.9959205639111,
170.745227169835));
#29245=CARTESIAN_POINT('Ctrl Pts',(-33.6647493990804,-32.4961013714264,
170.711873403223));
#29246=CARTESIAN_POINT('Ctrl Pts',(-33.6681095677655,-31.9990590647821,
170.67851963661));
#29247=CARTESIAN_POINT('Ctrl Pts',(-33.6674948610292,-32.0012453678407,
170.87148036339));
#29248=CARTESIAN_POINT('Ctrl Pts',(-33.6681603858837,-32.0810240091201,
170.87682870458));
#29249=CARTESIAN_POINT('Ctrl Pts',(-33.6629299510325,-32.1607149996279,
170.88217704577));
#29250=CARTESIAN_POINT('Ctrl Pts',(-33.651503176545,-32.2395073730154,170.88752538696));
#29251=CARTESIAN_POINT('Ctrl Pts',(-33.5723599434589,-32.7852329563164,
170.924568650033));
#29252=CARTESIAN_POINT('Ctrl Pts',(-33.1959710814645,-33.2878508297859,
170.961611913106));
#29253=CARTESIAN_POINT('Ctrl Pts',(-32.6945700929267,-33.5173657798562,
170.99865517618));
#29254=CARTESIAN_POINT('Ctrl Pts',(-32.193169104389,-33.7468807299266,171.035698439253));
#29255=CARTESIAN_POINT('Ctrl Pts',(-31.5667559893079,-33.7032927565979,
171.072741702326));
#29256=CARTESIAN_POINT('Ctrl Pts',(-31.1019739925609,-33.4065474801193,
171.109784965399));
#29257=CARTESIAN_POINT('Ctrl Pts',(-30.6371919958139,-33.1098022036407,
171.146828228473));
#29258=CARTESIAN_POINT('Ctrl Pts',(-30.334041117401,-32.5598996240123,171.183871491546));
#29259=CARTESIAN_POINT('Ctrl Pts',(-30.3312415555168,-32.0084721799494,
171.220914754619));
#29260=CARTESIAN_POINT('Ctrl Pts',(-30.3284419936326,-31.4570447358866,
171.257958017692));
#29261=CARTESIAN_POINT('Ctrl Pts',(-30.625993748277,-30.9040924273892,171.295001280766));
#29262=CARTESIAN_POINT('Ctrl Pts',(-31.087738749932,-30.6026432325668,171.332044543839));
#29263=CARTESIAN_POINT('Ctrl Pts',(-31.549483751587,-30.3011940377444,171.369087806912));
#29264=CARTESIAN_POINT('Ctrl Pts',(-32.1754220002525,-30.2512479565968,
171.406131069985));
#29265=CARTESIAN_POINT('Ctrl Pts',(-32.6791275473481,-30.4756600450359,
171.443174333058));
#29266=CARTESIAN_POINT('Ctrl Pts',(-33.1828330944437,-30.700072133475,171.480217596132));
#29267=CARTESIAN_POINT('Ctrl Pts',(-33.5643059399693,-31.1988423915007,
171.517260859205));
#29268=CARTESIAN_POINT('Ctrl Pts',(-33.6489861782628,-31.7437362535097,
171.554304122278));
#29269=CARTESIAN_POINT('Ctrl Pts',(-33.6620743718116,-31.8279551512505,
171.560029535982));
#29270=CARTESIAN_POINT('Ctrl Pts',(-33.6680725307781,-31.9132758889271,
171.565754949686));
#29271=CARTESIAN_POINT('Ctrl Pts',(-33.6673390318703,-31.9986999066965,
171.57148036339));
#29272=CARTESIAN_POINT('Origin',(-32.,-32.,172.));
#29273=CARTESIAN_POINT('',(-33.6634139074877,-31.999580988466,172.27148036339));
#29274=CARTESIAN_POINT('',(-33.6649323450731,-32.0014151634909,172.07851963661));
#29275=CARTESIAN_POINT('',(-33.666,-32.,172.));
#29276=CARTESIAN_POINT('Ctrl Pts',(-33.6649323450731,-32.0014151634909,
172.07851963661));
#29277=CARTESIAN_POINT('Ctrl Pts',(-33.6618075747334,-31.6144944764027,
172.052682630362));
#29278=CARTESIAN_POINT('Ctrl Pts',(-33.5274443578025,-31.22561670968,172.026845624113));
#29279=CARTESIAN_POINT('Ctrl Pts',(-33.2809243786464,-30.9303929232983,
172.001008617865));
#29280=CARTESIAN_POINT('Ctrl Pts',(-32.9274815550867,-30.5071220427884,
171.963965354792));
#29281=CARTESIAN_POINT('Ctrl Pts',(-32.3434916893401,-30.2763642816683,
171.926922091719));
#29282=CARTESIAN_POINT('Ctrl Pts',(-31.796185377419,-30.3437131401949,171.889878828646));
#29283=CARTESIAN_POINT('Ctrl Pts',(-31.2488790654979,-30.4110619987214,
171.852835565572));
#29284=CARTESIAN_POINT('Ctrl Pts',(-30.7382563074024,-30.7765174768945,
171.815792302499));
#29285=CARTESIAN_POINT('Ctrl Pts',(-30.4979753085002,-31.272849129502,171.778749039426));
#29286=CARTESIAN_POINT('Ctrl Pts',(-30.2576943095981,-31.7691807821095,
171.741705776353));
#29287=CARTESIAN_POINT('Ctrl Pts',(-30.2877550698894,-32.3963886091514,
171.704662513279));
#29288=CARTESIAN_POINT('Ctrl Pts',(-30.5744019484625,-32.8674657098661,
171.667619250206));
#29289=CARTESIAN_POINT('Ctrl Pts',(-30.8610488270356,-33.3385428105808,
171.630575987133));
#29290=CARTESIAN_POINT('Ctrl Pts',(-31.4042818238906,-33.6534891849684,
171.59353272406));
#29291=CARTESIAN_POINT('Ctrl Pts',(-31.9555204652248,-33.6681870798346,
171.556489460986));
#29292=CARTESIAN_POINT('Ctrl Pts',(-32.506759106559,-33.6828849747009,171.519446197913));
#29293=CARTESIAN_POINT('Ctrl Pts',(-33.0660033923725,-33.3973343900459,
171.48240293484));
#29294=CARTESIAN_POINT('Ctrl Pts',(-33.3773461698529,-32.9422017250741,
171.445359671767));
#29295=CARTESIAN_POINT('Ctrl Pts',(-33.5646061506259,-32.6684579922612,
171.423079660048));
#29296=CARTESIAN_POINT('Ctrl Pts',(-33.6621869723126,-32.3333674025406,
171.400799648329));
#29297=CARTESIAN_POINT('Ctrl Pts',(-33.6637722109972,-31.999128635268,171.37851963661));
#29298=CARTESIAN_POINT('Ctrl Pts',(-33.6673390318703,-31.9986999066965,
171.57148036339));
#29299=CARTESIAN_POINT('Ctrl Pts',(-33.6633268138032,-32.4659668430872,
171.60279821276));
#29300=CARTESIAN_POINT('Ctrl Pts',(-33.4578994378697,-32.9363239805219,
171.634116062129));
#29301=CARTESIAN_POINT('Ctrl Pts',(-33.1097105413418,-33.2463422637068,
171.665433911498));
#29302=CARTESIAN_POINT('Ctrl Pts',(-32.697867035066,-33.6130369459029,171.702477174571));
#29303=CARTESIAN_POINT('Ctrl Pts',(-32.0862923914529,-33.7554088443029,
171.739520437645));
#29304=CARTESIAN_POINT('Ctrl Pts',(-31.5548398512946,-33.6083093501785,
171.776563700718));
#29305=CARTESIAN_POINT('Ctrl Pts',(-31.0233873111362,-33.4612098560541,
171.813606963791));
#29306=CARTESIAN_POINT('Ctrl Pts',(-30.5720568744324,-33.0246389694052,
171.850650226864));
#29307=CARTESIAN_POINT('Ctrl Pts',(-30.4073749017817,-32.4983691607554,
171.887693489938));
#29308=CARTESIAN_POINT('Ctrl Pts',(-30.2426929291309,-31.9720993521056,
171.924736753011));
#29309=CARTESIAN_POINT('Ctrl Pts',(-30.364659420533,-31.3561306214548,171.961780016084));
#29310=CARTESIAN_POINT('Ctrl Pts',(-30.7174631708582,-30.9323269199975,
171.998823279157));
#29311=CARTESIAN_POINT('Ctrl Pts',(-31.0702669211834,-30.5085232185402,
172.035866542231));
#29312=CARTESIAN_POINT('Ctrl Pts',(-31.6539079304317,-30.2768845462763,
172.072909805304));
#29313=CARTESIAN_POINT('Ctrl Pts',(-32.2013152374326,-30.3434075036254,
172.109953068377));
#29314=CARTESIAN_POINT('Ctrl Pts',(-32.7487225444335,-30.4099304609746,
172.14699633145));
#29315=CARTESIAN_POINT('Ctrl Pts',(-33.259896149187,-30.7746150479367,172.184039594523));
#29316=CARTESIAN_POINT('Ctrl Pts',(-33.5009257818815,-31.2705835749378,
172.221082857597));
#29317=CARTESIAN_POINT('Ctrl Pts',(-33.6102330377975,-31.4955059552325,
172.237882026195));
#29318=CARTESIAN_POINT('Ctrl Pts',(-33.6639815538493,-31.7474286428721,
172.254681194792));
#29319=CARTESIAN_POINT('Ctrl Pts',(-33.6634139074877,-31.999580988466,172.27148036339));
#29320=CARTESIAN_POINT('Origin',(-32.,-32.,172.));
#29321=CARTESIAN_POINT('',(-33.6658031255686,-32.0015218482784,172.97148036339));
#29322=CARTESIAN_POINT('',(-33.6687793242584,-32.0000368508118,172.77851963661));
#29323=CARTESIAN_POINT('',(-33.666,-32.,172.));
#29324=CARTESIAN_POINT('Ctrl Pts',(-33.6687789306113,-32.0000368455925,
172.77851963661));
#29325=CARTESIAN_POINT('Ctrl Pts',(-33.6686001379207,-31.4505738269769,
172.741608875468));
#29326=CARTESIAN_POINT('Ctrl Pts',(-33.3706978307467,-30.9009446699073,
172.704698114326));
#29327=CARTESIAN_POINT('Ctrl Pts',(-32.9101517626888,-30.6012683133584,
172.667787353184));
#29328=CARTESIAN_POINT('Ctrl Pts',(-32.4479524303382,-30.300516181216,172.63074409011));
#29329=CARTESIAN_POINT('Ctrl Pts',(-31.8219395268455,-30.2515146274405,
172.593700827037));
#29330=CARTESIAN_POINT('Ctrl Pts',(-31.3185731624352,-30.4766864973396,
172.556657563964));
#29331=CARTESIAN_POINT('Ctrl Pts',(-30.8152067980249,-30.7018583672388,
172.519614300891));
#29332=CARTESIAN_POINT('Ctrl Pts',(-30.4344869726971,-31.2012036608125,
172.482571037817));
#29333=CARTESIAN_POINT('Ctrl Pts',(-30.3506290141545,-31.7462246793086,
172.445527774744));
#29334=CARTESIAN_POINT('Ctrl Pts',(-30.2667710556119,-32.2912456978048,
172.408484511671));
#29335=CARTESIAN_POINT('Ctrl Pts',(-30.4797749638545,-32.8819424412233,
172.371441248598));
#29336=CARTESIAN_POINT('Ctrl Pts',(-30.8921713054361,-33.2480152826956,
172.334397985524));
#29337=CARTESIAN_POINT('Ctrl Pts',(-31.3045676470177,-33.6140881241679,
172.297354722451));
#29338=CARTESIAN_POINT('Ctrl Pts',(-31.9163564219383,-33.755537063694,172.260311459378));
#29339=CARTESIAN_POINT('Ctrl Pts',(-32.4475864040807,-33.6076358335217,
172.223268196305));
#29340=CARTESIAN_POINT('Ctrl Pts',(-32.9788163862231,-33.4597346033494,
172.186224933231));
#29341=CARTESIAN_POINT('Ctrl Pts',(-33.4294875755873,-33.0224832034787,
172.149181670158));
#29342=CARTESIAN_POINT('Ctrl Pts',(-33.593375279583,-32.4959655035934,172.112138407085));
#29343=CARTESIAN_POINT('Ctrl Pts',(-33.6429542731456,-32.3366843798927,
172.10093215026));
#29344=CARTESIAN_POINT('Ctrl Pts',(-33.6662876483389,-32.1692338553619,
172.089725893435));
#29345=CARTESIAN_POINT('Ctrl Pts',(-33.6649323450731,-32.0014151634909,
172.07851963661));
#29346=CARTESIAN_POINT('Ctrl Pts',(-33.6634139074877,-31.999580988466,172.27148036339));
#29347=CARTESIAN_POINT('Ctrl Pts',(-33.6627298565773,-32.3034410203875,
172.291724457866));
#29348=CARTESIAN_POINT('Ctrl Pts',(-33.5831688370359,-32.6076345575211,
172.311968552341));
#29349=CARTESIAN_POINT('Ctrl Pts',(-33.4269053276148,-32.8653136482753,
172.332212646816));
#29350=CARTESIAN_POINT('Ctrl Pts',(-33.1409695800183,-33.3368227275717,
172.36925590989));
#29351=CARTESIAN_POINT('Ctrl Pts',(-32.5982124241901,-33.6525884191244,
172.406299172963));
#29352=CARTESIAN_POINT('Ctrl Pts',(-32.0469965916589,-33.668118054647,172.443342436036));
#29353=CARTESIAN_POINT('Ctrl Pts',(-31.4957807591278,-33.6836476901697,
172.480385699109));
#29354=CARTESIAN_POINT('Ctrl Pts',(-30.9361062498938,-33.3989412696623,
172.517428962183));
#29355=CARTESIAN_POINT('Ctrl Pts',(-30.6240770846737,-32.9442789073928,
172.554472225256));
#29356=CARTESIAN_POINT('Ctrl Pts',(-30.3120479194536,-32.4896165451233,
172.591515488329));
#29357=CARTESIAN_POINT('Ctrl Pts',(-30.2476640982474,-31.8649982410916,
172.628558751402));
#29358=CARTESIAN_POINT('Ctrl Pts',(-30.4603873085324,-31.356245944371,172.665602014476));
#29359=CARTESIAN_POINT('Ctrl Pts',(-30.6731105188173,-30.8474936476504,
172.702645277549));
#29360=CARTESIAN_POINT('Ctrl Pts',(-31.1629407605934,-30.4546073582408,
172.739688540622));
#29361=CARTESIAN_POINT('Ctrl Pts',(-31.7057343712178,-30.3573697118388,
172.776731803695));
#29362=CARTESIAN_POINT('Ctrl Pts',(-32.2485279818422,-30.2601320654369,
172.813775066769));
#29363=CARTESIAN_POINT('Ctrl Pts',(-32.8442849613149,-30.4585430620426,
172.850818329842));
#29364=CARTESIAN_POINT('Ctrl Pts',(-33.2203901461869,-30.8618109054481,
172.887861592915));
#29365=CARTESIAN_POINT('Ctrl Pts',(-33.5033876516186,-31.1652467481191,
172.915734516407));
#29366=CARTESIAN_POINT('Ctrl Pts',(-33.6620249806223,-31.5846663170183,
172.943607439898));
#29367=CARTESIAN_POINT('Ctrl Pts',(-33.6658031255686,-32.0015218482784,
172.97148036339));
#29368=CARTESIAN_POINT('Origin',(-32.,-32.,172.));
#29369=CARTESIAN_POINT('',(-33.668584334028,-31.9994831966231,173.67148036339));
#29370=CARTESIAN_POINT('',(-33.665039714177,-31.9985615025105,173.47851963661));
#29371=CARTESIAN_POINT('',(-33.666,-32.,172.));
#29372=CARTESIAN_POINT('Ctrl Pts',(-33.665039714177,-31.9985615025105,173.47851963661));
#29373=CARTESIAN_POINT('Ctrl Pts',(-33.6663911314701,-31.8347380945258,
173.467578383647));
#29374=CARTESIAN_POINT('Ctrl Pts',(-33.6441694753636,-31.6712733003014,
173.456637130684));
#29375=CARTESIAN_POINT('Ctrl Pts',(-33.5968738937745,-31.5154173654344,
173.445695877722));
#29376=CARTESIAN_POINT('Ctrl Pts',(-33.4367475648267,-30.9877435773881,
173.408652614648));
#29377=CARTESIAN_POINT('Ctrl Pts',(-32.9892080527959,-30.5472873448482,
173.371609351575));
#29378=CARTESIAN_POINT('Ctrl Pts',(-32.4590470117056,-30.3955990515507,
173.334566088502));
#29379=CARTESIAN_POINT('Ctrl Pts',(-31.9288859706153,-30.2439107582531,
173.297522825429));
#29380=CARTESIAN_POINT('Ctrl Pts',(-31.3161034004654,-30.3809904041979,
173.260479562355));
#29381=CARTESIAN_POINT('Ctrl Pts',(-30.9011052826813,-30.744111086684,173.223436299282));
#29382=CARTESIAN_POINT('Ctrl Pts',(-30.4861071648973,-31.1072317691701,
173.186393036209));
#29383=CARTESIAN_POINT('Ctrl Pts',(-30.2688934994791,-31.6963934881976,
173.149349773136));
#29384=CARTESIAN_POINT('Ctrl Pts',(-30.3488600819301,-32.241999035736,173.112306510062));
#29385=CARTESIAN_POINT('Ctrl Pts',(-30.4288266643811,-32.7876045832743,
173.075263246989));
#29386=CARTESIAN_POINT('Ctrl Pts',(-30.8059734947013,-33.2896539593234,
173.038219983916));
#29387=CARTESIAN_POINT('Ctrl Pts',(-31.3077202283297,-33.5184120916527,
173.001176720843));
#29388=CARTESIAN_POINT('Ctrl Pts',(-31.809466961958,-33.7471702239819,172.96413345777));
#29389=CARTESIAN_POINT('Ctrl Pts',(-32.4358135988946,-33.7026371125912,
172.927090194696));
#29390=CARTESIAN_POINT('Ctrl Pts',(-32.9001473143004,-33.4051908677823,
172.890046931623));
#29391=CARTESIAN_POINT('Ctrl Pts',(-33.3644810297062,-33.1077446229734,
172.85300366855));
#29392=CARTESIAN_POINT('Ctrl Pts',(-33.6668018235812,-32.5573852447462,
172.815960405477));
#29393=CARTESIAN_POINT('Ctrl Pts',(-33.6687693399146,-32.005954200378,172.778917142403));
#29394=CARTESIAN_POINT('Ctrl Pts',(-33.6687763776238,-32.0039817586375,
172.778784640472));
#29395=CARTESIAN_POINT('Ctrl Pts',(-33.6687795724397,-32.0020093031855,
172.778652138541));
#29396=CARTESIAN_POINT('Ctrl Pts',(-33.6687789306113,-32.0000368455925,
172.77851963661));
#29397=CARTESIAN_POINT('Ctrl Pts',(-33.6658031255686,-32.0015218482784,
172.97148036339));
#29398=CARTESIAN_POINT('Ctrl Pts',(-33.6670461552837,-32.1386695277898,
172.980650702972));
#29399=CARTESIAN_POINT('Ctrl Pts',(-33.651526531901,-32.2755396643596,172.989821042553));
#29400=CARTESIAN_POINT('Ctrl Pts',(-33.6181580939457,-32.4079104152445,
172.998991382135));
#29401=CARTESIAN_POINT('Ctrl Pts',(-33.4833674665614,-32.9426173914303,
173.036034645208));
#29402=CARTESIAN_POINT('Ctrl Pts',(-33.0573328215213,-33.4039066535968,
173.073077908281));
#29403=CARTESIAN_POINT('Ctrl Pts',(-32.5350053023192,-33.5806947366134,
173.110121171355));
#29404=CARTESIAN_POINT('Ctrl Pts',(-32.0126777831172,-33.75748281963,173.147164434428));
#29405=CARTESIAN_POINT('Ctrl Pts',(-31.3940573897532,-33.6497697234968,
173.184207697501));
#29406=CARTESIAN_POINT('Ctrl Pts',(-30.9622214599011,-33.3068443769544,
173.221250960574));
#29407=CARTESIAN_POINT('Ctrl Pts',(-30.530385530049,-32.9639190304119,173.258294223647));
#29408=CARTESIAN_POINT('Ctrl Pts',(-30.285334063709,-32.3857814334602,173.295337486721));
#29409=CARTESIAN_POINT('Ctrl Pts',(-30.3392012831418,-31.8369842156438,
173.332380749794));
#29410=CARTESIAN_POINT('Ctrl Pts',(-30.3930685025747,-31.2881869978274,
173.369424012867));
#29411=CARTESIAN_POINT('Ctrl Pts',(-30.7458544077805,-30.7687301591463,
173.40646727594));
#29412=CARTESIAN_POINT('Ctrl Pts',(-31.236126081439,-30.5163143323435,173.443510539014));
#29413=CARTESIAN_POINT('Ctrl Pts',(-31.7263977550975,-30.2638985055407,
173.480553802087));
#29414=CARTESIAN_POINT('Ctrl Pts',(-32.3541551972087,-30.2785236906163,
173.51759706516));
#29415=CARTESIAN_POINT('Ctrl Pts',(-32.8321400061355,-30.5534974821813,
173.554640328233));
#29416=CARTESIAN_POINT('Ctrl Pts',(-33.3101248150623,-30.8284712737464,
173.591683591306));
#29417=CARTESIAN_POINT('Ctrl Pts',(-33.6383369908047,-31.363793671801,173.62872685438));
#29418=CARTESIAN_POINT('Ctrl Pts',(-33.6665884213994,-31.9145040496602,
173.665770117453));
#29419=CARTESIAN_POINT('Ctrl Pts',(-33.668040080922,-31.9428015180507,173.667673532765));
#29420=CARTESIAN_POINT('Ctrl Pts',(-33.6686997625326,-31.9711396148911,
173.669576948078));
#29421=CARTESIAN_POINT('Ctrl Pts',(-33.668584334028,-31.9994831966231,173.67148036339));
#29422=CARTESIAN_POINT('Origin',(-32.,-32.,172.));
#29423=CARTESIAN_POINT('',(-33.6642813575761,-31.9988063447756,174.37148036339));
#29424=CARTESIAN_POINT('',(-33.6637114455411,-32.0008167340949,174.17851963661));
#29425=CARTESIAN_POINT('',(-33.666,-32.,172.));
#29426=CARTESIAN_POINT('Ctrl Pts',(-33.6637114455411,-32.0008167340949,
174.17851963661));
#29427=CARTESIAN_POINT('Ctrl Pts',(-33.6622464362393,-31.6705232921065,
174.156504628753));
#29428=CARTESIAN_POINT('Ctrl Pts',(-33.5671323700757,-31.3394521882123,
174.134489620897));
#29429=CARTESIAN_POINT('Ctrl Pts',(-33.3840346023194,-31.0676509334355,
174.11247461304));
#29430=CARTESIAN_POINT('Ctrl Pts',(-33.0759475544607,-30.6103081312015,
174.075431349967));
#29431=CARTESIAN_POINT('Ctrl Pts',(-32.5187551814412,-30.3207740795586,
174.038388086894));
#29432=CARTESIAN_POINT('Ctrl Pts',(-31.9674256919048,-30.3315379906054,
174.00134482382));
#29433=CARTESIAN_POINT('Ctrl Pts',(-31.4160962023684,-30.3423019016522,
173.964301560747));
#29434=CARTESIAN_POINT('Ctrl Pts',(-30.8706295963151,-30.6533637753888,
173.927258297674));
#29435=CARTESIAN_POINT('Ctrl Pts',(-30.5806284350053,-31.1223833850562,
173.890215034601));
#29436=CARTESIAN_POINT('Ctrl Pts',(-30.2906272736955,-31.5914029947235,
173.853171771527));
#29437=CARTESIAN_POINT('Ctrl Pts',(-30.2560915571293,-32.2183803403215,
173.816128508454));
#29438=CARTESIAN_POINT('Ctrl Pts',(-30.4928246419453,-32.7164139881476,
173.779085245381));
#29439=CARTESIAN_POINT('Ctrl Pts',(-30.7295577267612,-33.2144476359738,
173.742041982308));
#29440=CARTESIAN_POINT('Ctrl Pts',(-31.2375596129593,-33.5835375860281,
173.704998719234));
#29441=CARTESIAN_POINT('Ctrl Pts',(-31.7843713919408,-33.6547902784726,
173.667955456161));
#29442=CARTESIAN_POINT('Ctrl Pts',(-32.3311831709223,-33.7260429709171,
173.630912193088));
#29443=CARTESIAN_POINT('Ctrl Pts',(-32.9168048426872,-33.4994584057518,
173.593868930015));
#29444=CARTESIAN_POINT('Ctrl Pts',(-33.2732591056372,-33.0787204513927,
173.556825666941));
#29445=CARTESIAN_POINT('Ctrl Pts',(-33.5244295480755,-32.7822534172426,
173.530723656831));
#29446=CARTESIAN_POINT('Ctrl Pts',(-33.6618157042791,-32.3893869652009,
173.50462164672));
#29447=CARTESIAN_POINT('Ctrl Pts',(-33.665039714177,-31.9985615025105,173.47851963661));
#29448=CARTESIAN_POINT('Ctrl Pts',(-33.668584334028,-31.9994831966231,173.67148036339));
#29449=CARTESIAN_POINT('Ctrl Pts',(-33.6664533539675,-32.5227474262364,
173.706620211151));
#29450=CARTESIAN_POINT('Ctrl Pts',(-33.40014474482,-33.0478810491315,173.741760058912));
#29451=CARTESIAN_POINT('Ctrl Pts',(-32.9757931867974,-33.3537555837251,
173.776899906673));
#29452=CARTESIAN_POINT('Ctrl Pts',(-32.5284558361537,-33.676198382267,173.813943169746));
#29453=CARTESIAN_POINT('Ctrl Pts',(-31.9054904494194,-33.7549856216871,
173.850986432819));
#29454=CARTESIAN_POINT('Ctrl Pts',(-31.3919626096749,-33.5540646884328,
173.888029695892));
#29455=CARTESIAN_POINT('Ctrl Pts',(-30.8784347699304,-33.3531437551784,
173.925072958966));
#29456=CARTESIAN_POINT('Ctrl Pts',(-30.4743444771757,-32.8725146492496,
173.962116222039));
#29457=CARTESIAN_POINT('Ctrl Pts',(-30.364601258287,-32.3321106434165,173.999159485112));
#29458=CARTESIAN_POINT('Ctrl Pts',(-30.2548580393983,-31.7917066375835,
174.036202748186));
#29459=CARTESIAN_POINT('Ctrl Pts',(-30.4394618943756,-31.1915277318462,
174.073246011259));
#29460=CARTESIAN_POINT('Ctrl Pts',(-30.833939100154,-30.8062125391354,174.110289274332));
#29461=CARTESIAN_POINT('Ctrl Pts',(-31.2284163059325,-30.4208973464247,
174.147332537405));
#29462=CARTESIAN_POINT('Ctrl Pts',(-31.832766862512,-30.2504458667405,174.184375800479));
#29463=CARTESIAN_POINT('Ctrl Pts',(-32.3704432321562,-30.3728557729517,
174.221419063552));
#29464=CARTESIAN_POINT('Ctrl Pts',(-32.9081196018005,-30.4952656791629,
174.258462326625));
#29465=CARTESIAN_POINT('Ctrl Pts',(-33.3791217845095,-30.9105369712694,
174.295505589698));
#29466=CARTESIAN_POINT('Ctrl Pts',(-33.5679217353786,-31.4286437577182,
174.332548852771));
#29467=CARTESIAN_POINT('Ctrl Pts',(-33.63406302246,-31.6101493648096,174.345526022978));
#29468=CARTESIAN_POINT('Ctrl Pts',(-33.6655703636659,-31.8042757046356,
174.358503193184));
#29469=CARTESIAN_POINT('Ctrl Pts',(-33.6642813575761,-31.9988063447756,
174.37148036339));
#29470=CARTESIAN_POINT('Origin',(-32.,-32.,172.));
#29471=CARTESIAN_POINT('',(-33.6642763556304,-32.0011913006623,175.07148036339));
#29472=CARTESIAN_POINT('',(-33.6680206995223,-32.0009960691358,174.87851963661));
#29473=CARTESIAN_POINT('',(-33.666,-32.,172.));
#29474=CARTESIAN_POINT('Ctrl Pts',(-33.6680206995223,-32.0009960691358,
174.87851963661));
#29475=CARTESIAN_POINT('Ctrl Pts',(-33.6645339286199,-31.5078337739205,
174.845430873859));
#29476=CARTESIAN_POINT('Ctrl Pts',(-33.4321106122014,-31.0118158279499,
174.812342111109));
#29477=CARTESIAN_POINT('Ctrl Pts',(-33.0490371619582,-30.7021758227049,
174.779253348358));
#29478=CARTESIAN_POINT('Ctrl Pts',(-32.6201818825768,-30.3555301575651,
174.742210085285));
#29479=CARTESIAN_POINT('Ctrl Pts',(-32.0025157577892,-30.2424732431291,
174.705166822212));
#29480=CARTESIAN_POINT('Ctrl Pts',(-31.4786794571432,-30.4147393104172,
174.668123559139));
#29481=CARTESIAN_POINT('Ctrl Pts',(-30.9548431564971,-30.5870053777054,
174.631080296065));
#29482=CARTESIAN_POINT('Ctrl Pts',(-30.5248366799925,-31.0445944267177,
174.594037032992));
#29483=CARTESIAN_POINT('Ctrl Pts',(-30.3854286596648,-31.5781161897994,
174.556993769919));
#29484=CARTESIAN_POINT('Ctrl Pts',(-30.2460206393372,-32.1116379528812,
174.519950506846));
#29485=CARTESIAN_POINT('Ctrl Pts',(-30.3972110751866,-32.7210924300323,
174.482907243773));
#29486=CARTESIAN_POINT('Ctrl Pts',(-30.7698160435642,-33.1275965571378,
174.445863980699));
#29487=CARTESIAN_POINT('Ctrl Pts',(-31.1424210119419,-33.5341006842432,
174.408820717626));
#29488=CARTESIAN_POINT('Ctrl Pts',(-31.7364405128478,-33.7376544613031,
174.371777454553));
#29489=CARTESIAN_POINT('Ctrl Pts',(-32.2800544436041,-33.6451127836591,
174.33473419148));
#29490=CARTESIAN_POINT('Ctrl Pts',(-32.8236683743604,-33.5525711060151,
174.297690928406));
#29491=CARTESIAN_POINT('Ctrl Pts',(-33.3168767349671,-33.1639339736673,
174.260647665333));
#29492=CARTESIAN_POINT('Ctrl Pts',(-33.5339900539215,-32.6570396310809,
174.22360440226));
#29493=CARTESIAN_POINT('Ctrl Pts',(-33.6220717750628,-32.4513952867042,
174.208576147043));
#29494=CARTESIAN_POINT('Ctrl Pts',(-33.6647115148495,-32.226287202919,174.193547891826));
#29495=CARTESIAN_POINT('Ctrl Pts',(-33.6637114455411,-32.0008167340949,
174.17851963661));
#29496=CARTESIAN_POINT('Ctrl Pts',(-33.6642813575761,-31.9988063447756,
174.37148036339));
#29497=CARTESIAN_POINT('Ctrl Pts',(-33.6618909026641,-32.3595623783854,
174.395546456257));
#29498=CARTESIAN_POINT('Ctrl Pts',(-33.5467088752249,-32.7217088616016,
174.419612549124));
#29499=CARTESIAN_POINT('Ctrl Pts',(-33.3304552697857,-33.0073307793206,
174.443678641991));
#29500=CARTESIAN_POINT('Ctrl Pts',(-32.9975911342944,-33.4469687336831,
174.480721905064));
#29501=CARTESIAN_POINT('Ctrl Pts',(-32.4252651442828,-33.7053023616173,
174.517765168138));
#29502=CARTESIAN_POINT('Ctrl Pts',(-31.8753705694715,-33.6641195957362,
174.554808431211));
#29503=CARTESIAN_POINT('Ctrl Pts',(-31.3254759946603,-33.622936829855,174.591851694284));
#29504=CARTESIAN_POINT('Ctrl Pts',(-30.7980128350495,-33.2822376701586,
174.628894957357));
#29505=CARTESIAN_POINT('Ctrl Pts',(-30.5343453724271,-32.7979242047596,
174.665938220431));
#29506=CARTESIAN_POINT('Ctrl Pts',(-30.2706779098048,-32.3136107393606,
174.702981483504));
#29507=CARTESIAN_POINT('Ctrl Pts',(-30.2708061441709,-31.6856829682592,
174.740024746577));
#29508=CARTESIAN_POINT('Ctrl Pts',(-30.5346713961749,-31.2014772347147,
174.77706800965));
#29509=CARTESIAN_POINT('Ctrl Pts',(-30.7985366481788,-30.7172715011702,
174.814111272724));
#29510=CARTESIAN_POINT('Ctrl Pts',(-31.3261389178206,-30.3767878051827,
174.851154535797));
#29511=CARTESIAN_POINT('Ctrl Pts',(-31.8760502673163,-30.3358296398401,
174.88819779887));
#29512=CARTESIAN_POINT('Ctrl Pts',(-32.4259616168121,-30.2948714744975,
174.925241061943));
#29513=CARTESIAN_POINT('Ctrl Pts',(-32.9981820461618,-30.5534388397998,
174.962284325017));
#29514=CARTESIAN_POINT('Ctrl Pts',(-33.330866589631,-30.9932127114078,174.99932758809));
#29515=CARTESIAN_POINT('Ctrl Pts',(-33.5468672972666,-31.2787428610095,
175.02337851319));
#29516=CARTESIAN_POINT('Ctrl Pts',(-33.661892580785,-31.6406599108861,175.04742943829));
#29517=CARTESIAN_POINT('Ctrl Pts',(-33.6642763556304,-32.0011913006623,
175.07148036339));
#29518=CARTESIAN_POINT('Origin',(-32.,-32.,172.));
#29519=CARTESIAN_POINT('',(-33.6685813534211,-32.0005207267373,175.77148036339));
#29520=CARTESIAN_POINT('',(-33.6667310125706,-31.9985486151775,175.57851963661));
#29521=CARTESIAN_POINT('',(-33.666,-32.,172.));
#29522=CARTESIAN_POINT('Ctrl Pts',(-33.6667310125706,-31.9985486151775,
175.57851963661));
#29523=CARTESIAN_POINT('Ctrl Pts',(-33.6677032793229,-31.8922279811891,
175.571400382039));
#29524=CARTESIAN_POINT('Ctrl Pts',(-33.6584013252062,-31.7860768205684,
175.564281127468));
#29525=CARTESIAN_POINT('Ctrl Pts',(-33.6382086695285,-31.6820394404608,
175.557161872897));
#29526=CARTESIAN_POINT('Ctrl Pts',(-33.5331412289776,-31.1407069171911,
175.520118609823));
#29527=CARTESIAN_POINT('Ctrl Pts',(-33.1332209699927,-30.6566024924382,
175.48307534675));
#29528=CARTESIAN_POINT('Ctrl Pts',(-32.6214492346079,-30.4512497260222,
175.446032083677));
#29529=CARTESIAN_POINT('Ctrl Pts',(-32.109677499223,-30.2458969596062,175.408988820604));
#29530=CARTESIAN_POINT('Ctrl Pts',(-31.4860542874383,-30.3192958515271,
175.37194555753));
#29531=CARTESIAN_POINT('Ctrl Pts',(-31.0359461995104,-30.6378594668308,
175.334902294457));
#29532=CARTESIAN_POINT('Ctrl Pts',(-30.5858381115824,-30.9564230821345,
175.297859031384));
#29533=CARTESIAN_POINT('Ctrl Pts',(-30.3092451475112,-31.5201514208209,
175.260815768311));
#29534=CARTESIAN_POINT('Ctrl Pts',(-30.3327347478929,-32.0710854517969,
175.223772505237));
#29535=CARTESIAN_POINT('Ctrl Pts',(-30.3562243482745,-32.6220194827728,
175.186729242164));
#29536=CARTESIAN_POINT('Ctrl Pts',(-30.679796513109,-33.1601592060383,175.149685979091));
#29537=CARTESIAN_POINT('Ctrl Pts',(-31.1553863742651,-33.4392548021681,
175.112642716018));
#29538=CARTESIAN_POINT('Ctrl Pts',(-31.6309762354211,-33.7183503982979,
175.075599452944));
#29539=CARTESIAN_POINT('Ctrl Pts',(-32.2585837928988,-33.7384018672921,
175.038556189871));
#29540=CARTESIAN_POINT('Ctrl Pts',(-32.7510192314565,-33.4902337656634,
175.001512926798));
#29541=CARTESIAN_POINT('Ctrl Pts',(-33.2434546700142,-33.2420656640348,
174.964469663725));
#29542=CARTESIAN_POINT('Ctrl Pts',(-33.600717989652,-32.7256779917834,174.927426400651));
#29543=CARTESIAN_POINT('Ctrl Pts',(-33.6593274324834,-32.1773669477359,
174.890383137578));
#29544=CARTESIAN_POINT('Ctrl Pts',(-33.6655841993383,-32.118832790084,174.886428637255));
#29545=CARTESIAN_POINT('Ctrl Pts',(-33.6684374100764,-32.0599348233683,
174.882474136933));
#29546=CARTESIAN_POINT('Ctrl Pts',(-33.6680206995223,-32.0009960691358,
174.87851963661));
#29547=CARTESIAN_POINT('Ctrl Pts',(-33.6642763556304,-32.0011913006623,
175.07148036339));
#29548=CARTESIAN_POINT('Ctrl Pts',(-33.6655640736003,-32.1959507806569,
175.084472701363));
#29549=CARTESIAN_POINT('Ctrl Pts',(-33.6339810497051,-32.3903059010507,
175.097465039336));
#29550=CARTESIAN_POINT('Ctrl Pts',(-33.5676882417626,-32.5719965913415,
175.11045737731));
#29551=CARTESIAN_POINT('Ctrl Pts',(-33.378676692836,-33.0900262217536,175.147500640383));
#29552=CARTESIAN_POINT('Ctrl Pts',(-32.9075049373938,-33.5051051046639,
175.184543903456));
#29553=CARTESIAN_POINT('Ctrl Pts',(-32.3697786159041,-33.6272953939243,
175.221587166529));
#29554=CARTESIAN_POINT('Ctrl Pts',(-31.8320522944143,-33.7494856831846,
175.258630429603));
#29555=CARTESIAN_POINT('Ctrl Pts',(-31.2277714068769,-33.5787873787949,
175.295673692676));
#29556=CARTESIAN_POINT('Ctrl Pts',(-30.8334516108523,-33.1933110992711,
175.332716955749));
#29557=CARTESIAN_POINT('Ctrl Pts',(-30.4391318148276,-32.8078348197473,
175.369760218822));
#29558=CARTESIAN_POINT('Ctrl Pts',(-30.2547731103158,-32.2075805650895,
175.406803481895));
#29559=CARTESIAN_POINT('Ctrl Pts',(-30.3647370408579,-31.6672214274853,
175.443846744969));
#29560=CARTESIAN_POINT('Ctrl Pts',(-30.4747009714001,-31.1268622898811,
175.480890008042));
#29561=CARTESIAN_POINT('Ctrl Pts',(-30.8789875369963,-30.6463982693306,
175.517933271115));
#29562=CARTESIAN_POINT('Ctrl Pts',(-31.3925973973822,-30.4456870964311,
175.554976534188));
#29563=CARTESIAN_POINT('Ctrl Pts',(-31.906207257768,-30.2449759235315,175.592019797262));
#29564=CARTESIAN_POINT('Ctrl Pts',(-32.5291404129435,-30.324017598283,175.629063060335));
#29565=CARTESIAN_POINT('Ctrl Pts',(-32.9763460288151,-30.6466430789026,
175.666106323408));
#29566=CARTESIAN_POINT('Ctrl Pts',(-33.400389507867,-30.9525588062043,175.701231003402));
#29567=CARTESIAN_POINT('Ctrl Pts',(-33.6664369809567,-31.47747986754,175.736355683396));
#29568=CARTESIAN_POINT('Ctrl Pts',(-33.6685813534211,-32.0005207267373,
175.77148036339));
#29569=CARTESIAN_POINT('Origin',(-32.,-32.,172.));
#29570=CARTESIAN_POINT('',(-33.6658099164955,-31.9984780038309,176.47148036339));
#29571=CARTESIAN_POINT('',(-33.6633199948406,-31.9999190844576,176.27851963661));
#29572=CARTESIAN_POINT('',(-33.666,-32.,172.));
#29573=CARTESIAN_POINT('Ctrl Pts',(-33.6633199948406,-31.9999190844576,
176.27851963661));
#29574=CARTESIAN_POINT('Ctrl Pts',(-33.6634383333563,-31.7268069707849,
176.260326627145));
#29575=CARTESIAN_POINT('Ctrl Pts',(-33.5999313242785,-31.4537466878109,
176.24213361768));
#29576=CARTESIAN_POINT('Ctrl Pts',(-33.4724977567379,-31.2147758799386,
176.223940608215));
#29577=CARTESIAN_POINT('Ctrl Pts',(-33.2130269321966,-30.728201159034,176.186897345142));
#29578=CARTESIAN_POINT('Ctrl Pts',(-32.6885287507801,-30.3829549203862,
176.149854082068));
#29579=CARTESIAN_POINT('Ctrl Pts',(-32.1390107363186,-30.3370199707946,
176.112810818995));
#29580=CARTESIAN_POINT('Ctrl Pts',(-31.5894927218572,-30.2910850212031,
176.075767555922));
#29581=CARTESIAN_POINT('Ctrl Pts',(-31.0149548743507,-30.5444613606678,
176.038724292849));
#29582=CARTESIAN_POINT('Ctrl Pts',(-30.6783025975229,-30.9812053501188,
176.001681029775));
#29583=CARTESIAN_POINT('Ctrl Pts',(-30.3416503206951,-31.4179493395698,
175.964637766702));
#29584=CARTESIAN_POINT('Ctrl Pts',(-30.2428836145458,-32.0380609790071,
175.927594503629));
#29585=CARTESIAN_POINT('Ctrl Pts',(-30.4271975882658,-32.557780544643,175.890551240556));
#29586=CARTESIAN_POINT('Ctrl Pts',(-30.6115115619858,-33.0775001102788,
175.853507977482));
#29587=CARTESIAN_POINT('Ctrl Pts',(-31.0789062155749,-33.4968276021132,
175.816464714409));
#29588=CARTESIAN_POINT('Ctrl Pts',(-31.6155042898944,-33.6238810335897,
175.779421451336));
#29589=CARTESIAN_POINT('Ctrl Pts',(-32.1521023642139,-33.7509344650662,
175.742378188263));
#29590=CARTESIAN_POINT('Ctrl Pts',(-32.7579038592636,-33.5857138361847,
175.705334925189));
#29591=CARTESIAN_POINT('Ctrl Pts',(-33.15569729573,-33.2038232108508,175.668291662116));
#29592=CARTESIAN_POINT('Ctrl Pts',(-33.4770397798243,-32.895327215323,175.638367653614));
#29593=CARTESIAN_POINT('Ctrl Pts',(-33.6626443321084,-32.4454408457679,
175.608443645112));
#29594=CARTESIAN_POINT('Ctrl Pts',(-33.6667310125706,-31.9985486151775,
175.57851963661));
#29595=CARTESIAN_POINT('Ctrl Pts',(-33.6685813534211,-32.0005207267373,
175.77148036339));
#29596=CARTESIAN_POINT('Ctrl Pts',(-33.6686984835053,-32.0290903063712,
175.773398946469));
#29597=CARTESIAN_POINT('Ctrl Pts',(-33.6680282397883,-32.0576542762874,
175.775317529549));
#29598=CARTESIAN_POINT('Ctrl Pts',(-33.6665533627086,-32.0861766390156,
175.777236112628));
#29599=CARTESIAN_POINT('Ctrl Pts',(-33.6380770041629,-32.6368754320213,
175.814279375701));
#29600=CARTESIAN_POINT('Ctrl Pts',(-33.3096462105037,-33.1720637315449,
175.851322638774));
#29601=CARTESIAN_POINT('Ctrl Pts',(-32.8315491320692,-33.4468422736528,
175.888365901848));
#29602=CARTESIAN_POINT('Ctrl Pts',(-32.3534520536346,-33.7216208157607,
175.925409164921));
#29603=CARTESIAN_POINT('Ctrl Pts',(-31.7256886904246,-33.7359896004529,
175.962452427994));
#29604=CARTESIAN_POINT('Ctrl Pts',(-31.2355201535362,-33.4833735497848,
175.999495691067));
#29605=CARTESIAN_POINT('Ctrl Pts',(-30.7453516166478,-33.2307574991166,
176.03653895414));
#29606=CARTESIAN_POINT('Ctrl Pts',(-30.392777906081,-32.7111566130881,176.073582217214));
#29607=CARTESIAN_POINT('Ctrl Pts',(-30.3391348400455,-32.1623374396888,
176.110625480287));
#29608=CARTESIAN_POINT('Ctrl Pts',(-30.2854917740099,-31.6135182662894,
176.14766874336));
#29609=CARTESIAN_POINT('Ctrl Pts',(-30.5307793525056,-31.0354808055192,
176.184712006434));
#29610=CARTESIAN_POINT('Ctrl Pts',(-30.962755309618,-30.6927318652276,176.221755269507));
#29611=CARTESIAN_POINT('Ctrl Pts',(-31.3947312667304,-30.3499829249361,
176.25879853258));
#29612=CARTESIAN_POINT('Ctrl Pts',(-32.0133956024596,-30.2425225051232,
176.295841795653));
#29613=CARTESIAN_POINT('Ctrl Pts',(-32.5356508713666,-30.4195239110553,
176.332885058727));
#29614=CARTESIAN_POINT('Ctrl Pts',(-33.0579061402737,-30.5965253169874,
176.3699283218));
#29615=CARTESIAN_POINT('Ctrl Pts',(-33.4837523423586,-31.0579885486645,
176.406971584873));
#29616=CARTESIAN_POINT('Ctrl Pts',(-33.6183245645552,-31.5927505337774,
176.444014847946));
#29617=CARTESIAN_POINT('Ctrl Pts',(-33.6515838325967,-31.7249159384278,
176.453170019761));
#29618=CARTESIAN_POINT('Ctrl Pts',(-33.6670514510545,-31.8615585907079,
176.462325191576));
#29619=CARTESIAN_POINT('Ctrl Pts',(-33.6658099164955,-31.9984780038309,
176.47148036339));
#29620=CARTESIAN_POINT('Origin',(-32.,-32.,172.));
#29621=CARTESIAN_POINT('',(-33.6634122043807,-32.0004154259855,177.17148036339));
#29622=CARTESIAN_POINT('',(-33.6664340665864,-32.0014938874889,176.97851963661));
#29623=CARTESIAN_POINT('',(-33.666,-32.,172.));
#29624=CARTESIAN_POINT('Ctrl Pts',(-33.6664340665864,-32.0014938874889,
176.97851963661));
#29625=CARTESIAN_POINT('Ctrl Pts',(-33.6623982369357,-31.5642166774555,
176.949252872251));
#29626=CARTESIAN_POINT('Ctrl Pts',(-33.485716464103,-31.1240530442927,176.919986107892));
#29627=CARTESIAN_POINT('Ctrl Pts',(-33.1768207287417,-30.8168180471713,
176.890719343533));
#29628=CARTESIAN_POINT('Ctrl Pts',(-32.7858480251356,-30.427947358081,176.85367608046));
#29629=CARTESIAN_POINT('Ctrl Pts',(-32.1830653647693,-30.2520315499555,
176.816632817387));
#29630=CARTESIAN_POINT('Ctrl Pts',(-31.6443028236447,-30.3695687437297,
176.779589554313));
#29631=CARTESIAN_POINT('Ctrl Pts',(-31.1055402825201,-30.4871059375039,
176.74254629124));
#29632=CARTESIAN_POINT('Ctrl Pts',(-30.6307978606372,-30.8980961331778,
176.705503028167));
#29633=CARTESIAN_POINT('Ctrl Pts',(-30.4373151165222,-31.4144724452213,
176.668459765094));
#29634=CARTESIAN_POINT('Ctrl Pts',(-30.2438323724072,-31.9308487572648,
176.631416502021));
#29635=CARTESIAN_POINT('Ctrl Pts',(-30.3316093060602,-32.5526111856777,
176.594373238947));
#29636=CARTESIAN_POINT('Ctrl Pts',(-30.660479668368,-32.9952446148261,176.557329975874));
#29637=CARTESIAN_POINT('Ctrl Pts',(-30.9893500306758,-33.4378780439745,
176.520286712801));
#29638=CARTESIAN_POINT('Ctrl Pts',(-31.5593138216386,-33.7013824738583,
176.483243449728));
#29639=CARTESIAN_POINT('Ctrl Pts',(-32.1095587011216,-33.6651797060375,
176.446200186654));
#29640=CARTESIAN_POINT('Ctrl Pts',(-32.6598035806047,-33.6289769382167,
176.409156923581));
#29641=CARTESIAN_POINT('Ctrl Pts',(-33.1903295486081,-33.2930669726913,
176.372113660508));
#29642=CARTESIAN_POINT('Ctrl Pts',(-33.4583707987768,-32.8111603883479,
176.335070397434));
#29643=CARTESIAN_POINT('Ctrl Pts',(-33.5947692994478,-32.5659319560578,
176.316220143826));
#29644=CARTESIAN_POINT('Ctrl Pts',(-33.6631973812051,-32.2828976986404,
176.297369890218));
#29645=CARTESIAN_POINT('Ctrl Pts',(-33.6633199948406,-31.9999190844576,
176.27851963661));
#29646=CARTESIAN_POINT('Ctrl Pts',(-33.6658099164955,-31.9984780038309,
176.47148036339));
#29647=CARTESIAN_POINT('Ctrl Pts',(-33.6620280072332,-32.4155560407657,
176.499368454649));
#29648=CARTESIAN_POINT('Ctrl Pts',(-33.5032006501307,-32.8352021617193,
176.527256545907));
#29649=CARTESIAN_POINT('Ctrl Pts',(-33.2199251662155,-33.138687451872,176.555144637166));
#29650=CARTESIAN_POINT('Ctrl Pts',(-32.843655303371,-33.5418016463048,176.592187900239));
#29651=CARTESIAN_POINT('Ctrl Pts',(-32.2478173353736,-33.7399692966219,
176.629231163313));
#29652=CARTESIAN_POINT('Ctrl Pts',(-31.7050634853874,-33.6425099619088,
176.666274426386));
#29653=CARTESIAN_POINT('Ctrl Pts',(-31.1623096354013,-33.5450506271958,
176.703317689459));
#29654=CARTESIAN_POINT('Ctrl Pts',(-30.6726399034262,-33.1519643074527,
176.740360952532));
#29655=CARTESIAN_POINT('Ctrl Pts',(-30.4601245040871,-32.6431251684204,
176.777404215605));
#29656=CARTESIAN_POINT('Ctrl Pts',(-30.247609104748,-32.1342860293882,176.814447478679));
#29657=CARTESIAN_POINT('Ctrl Pts',(-30.3122480380448,-31.5096940710668,
176.851490741752));
#29658=CARTESIAN_POINT('Ctrl Pts',(-30.6244628777836,-31.0551591924778,
176.888534004825));
#29659=CARTESIAN_POINT('Ctrl Pts',(-30.9366777175223,-30.6006243138889,
176.925577267898));
#29660=CARTESIAN_POINT('Ctrl Pts',(-31.4964684637029,-30.3161465150323,
176.962620530972));
#29661=CARTESIAN_POINT('Ctrl Pts',(-32.0476779078561,-30.3319012827413,
176.999663794045));
#29662=CARTESIAN_POINT('Ctrl Pts',(-32.5988873520092,-30.3476560504503,
177.036707057118));
#29663=CARTESIAN_POINT('Ctrl Pts',(-33.1415154941349,-30.6636433847247,
177.073750320191));
#29664=CARTESIAN_POINT('Ctrl Pts',(-33.4272586353279,-31.1352692179958,
177.110793583265));
#29665=CARTESIAN_POINT('Ctrl Pts',(-33.5832998849668,-31.3928190023175,
177.131022509973));
#29666=CARTESIAN_POINT('Ctrl Pts',(-33.6627345752346,-31.6967822785539,
177.151251436682));
#29667=CARTESIAN_POINT('Ctrl Pts',(-33.6634122043807,-32.0004154259855,
177.17148036339));
#29668=CARTESIAN_POINT('Origin',(-32.,-32.,172.));
#29669=CARTESIAN_POINT('',(-33.6673324974466,-32.0013033571361,177.87148036339));
#29670=CARTESIAN_POINT('',(-33.6682333060465,-31.9991447275653,177.67851963661));
#29671=CARTESIAN_POINT('',(-33.666,-32.,172.));
#29672=CARTESIAN_POINT('Ctrl Pts',(-33.6682333060465,-31.9991447275653,
177.67851963661));
#29673=CARTESIAN_POINT('Ctrl Pts',(-33.6685408591694,-31.9500181746268,
177.67522238043));
#29674=CARTESIAN_POINT('Ctrl Pts',(-33.6665588525363,-31.9009167876488,
177.671925124251));
#29675=CARTESIAN_POINT('Ctrl Pts',(-33.6622065197431,-31.8520264135902,
177.668627868071));
#29676=CARTESIAN_POINT('Ctrl Pts',(-33.6133099221287,-31.3027639694832,
177.631584604998));
#29677=CARTESIAN_POINT('Ctrl Pts',(-33.265241148879,-30.7801346509114,177.594541341925));
#29678=CARTESIAN_POINT('Ctrl Pts',(-32.7772747180259,-30.5232906550829,
177.557498078852));
#29679=CARTESIAN_POINT('Ctrl Pts',(-32.2893082871728,-30.2664466592544,
177.520454815778));
#29680=CARTESIAN_POINT('Ctrl Pts',(-31.6614441987163,-30.2753879861691,
177.483411552705));
#29681=CARTESIAN_POINT('Ctrl Pts',(-31.1809895889168,-30.5460232043939,
177.446368289632));
#29682=CARTESIAN_POINT('Ctrl Pts',(-30.7005349791173,-30.8166584226187,
177.409325026559));
#29683=CARTESIAN_POINT('Ctrl Pts',(-30.3674898479748,-31.3489875321536,
177.372281763485));
#29684=CARTESIAN_POINT('Ctrl Pts',(-30.3342538741355,-31.8994195839005,
177.335238500412));
#29685=CARTESIAN_POINT('Ctrl Pts',(-30.3010179002961,-32.4498516356474,
177.298195237339));
#29686=CARTESIAN_POINT('Ctrl Pts',(-30.5675910837598,-33.0183866296063,
177.261151974266));
#29687=CARTESIAN_POINT('Ctrl Pts',(-31.0119909652455,-33.3448660524889,
177.224108711192));
#29688=CARTESIAN_POINT('Ctrl Pts',(-31.4563908467312,-33.6713454753716,
177.187065448119));
#29689=CARTESIAN_POINT('Ctrl Pts',(-32.0786174262389,-33.755769327178,177.150022185046));
#29690=CARTESIAN_POINT('Ctrl Pts',(-32.5939432027082,-33.5595057026458,
177.112978921973));
#29691=CARTESIAN_POINT('Ctrl Pts',(-33.1092689791776,-33.3632420781135,
177.075935658899));
#29692=CARTESIAN_POINT('Ctrl Pts',(-33.5176939526085,-32.8862909772425,
177.038892395826));
#29693=CARTESIAN_POINT('Ctrl Pts',(-33.6323250659011,-32.3469026417795,
177.001849132753));
#29694=CARTESIAN_POINT('Ctrl Pts',(-33.656389595621,-32.2336687539068,176.994072634039));
#29695=CARTESIAN_POINT('Ctrl Pts',(-33.6675064305726,-32.1176832147392,
176.986296135324));
#29696=CARTESIAN_POINT('Ctrl Pts',(-33.6664340665864,-32.0014938874889,
176.97851963661));
#29697=CARTESIAN_POINT('Ctrl Pts',(-33.6634122043807,-32.0004154259855,
177.17148036339));
#29698=CARTESIAN_POINT('Ctrl Pts',(-33.663975451485,-32.2527960859167,177.188294699755));
#29699=CARTESIAN_POINT('Ctrl Pts',(-33.6101256220151,-32.5049486605984,
177.20510903612));
#29700=CARTESIAN_POINT('Ctrl Pts',(-33.5006277344169,-32.7300294102653,
177.221923372484));
#29701=CARTESIAN_POINT('Ctrl Pts',(-33.259395552053,-33.2258994369961,177.258966635558));
#29702=CARTESIAN_POINT('Ctrl Pts',(-32.7480730470649,-33.5903751581898,
177.296009898631));
#29703=CARTESIAN_POINT('Ctrl Pts',(-32.200638611329,-33.6566745563935,177.333053161704));
#29704=CARTESIAN_POINT('Ctrl Pts',(-31.653204175593,-33.7229739545973,177.370096424777));
#29705=CARTESIAN_POINT('Ctrl Pts',(-31.0696578091092,-33.491097029811,177.407139687851));
#29706=CARTESIAN_POINT('Ctrl Pts',(-30.717027193283,-33.0671492094921,177.444182950924));
#29707=CARTESIAN_POINT('Ctrl Pts',(-30.3643965774567,-32.6432013891732,
177.481226213997));
#29708=CARTESIAN_POINT('Ctrl Pts',(-30.2426817122881,-32.0271826733217,
177.51826947707));
#29709=CARTESIAN_POINT('Ctrl Pts',(-30.4075786025872,-31.5009802852002,
177.555312740144));
#29710=CARTESIAN_POINT('Ctrl Pts',(-30.5724754928864,-30.9747778970788,
177.592356003217));
#29711=CARTESIAN_POINT('Ctrl Pts',(-31.0239841386533,-30.5383918366873,
177.62939926629));
#29712=CARTESIAN_POINT('Ctrl Pts',(-31.5554967489003,-30.3915091864542,
177.666442529363));
#29713=CARTESIAN_POINT('Ctrl Pts',(-32.0870093591472,-30.2446265362211,
177.703485792436));
#29714=CARTESIAN_POINT('Ctrl Pts',(-32.6985259338742,-30.3872472961464,
177.74052905551));
#29715=CARTESIAN_POINT('Ctrl Pts',(-33.1102195658544,-30.7541106342973,
177.777572318583));
#29716=CARTESIAN_POINT('Ctrl Pts',(-33.4581131802515,-31.0641212897578,
177.808875000185));
#29717=CARTESIAN_POINT('Ctrl Pts',(-33.6633179681641,-31.5342582545151,
177.840177681788));
#29718=CARTESIAN_POINT('Ctrl Pts',(-33.6673324974466,-32.0013033571361,
177.87148036339));
#29719=CARTESIAN_POINT('Origin',(-32.,-32.,172.));
#29720=CARTESIAN_POINT('',(-33.6674973899495,-31.9987820730806,178.57148036339));
#29721=CARTESIAN_POINT('',(-33.6638666881858,-31.9990537019747,178.37851963661));
#29722=CARTESIAN_POINT('',(-33.666,-32.,172.));
#29723=CARTESIAN_POINT('',(-30.7309291201475,-30.9206413469517,179.));
#29724=CARTESIAN_POINT('Ctrl Pts',(-33.6674973899495,-31.9987820730806,
178.57148036339));
#29725=CARTESIAN_POINT('Ctrl Pts',(-33.6635707056189,-32.4716839165788,
178.60319045304));
#29726=CARTESIAN_POINT('Ctrl Pts',(-33.452366876924,-32.9475799899327,178.634900542691));
#29727=CARTESIAN_POINT('Ctrl Pts',(-33.0965045258218,-33.2578609118632,
178.666610632341));
#29728=CARTESIAN_POINT('Ctrl Pts',(-32.6807913305846,-33.6203265480209,
178.703653895414));
#29729=CARTESIAN_POINT('Ctrl Pts',(-32.067668858848,-33.756784295561,178.740697158487));
#29730=CARTESIAN_POINT('Ctrl Pts',(-31.5378405565417,-33.6037851722251,
178.777740421561));
#29731=CARTESIAN_POINT('Ctrl Pts',(-31.0080122542353,-33.4507860488891,
178.814783684634));
#29732=CARTESIAN_POINT('Ctrl Pts',(-30.5614781213592,-33.0083300546771,
178.851826947707));
#29733=CARTESIAN_POINT('Ctrl Pts',(-30.4024857707402,-32.4812852538864,
178.88887021078));
#29734=CARTESIAN_POINT('Ctrl Pts',(-30.2434934201212,-31.9542404530957,
178.925913473853));
#29735=CARTESIAN_POINT('Ctrl Pts',(-30.3720428517593,-31.3426068457263,
178.962956736927));
#29736=CARTESIAN_POINT('Ctrl Pts',(-30.7309291201476,-30.9206413469516,
179.));
#29737=CARTESIAN_POINT('',(-33.2714881524743,-30.9188041220687,179.));
#29738=CARTESIAN_POINT('Origin',(-32.,-32.,179.));
#29739=CARTESIAN_POINT('Ctrl Pts',(-33.2714899711315,-30.918802739816,179.));
#29740=CARTESIAN_POINT('Ctrl Pts',(-32.9207087468888,-30.5073974083421,
178.963685183163));
#29741=CARTESIAN_POINT('Ctrl Pts',(-32.3509045024841,-30.2812938695396,
178.927370366326));
#29742=CARTESIAN_POINT('Ctrl Pts',(-31.8135987861801,-30.3417506510624,
178.891055549488));
#29743=CARTESIAN_POINT('Ctrl Pts',(-31.2655151461327,-30.4034201473605,
178.854012286415));
#29744=CARTESIAN_POINT('Ctrl Pts',(-30.7512468997307,-30.7632616102458,
178.816969023342));
#29745=CARTESIAN_POINT('Ctrl Pts',(-30.5057843626736,-31.2569767104513,
178.779925760269));
#29746=CARTESIAN_POINT('Ctrl Pts',(-30.2603218256164,-31.7506918106568,
178.742882497195));
#29747=CARTESIAN_POINT('Ctrl Pts',(-30.283664997904,-32.3782805481824,178.705839234122));
#29748=CARTESIAN_POINT('Ctrl Pts',(-30.5652971229397,-32.8523839798957,
178.668795971049));
#29749=CARTESIAN_POINT('Ctrl Pts',(-30.8469292479753,-33.326487411609,178.631752707976));
#29750=CARTESIAN_POINT('Ctrl Pts',(-31.386850325759,-33.64710553751,178.594709444902));
#29751=CARTESIAN_POINT('Ctrl Pts',(-31.9379143916448,-33.6676125145974,
178.557666181829));
#29752=CARTESIAN_POINT('Ctrl Pts',(-32.4889784575306,-33.6881194916849,
178.520622918756));
#29753=CARTESIAN_POINT('Ctrl Pts',(-33.0511855115185,-33.4085153199588,
178.483579655683));
#29754=CARTESIAN_POINT('Ctrl Pts',(-33.3673124400932,-32.9567024906769,
178.446536392609));
#29755=CARTESIAN_POINT('Ctrl Pts',(-33.5607972682093,-32.6801713896778,
178.42386414061));
#29756=CARTESIAN_POINT('Ctrl Pts',(-33.6620998285923,-32.3391304687567,
178.40119188861));
#29757=CARTESIAN_POINT('Ctrl Pts',(-33.6638666881858,-31.9990537019747,
178.37851963661));
#29758=CARTESIAN_POINT('Origin',(-32.,-32.,180.545925280538));
#29759=CARTESIAN_POINT('',(-34.0533144768684,-31.9981861022711,166.254074719462));
#29760=CARTESIAN_POINT('',(-34.054669363007,-32.0018603689044,166.195925280538));
#29761=CARTESIAN_POINT('',(-34.05475,-31.9999999999998,180.545925280538));
#29762=CARTESIAN_POINT('',(-31.6163320011535,-29.981387499008,166.));
#29763=CARTESIAN_POINT('Ctrl Pts',(-34.0546693630069,-32.0018603689044,
166.195925280538));
#29764=CARTESIAN_POINT('Ctrl Pts',(-34.0494207835165,-31.4804652280817,
166.167660116765));
#29765=CARTESIAN_POINT('Ctrl Pts',(-33.5818273573597,-30.2681449287862,
166.102351689919));
#29766=CARTESIAN_POINT('Ctrl Pts',(-32.2875197530252,-29.8538180613451,
166.037043263073));
#29767=CARTESIAN_POINT('Ctrl Pts',(-31.6163320011535,-29.981387499008,166.));
#29768=CARTESIAN_POINT('',(-30.6584058382614,-30.4387497520534,166.));
#29769=CARTESIAN_POINT('Origin',(-32.,-32.,166.));
#29770=CARTESIAN_POINT('Ctrl Pts',(-34.0533144768684,-31.9981861022711,
166.254074719462));
#29771=CARTESIAN_POINT('Ctrl Pts',(-34.0549811944317,-31.7888335083511,
166.242741226219));
#29772=CARTESIAN_POINT('Ctrl Pts',(-33.9292854405696,-30.897222765403,166.194364469902));
#29773=CARTESIAN_POINT('Ctrl Pts',(-32.6547058314541,-29.6692718705854,
166.109672896748));
#29774=CARTESIAN_POINT('Ctrl Pts',(-31.1647193012354,-30.0048405258246,
166.036314816837));
#29775=CARTESIAN_POINT('Ctrl Pts',(-30.658403887814,-30.438747719014,166.));
#29776=CARTESIAN_POINT('Origin',(-32.,-32.,180.545925280538));
#29777=CARTESIAN_POINT('',(-34.052039769042,-32.0011058419296,166.954074719462));
#29778=CARTESIAN_POINT('',(-34.0578396464241,-31.9992413474394,166.895925280538));
#29779=CARTESIAN_POINT('',(-34.05475,-31.9999999999998,180.545925280538));
#29780=CARTESIAN_POINT('Ctrl Pts',(-34.0578396464241,-31.9992413474394,
166.895925280538));
#29781=CARTESIAN_POINT('Ctrl Pts',(-34.0580399301433,-31.9570745650302,
166.893629624944));
#29782=CARTESIAN_POINT('Ctrl Pts',(-34.0377496442503,-31.2346904324969,
166.854290706278));
#29783=CARTESIAN_POINT('Ctrl Pts',(-33.1886966470223,-29.8821785627325,
166.777908524538));
#29784=CARTESIAN_POINT('Ctrl Pts',(-30.8656448278897,-29.8526443561693,
166.666778735318));
#29785=CARTESIAN_POINT('Ctrl Pts',(-29.580472364777,-31.7882407548095,166.555648946099));
#29786=CARTESIAN_POINT('Ctrl Pts',(-30.5101755007489,-33.9178527489701,
166.444519156879));
#29787=CARTESIAN_POINT('Ctrl Pts',(-32.8022294941794,-34.2918270332952,
166.333389367659));
#29788=CARTESIAN_POINT('Ctrl Pts',(-33.9655640455529,-33.0073758803891,
166.250524742212));
#29789=CARTESIAN_POINT('Ctrl Pts',(-34.0562993748591,-32.1637861358238,
166.204703379838));
#29790=CARTESIAN_POINT('Ctrl Pts',(-34.0546693630069,-32.0018603689044,
166.195925280538));
#29791=CARTESIAN_POINT('Ctrl Pts',(-34.052039769042,-32.0011058419296,166.954074719462));
#29792=CARTESIAN_POINT('Ctrl Pts',(-34.0500129149945,-31.5865390425708,
166.931667471325));
#29793=CARTESIAN_POINT('Ctrl Pts',(-33.7267813695385,-30.483712125216,166.872216960114));
#29794=CARTESIAN_POINT('Ctrl Pts',(-31.9269554466752,-29.5724870533531,
166.77572318583));
#29795=CARTESIAN_POINT('Ctrl Pts',(-29.9209653227032,-30.7446538702704,
166.66459339661));
#29796=CARTESIAN_POINT('Ctrl Pts',(-29.8177242538605,-33.0657579476906,
166.553463607391));
#29797=CARTESIAN_POINT('Ctrl Pts',(-31.7115987445193,-34.4113736221389,
166.442333818171));
#29798=CARTESIAN_POINT('Ctrl Pts',(-33.6494969998368,-33.6381762860152,
166.342537522195));
#29799=CARTESIAN_POINT('Ctrl Pts',(-34.0495335662521,-32.4730976663593,
166.279784489292));
#29800=CARTESIAN_POINT('Ctrl Pts',(-34.0533144768684,-31.9981861022711,
166.254074719462));
#29801=CARTESIAN_POINT('Origin',(-32.,-32.,180.545925280538));
#29802=CARTESIAN_POINT('',(-34.0574026221756,-32.0011268610995,167.654074719462));
#29803=CARTESIAN_POINT('',(-34.052475201976,-31.9986057389706,167.595925280538));
#29804=CARTESIAN_POINT('',(-34.05475,-31.9999999999998,180.545925280538));
#29805=CARTESIAN_POINT('Ctrl Pts',(-34.052475201976,-31.9986057389706,167.595925280538));
#29806=CARTESIAN_POINT('Ctrl Pts',(-34.0540189352112,-31.7513839339351,
167.58255587005));
#29807=CARTESIAN_POINT('Ctrl Pts',(-33.8982418403506,-30.8210528024315,
167.53214319649));
#29808=CARTESIAN_POINT('Ctrl Pts',(-32.514074117309,-29.6264115999403,167.444687259856));
#29809=CARTESIAN_POINT('Ctrl Pts',(-30.2847464274524,-30.2806705307475,
167.333557470637));
#29810=CARTESIAN_POINT('Ctrl Pts',(-29.6251964131156,-32.5084396585803,
167.222427681417));
#29811=CARTESIAN_POINT('Ctrl Pts',(-31.139048610325,-34.2708933540495,167.111297892197));
#29812=CARTESIAN_POINT('Ctrl Pts',(-33.3932698151157,-33.9615685478801,
167.002463758571));
#29813=CARTESIAN_POINT('Ctrl Pts',(-34.0548081028085,-32.6374881332951,
166.930672888018));
#29814=CARTESIAN_POINT('Ctrl Pts',(-34.0578396464241,-31.9992413474394,
166.895925280538));
#29815=CARTESIAN_POINT('Ctrl Pts',(-34.0574026221756,-32.0011268610995,
167.654074719462));
#29816=CARTESIAN_POINT('Ctrl Pts',(-34.0533392918178,-31.3858045207831,
167.620593716431));
#29817=CARTESIAN_POINT('Ctrl Pts',(-33.4332619034794,-30.0825878835663,
167.550069450326));
#29818=CARTESIAN_POINT('Ctrl Pts',(-31.2169834359616,-29.7010702107005,
167.442501921148));
#29819=CARTESIAN_POINT('Ctrl Pts',(-29.643917581989,-31.4108732197425,167.331372131929));
#29820=CARTESIAN_POINT('Ctrl Pts',(-30.2271133546761,-33.6598394847521,
167.220242342709));
#29821=CARTESIAN_POINT('Ctrl Pts',(-32.4328346425493,-34.389736993149,167.109112553489));
#29822=CARTESIAN_POINT('Ctrl Pts',(-33.8775609679021,-33.2263857218232,
167.020390012407));
#29823=CARTESIAN_POINT('Ctrl Pts',(-34.0533636739647,-32.2718934830552,
166.968710734398));
#29824=CARTESIAN_POINT('Ctrl Pts',(-34.052039769042,-32.0011058419296,166.954074719462));
#29825=CARTESIAN_POINT('Origin',(-32.,-32.,180.545925280538));
#29826=CARTESIAN_POINT('',(-34.0554335040134,-31.998175874568,168.354074719462));
#29827=CARTESIAN_POINT('',(-34.0527878691605,-32.0015414751871,168.295925280538));
#29828=CARTESIAN_POINT('',(-34.05475,-31.9999999999998,180.545925280538));
#29829=CARTESIAN_POINT('Ctrl Pts',(-34.0527878691605,-32.0015414751871,
168.295925280538));
#29830=CARTESIAN_POINT('Ctrl Pts',(-34.0496367929324,-31.5497213201872,
168.271482115157));
#29831=CARTESIAN_POINT('Ctrl Pts',(-33.6800738627717,-30.4084888310145,
168.209995686702));
#29832=CARTESIAN_POINT('Ctrl Pts',(-31.7940424351662,-29.5801291028184,
168.111465995175));
#29833=CARTESIAN_POINT('Ctrl Pts',(-29.8553131533993,-30.8604773304489,
168.000336205955));
#29834=CARTESIAN_POINT('Ctrl Pts',(-29.8793779622368,-33.1837043267573,
167.889206416735));
#29835=CARTESIAN_POINT('Ctrl Pts',(-31.8442131712534,-34.4236180024818,
167.778076627516));
#29836=CARTESIAN_POINT('Ctrl Pts',(-33.6980918025173,-33.5631391374147,
167.680316248783));
#29837=CARTESIAN_POINT('Ctrl Pts',(-34.0497416399332,-32.4363731763679,
167.619599133124));
#29838=CARTESIAN_POINT('Ctrl Pts',(-34.052475201976,-31.9986057389706,167.595925280538));
#29839=CARTESIAN_POINT('Ctrl Pts',(-34.0554335040134,-31.998175874568,168.354074719462));
#29840=CARTESIAN_POINT('Ctrl Pts',(-34.0567078789638,-31.8597835387434,
168.34656322461));
#29841=CARTESIAN_POINT('Ctrl Pts',(-33.9808807164526,-31.0402919719527,
168.302008466685));
#29842=CARTESIAN_POINT('Ctrl Pts',(-32.8805549549265,-29.7366359735545,
168.220410445687));
#29843=CARTESIAN_POINT('Ctrl Pts',(-30.576127479021,-30.0325700070413,168.109280656467));
#29844=CARTESIAN_POINT('Ctrl Pts',(-29.5748126892805,-32.1290746285719,
167.998150867247));
#29845=CARTESIAN_POINT('Ctrl Pts',(-30.7930030339464,-34.1074515612365,
167.887021078027));
#29846=CARTESIAN_POINT('Ctrl Pts',(-33.1158238969359,-34.1571116561114,
167.775891288808));
#29847=CARTESIAN_POINT('Ctrl Pts',(-34.0253015915237,-32.8124183710368,
167.698242502619));
#29848=CARTESIAN_POINT('Ctrl Pts',(-34.0578349461223,-32.0665949769654,
167.657636979504));
#29849=CARTESIAN_POINT('Ctrl Pts',(-34.0574026221756,-32.0011268610995,
167.654074719462));
#29850=CARTESIAN_POINT('Origin',(-32.,-32.,180.545925280538));
#29851=CARTESIAN_POINT('',(-34.0514404014557,-32.0000193281895,169.054074719462));
#29852=CARTESIAN_POINT('',(-34.0580205885241,-32.0005154407378,168.995925280538));
#29853=CARTESIAN_POINT('',(-34.05475,-31.9999999999998,180.545925280538));
#29854=CARTESIAN_POINT('Ctrl Pts',(-34.0580205885241,-32.0005154407378,
168.995925280538));
#29855=CARTESIAN_POINT('Ctrl Pts',(-34.0558244730528,-31.3482962555674,
168.960408360263));
#29856=CARTESIAN_POINT('Ctrl Pts',(-33.3683227356013,-30.0118438106801,
168.887848176915));
#29857=CARTESIAN_POINT('Ctrl Pts',(-31.0921885500407,-29.7474299050867,
168.778244730493));
#29858=CARTESIAN_POINT('Ctrl Pts',(-29.6151760063164,-31.540861481794,168.667114941273));
#29859=CARTESIAN_POINT('Ctrl Pts',(-30.3207285185246,-33.7544916509204,
168.555985152054));
#29860=CARTESIAN_POINT('Ctrl Pts',(-32.56313208116,-34.3624300883911,168.444855362834));
#29861=CARTESIAN_POINT('Ctrl Pts',(-33.9103001430262,-33.150131804933,168.358168738995));
#29862=CARTESIAN_POINT('Ctrl Pts',(-34.0544122033125,-32.2344482204289,
168.30852537823));
#29863=CARTESIAN_POINT('Ctrl Pts',(-34.0527878691605,-32.0015414751871,
168.295925280538));
#29864=CARTESIAN_POINT('Ctrl Pts',(-34.0514404014557,-32.0000193281895,
169.054074719462));
#29865=CARTESIAN_POINT('Ctrl Pts',(-34.051411527961,-31.6559142783085,169.035489469716));
#29866=CARTESIAN_POINT('Ctrl Pts',(-33.8062204612892,-30.6259162375257,
168.979860956897));
#29867=CARTESIAN_POINT('Ctrl Pts',(-32.1767327344769,-29.5778193124972,
168.887189181005));
#29868=CARTESIAN_POINT('Ctrl Pts',(-30.0609459319521,-30.5377199094004,
168.776059391785));
#29869=CARTESIAN_POINT('Ctrl Pts',(-29.719760384286,-32.8358833873742,168.664929602565));
#29870=CARTESIAN_POINT('Ctrl Pts',(-31.4654254048604,-34.3690554541617,
168.553799813346));
#29871=CARTESIAN_POINT('Ctrl Pts',(-33.5492656048371,-33.7770120558115,
168.450181518978));
#29872=CARTESIAN_POINT('Ctrl Pts',(-34.0504232435519,-32.5422713529885,
168.383606487683));
#29873=CARTESIAN_POINT('Ctrl Pts',(-34.0554335040134,-31.998175874568,168.354074719462));
#29874=CARTESIAN_POINT('Origin',(-32.,-32.,180.545925280538));
#29875=CARTESIAN_POINT('',(-34.0555044381159,-32.0018139756141,169.754074719462));
#29876=CARTESIAN_POINT('',(-34.0543002253323,-31.9981314623868,169.695925280538));
#29877=CARTESIAN_POINT('',(-34.05475,-31.9999999999998,180.545925280538));
#29878=CARTESIAN_POINT('Ctrl Pts',(-34.0543002253323,-31.9981314623868,
169.695925280538));
#29879=CARTESIAN_POINT('Ctrl Pts',(-34.0558755988635,-31.8219808306189,
169.686377868442));
#29880=CARTESIAN_POINT('Ctrl Pts',(-33.9545116868703,-30.9641640659178,
169.639787193273));
#29881=CARTESIAN_POINT('Ctrl Pts',(-32.7552096240695,-29.6917859534862,
169.556153255031));
#29882=CARTESIAN_POINT('Ctrl Pts',(-30.4704602313883,-30.1135478386525,
169.445023465812));
#29883=CARTESIAN_POINT('Ctrl Pts',(-29.5855290477775,-32.2617702841642,
169.333893676592));
#29884=CARTESIAN_POINT('Ctrl Pts',(-30.9102954957832,-34.1704234043853,
169.222763887372));
#29885=CARTESIAN_POINT('Ctrl Pts',(-33.2323476887161,-34.0927285621829,
169.111634098152));
#29886=CARTESIAN_POINT('Ctrl Pts',(-34.0448973480045,-32.7367311286634,
169.036021229207));
#29887=CARTESIAN_POINT('Ctrl Pts',(-34.0581149667812,-32.0285446180569,
168.997451623336));
#29888=CARTESIAN_POINT('Ctrl Pts',(-34.0580205885241,-32.0005154407378,
168.995925280538));
#29889=CARTESIAN_POINT('Ctrl Pts',(-34.0555044381159,-32.001813975614,169.754074719462));
#29890=CARTESIAN_POINT('Ctrl Pts',(-34.0504819825047,-31.4554228012545,
169.724415714823));
#29891=CARTESIAN_POINT('Ctrl Pts',(-33.545729393308,-30.2184084874635,169.657713447109));
#29892=CARTESIAN_POINT('Ctrl Pts',(-31.4573116667505,-29.6327900145418,
169.553967916323));
#29893=CARTESIAN_POINT('Ctrl Pts',(-29.7169098581211,-31.1719340929902,
169.442838127103));
#29894=CARTESIAN_POINT('Ctrl Pts',(-30.065967388257,-33.4689151095322,169.331708337884));
#29895=CARTESIAN_POINT('Ctrl Pts',(-32.1850305909512,-34.4215609475536,
169.220578548664));
#29896=CARTESIAN_POINT('Ctrl Pts',(-33.8086854466956,-33.3693338832287,
169.12803400919));
#29897=CARTESIAN_POINT('Ctrl Pts',(-34.0514690772797,-32.3417686015944,
169.07253273279));
#29898=CARTESIAN_POINT('Ctrl Pts',(-34.0514404014557,-32.0000193281895,
169.054074719462));
#29899=CARTESIAN_POINT('Origin',(-32.,-32.,180.545925280538));
#29900=CARTESIAN_POINT('',(-34.0573518213482,-31.9988395038175,170.454074719462));
#29901=CARTESIAN_POINT('',(-34.0516184490435,-32.0006260637404,170.395925280538));
#29902=CARTESIAN_POINT('',(-34.05475,-31.9999999999998,180.545925280538));
#29903=CARTESIAN_POINT('Ctrl Pts',(-34.0516184490435,-32.0006260637404,
170.395925280538));
#29904=CARTESIAN_POINT('Ctrl Pts',(-34.0505756737721,-31.61890879556,170.375304113548));
#29905=CARTESIAN_POINT('Ctrl Pts',(-33.7652193718894,-30.5500373359834,
170.317639683485));
#29906=CARTESIAN_POINT('Ctrl Pts',(-32.0437423823724,-29.5717742558001,
170.22293199035));
#29907=CARTESIAN_POINT('Ctrl Pts',(-29.983732689712,-30.6461684764067,170.11180220113));
#29908=CARTESIAN_POINT('Ctrl Pts',(-29.7689889739188,-32.9595746257144,
170.00067241191));
#29909=CARTESIAN_POINT('Ctrl Pts',(-31.5960423548879,-34.3947884837217,
169.88954262269));
#29910=CARTESIAN_POINT('Ctrl Pts',(-33.6040655308435,-33.7033079951078,
169.787960245566));
#29911=CARTESIAN_POINT('Ctrl Pts',(-34.0497632643824,-32.5054324432433,
169.723421131515));
#29912=CARTESIAN_POINT('Ctrl Pts',(-34.0543002253323,-31.9981314623868,
169.695925280538));
#29913=CARTESIAN_POINT('Ctrl Pts',(-34.0573518213482,-31.9988395038175,
170.454074719462));
#29914=CARTESIAN_POINT('Ctrl Pts',(-34.0578102452832,-31.9310285956751,
170.450385223002));
#29915=CARTESIAN_POINT('Ctrl Pts',(-34.024004004144,-31.1828456234217,170.409652463468));
#29916=CARTESIAN_POINT('Ctrl Pts',(-33.1084266441611,-29.8390779475391,
170.331876440861));
#29917=CARTESIAN_POINT('Ctrl Pts',(-30.7857895475778,-29.8966962369818,
170.220746651642));
#29918=CARTESIAN_POINT('Ctrl Pts',(-29.5743846894872,-31.8792353209593,
170.109616862422));
#29919=CARTESIAN_POINT('Ctrl Pts',(-30.5828766588753,-33.9722969295563,
169.998487073202));
#29920=CARTESIAN_POINT('Ctrl Pts',(-32.888304541998,-34.2603337768931,169.887357283982));
#29921=CARTESIAN_POINT('Ctrl Pts',(-33.9824484770852,-32.9549541539966,
169.805886499403));
#29922=CARTESIAN_POINT('Ctrl Pts',(-34.0567548883806,-32.1378500188405,
169.761458977896));
#29923=CARTESIAN_POINT('Ctrl Pts',(-34.0555044381159,-32.001813975614,169.754074719462));
#29924=CARTESIAN_POINT('Origin',(-32.,-32.,180.545925280538));
#29925=CARTESIAN_POINT('',(-34.0520023712765,-31.9989253081128,171.154074719462));
#29926=CARTESIAN_POINT('',(-34.0565936768906,-32.0015359661287,171.095925280538));
#29927=CARTESIAN_POINT('',(-34.05475,-31.9999999999998,180.545925280538));
#29928=CARTESIAN_POINT('Ctrl Pts',(-34.0565936768906,-32.0015359661287,
171.095925280538));
#29929=CARTESIAN_POINT('Ctrl Pts',(-34.0517293936845,-31.4184384269289,
171.064230358654));
#29930=CARTESIAN_POINT('Ctrl Pts',(-33.4873352665121,-30.145615302178,170.995492173698));
#29931=CARTESIAN_POINT('Ctrl Pts',(-31.3284143351364,-29.6660834728807,
170.889710725668));
#29932=CARTESIAN_POINT('Ctrl Pts',(-29.6749656425999,-31.298281468308,170.778580936448));
#29933=CARTESIAN_POINT('Ctrl Pts',(-30.1493631800083,-33.5726846541191,
170.667451147229));
#29934=CARTESIAN_POINT('Ctrl Pts',(-32.3174434657525,-34.4077838995354,
170.556321358009));
#29935=CARTESIAN_POINT('Ctrl Pts',(-33.8466042950419,-33.2932393514889,
170.465812735779));
#29936=CARTESIAN_POINT('Ctrl Pts',(-34.0524488848626,-32.3046145653666,
170.412347376621));
#29937=CARTESIAN_POINT('Ctrl Pts',(-34.0516184490435,-32.0006260637404,
170.395925280538));
#29938=CARTESIAN_POINT('Ctrl Pts',(-34.0520023712765,-31.9989253081128,
171.154074719462));
#29939=CARTESIAN_POINT('Ctrl Pts',(-34.0532978946503,-31.7257714041052,
171.139311468108));
#29940=CARTESIAN_POINT('Ctrl Pts',(-33.8754247784623,-30.7688511478335,
171.08750495368));
#29941=CARTESIAN_POINT('Ctrl Pts',(-32.4246449932043,-29.6087931139184,
170.99865517618));
#29942=CARTESIAN_POINT('Ctrl Pts',(-30.2214364984569,-30.3462449959935,
170.88752538696));
#29943=CARTESIAN_POINT('Ctrl Pts',(-29.6459500326037,-32.5971955235092,
170.77639559774));
#29944=CARTESIAN_POINT('Ctrl Pts',(-31.2248645683027,-34.3015991842251,
170.66526580852));
#29945=CARTESIAN_POINT('Ctrl Pts',(-33.4372030087975,-33.91295041841,170.557825515761));
#29946=CARTESIAN_POINT('Ctrl Pts',(-34.0532075796883,-32.611863321091,170.487428486075));
#29947=CARTESIAN_POINT('Ctrl Pts',(-34.0573518213482,-31.9988395038175,
170.454074719462));
#29948=CARTESIAN_POINT('Origin',(-32.,-32.,180.545925280538));
#29949=CARTESIAN_POINT('',(-34.0534332149094,-32.0017453824621,171.854074719462));
#29950=CARTESIAN_POINT('',(-34.0564014860358,-31.998396538586,171.795925280538));
#29951=CARTESIAN_POINT('',(-34.05475,-31.9999999999998,180.545925280538));
#29952=CARTESIAN_POINT('Ctrl Pts',(-34.0564014860358,-31.998396538586,171.795925280538));
#29953=CARTESIAN_POINT('Ctrl Pts',(-34.0573061420266,-31.8930393954218,
171.790199866834));
#29954=CARTESIAN_POINT('Ctrl Pts',(-34.0020448666022,-31.1069760699122,
171.747431190056));
#29955=CARTESIAN_POINT('Ctrl Pts',(-32.9883523238082,-29.7815876522084,
171.667619250206));
#29956=CARTESIAN_POINT('Ctrl Pts',(-30.6723620180839,-29.9663896514365,
171.556489460986));
#29957=CARTESIAN_POINT('Ctrl Pts',(-29.5714115957749,-32.0123297880839,
171.445359671767));
#29958=CARTESIAN_POINT('Ctrl Pts',(-30.6930789440682,-34.046985836388,171.334229882547));
#29959=CARTESIAN_POINT('Ctrl Pts',(-33.0108262697815,-34.2082626458667,
171.223100093327));
#29960=CARTESIAN_POINT('Ctrl Pts',(-34.006283703558,-32.8789600308985,171.143665225991));
#29961=CARTESIAN_POINT('Ctrl Pts',(-34.0574144975358,-32.0999304218123,
171.101273621728));
#29962=CARTESIAN_POINT('Ctrl Pts',(-34.0565936768906,-32.0015359661287,
171.095925280538));
#29963=CARTESIAN_POINT('Ctrl Pts',(-34.0534332149094,-32.0017453824621,
171.854074719462));
#29964=CARTESIAN_POINT('Ctrl Pts',(-34.04957930023,-31.524539330965,171.828237713214));
#29965=CARTESIAN_POINT('Ctrl Pts',(-33.6462715310717,-30.357274746545,171.765357443893));
#29966=CARTESIAN_POINT('Ctrl Pts',(-31.7033831764878,-29.5895618235874,
171.665433911498));
#29967=CARTESIAN_POINT('Ctrl Pts',(-29.8140636467216,-30.9417580608795,
171.554304122278));
#29968=CARTESIAN_POINT('Ctrl Pts',(-29.925289361983,-33.2624458446987,171.443174333059));
#29969=CARTESIAN_POINT('Ctrl Pts',(-31.9352677538577,-34.4277568821048,
171.332044543839));
#29970=CARTESIAN_POINT('Ctrl Pts',(-33.729598785223,-33.5115700062286,171.235678005974));
#29971=CARTESIAN_POINT('Ctrl Pts',(-34.0500472277068,-32.4111564648077,
171.176354731181));
#29972=CARTESIAN_POINT('Ctrl Pts',(-34.0520023712765,-31.9989253081128,
171.154074719462));
#29973=CARTESIAN_POINT('Origin',(-32.,-32.,180.545925280538));
#29974=CARTESIAN_POINT('',(-34.0581778610564,-32.0000454497033,172.554074719462));
#29975=CARTESIAN_POINT('',(-34.0515604600302,-31.9994832149161,172.495925280538));
#29976=CARTESIAN_POINT('',(-34.05475,-31.9999999999998,180.545925280538));
#29977=CARTESIAN_POINT('Ctrl Pts',(-34.0515604600302,-31.9994832149161,
172.495925280538));
#29978=CARTESIAN_POINT('Ctrl Pts',(-34.0522605628883,-31.6884927994845,
172.47912611194));
#29979=CARTESIAN_POINT('Ctrl Pts',(-33.8397955875772,-30.6926560482339,
172.425283680269));
#29980=CARTESIAN_POINT('Ctrl Pts',(-32.2929794020452,-29.5891170225852,
172.334397985524));
#29981=CARTESIAN_POINT('Ctrl Pts',(-30.1334901515899,-30.4461870619026,
172.223268196305));
#29982=CARTESIAN_POINT('Ctrl Pts',(-29.6822104729431,-32.7252898517669,
172.112138407085));
#29983=CARTESIAN_POINT('Ctrl Pts',(-31.352146634078,-34.3406152347352,172.001008617865));
#29984=CARTESIAN_POINT('Ctrl Pts',(-33.4984092777462,-33.8409746916955,
171.895604242349));
#29985=CARTESIAN_POINT('Ctrl Pts',(-34.0514530436148,-32.5746971013405,
171.827243129907));
#29986=CARTESIAN_POINT('Ctrl Pts',(-34.0564014860358,-31.998396538586,171.795925280538));
#29987=CARTESIAN_POINT('Ctrl Pts',(-34.0581773755543,-32.000045443266,172.554074719462));
#29988=CARTESIAN_POINT('Ctrl Pts',(-34.0579568627806,-31.3223688901445,
172.51716395832));
#29989=CARTESIAN_POINT('Ctrl Pts',(-33.3218062651671,-29.9641725193915,
172.443209934105));
#29990=CARTESIAN_POINT('Ctrl Pts',(-31.0083014581836,-29.7830814754581,
172.332212646816));
#29991=CARTESIAN_POINT('Ctrl Pts',(-29.5996266783055,-31.6306740480343,
172.221082857597));
#29992=CARTESIAN_POINT('Ctrl Pts',(-30.3877475314776,-33.8162697266764,
172.109953068377));
#29993=CARTESIAN_POINT('Ctrl Pts',(-32.6513843596913,-34.3396350480892,
171.998823279157));
#29994=CARTESIAN_POINT('Ctrl Pts',(-33.9311983000411,-33.0979305633151,
171.913530496186));
#29995=CARTESIAN_POINT('Ctrl Pts',(-34.0551047691624,-32.2087234479617,
171.865280976287));
#29996=CARTESIAN_POINT('Ctrl Pts',(-34.0534332149094,-32.0017453824621,
171.854074719462));
#29997=CARTESIAN_POINT('Origin',(-32.,-32.,180.545925280538));
#29998=CARTESIAN_POINT('',(-34.0535656378783,-31.9982258387056,173.254074719462));
#29999=CARTESIAN_POINT('',(-34.0545071862317,-32.0018769614345,173.195925280538));
#30000=CARTESIAN_POINT('',(-34.05475,-31.9999999999998,180.545925280538));
#30001=CARTESIAN_POINT('Ctrl Pts',(-34.0545071862317,-32.0018769614345,
173.195925280538));
#30002=CARTESIAN_POINT('Ctrl Pts',(-34.0498474363346,-31.4877509693236,
173.168052357046));
#30003=CARTESIAN_POINT('Ctrl Pts',(-33.5941675512997,-30.2829837046594,
173.103136170481));
#30004=CARTESIAN_POINT('Ctrl Pts',(-31.571747429243,-29.6094365943462,173.001176720843));
#30005=CARTESIAN_POINT('Ctrl Pts',(-29.7593608338838,-31.063127656467,172.890046931623));
#30006=CARTESIAN_POINT('Ctrl Pts',(-29.9975829046342,-33.3742341274316,
172.778917142403));
#30007=CARTESIAN_POINT('Ctrl Pts',(-32.0683953857542,-34.4276564279194,
172.667787353184));
#30008=CARTESIAN_POINT('Ctrl Pts',(-33.7730366841982,-33.4359288520185,
172.573456732562));
#30009=CARTESIAN_POINT('Ctrl Pts',(-34.0507167903975,-32.374246960769,172.516169375013));
#30010=CARTESIAN_POINT('Ctrl Pts',(-34.0515604600302,-31.9994832149161,
172.495925280538));
#30011=CARTESIAN_POINT('Ctrl Pts',(-34.0535656378783,-31.9982258387056,
173.254074719462));
#30012=CARTESIAN_POINT('Ctrl Pts',(-34.0552323993927,-31.7961753299681,
173.2431334665));
#30013=CARTESIAN_POINT('Ctrl Pts',(-33.9350351652449,-30.9119920786341,
173.195148950464));
#30014=CARTESIAN_POINT('Ctrl Pts',(-32.6680632857967,-29.6650727659158,
173.110121171355));
#30015=CARTESIAN_POINT('Ctrl Pts',(-30.4007493854086,-30.1722715699463,
172.998991382135));
#30016=CARTESIAN_POINT('Ctrl Pts',(-29.5970523043438,-32.3521876122724,
172.887861592915));
#30017=CARTESIAN_POINT('Ctrl Pts',(-30.9925068954609,-34.2097853711626,
172.776731803695));
#30018=CARTESIAN_POINT('Ctrl Pts',(-33.3100082500444,-34.0450115224891,
172.665602014476));
#30019=CARTESIAN_POINT('Ctrl Pts',(-34.0570726447537,-32.685019407829,172.591382986398));
#30020=CARTESIAN_POINT('Ctrl Pts',(-34.0581781671492,-32.0024781606965,
172.554207221393));
#30021=CARTESIAN_POINT('Ctrl Pts',(-34.0581773755543,-32.000045443266,172.554074719462));
#30022=CARTESIAN_POINT('Origin',(-32.,-32.,180.545925280538));
#30023=CARTESIAN_POINT('',(-34.051927426606,-32.0010073135544,173.954074719462));
#30024=CARTESIAN_POINT('',(-34.0579373711549,-31.9993626039982,173.895925280538));
#30025=CARTESIAN_POINT('',(-34.05475,-31.9999999999998,180.545925280538));
#30026=CARTESIAN_POINT('Ctrl Pts',(-34.0579373711549,-31.9993626039982,
173.895925280538));
#30027=CARTESIAN_POINT('Ctrl Pts',(-34.058079734132,-31.9644052363129,173.894021865225));
#30028=CARTESIAN_POINT('Ctrl Pts',(-34.0414319960198,-31.2492644665138,
173.85507518684));
#30029=CARTESIAN_POINT('Ctrl Pts',(-33.2110354115502,-29.8948665380118,
173.779085245381));
#30030=CARTESIAN_POINT('Ctrl Pts',(-30.8883140354794,-29.8407529143012,
173.667955456161));
#30031=CARTESIAN_POINT('Ctrl Pts',(-29.5829955984056,-31.7627588073625,
173.556825666941));
#30032=CARTESIAN_POINT('Ctrl Pts',(-30.4896933783496,-33.9018852671521,
173.445695877722));
#30033=CARTESIAN_POINT('Ctrl Pts',(-32.7786073998349,-34.3004269555309,
173.334566088502));
#30034=CARTESIAN_POINT('Ctrl Pts',(-33.9595797532929,-33.0217284461304,
173.251309222774));
#30035=CARTESIAN_POINT('Ctrl Pts',(-34.056040268649,-32.1710271381908,173.205095620119));
#30036=CARTESIAN_POINT('Ctrl Pts',(-34.0545071862317,-32.0018769614345,
173.195925280538));
#30037=CARTESIAN_POINT('Ctrl Pts',(-34.051927426606,-32.0010073135544,173.954074719462));
#30038=CARTESIAN_POINT('Ctrl Pts',(-34.0501205671445,-31.5936420975126,
173.932059711606));
#30039=CARTESIAN_POINT('Ctrl Pts',(-33.7354250014453,-30.4982561832208,
173.873001440676));
#30040=CARTESIAN_POINT('Ctrl Pts',(-31.9525937458611,-29.571843005618,173.776899906673));
#30041=CARTESIAN_POINT('Ctrl Pts',(-29.9343509329174,-30.722781274034,173.665770117453));
#30042=CARTESIAN_POINT('Ctrl Pts',(-29.8065677451363,-33.0426162695937,
173.554640328234));
#30043=CARTESIAN_POINT('Ctrl Pts',(-31.6861899702242,-34.4082601619239,
173.443510539014));
#30044=CARTESIAN_POINT('Ctrl Pts',(-33.6396742821775,-33.6524319289162,
173.343322002757));
#30045=CARTESIAN_POINT('Ctrl Pts',(-34.0495893267512,-32.4802478191756,
173.280176729573));
#30046=CARTESIAN_POINT('Ctrl Pts',(-34.0535656378783,-31.9982258387056,
173.254074719462));
#30047=CARTESIAN_POINT('Origin',(-32.,-32.,180.545925280538));
#30048=CARTESIAN_POINT('',(-34.0572422162926,-32.0012284952321,174.654074719462));
#30049=CARTESIAN_POINT('',(-34.0526303238172,-31.9985278132817,174.595925280538));
#30050=CARTESIAN_POINT('',(-34.05475,-31.9999999999998,180.545925280538));
#30051=CARTESIAN_POINT('Ctrl Pts',(-34.0526303238172,-31.9985278132817,
174.595925280538));
#30052=CARTESIAN_POINT('Ctrl Pts',(-34.0542201108898,-31.7586047443576,
174.582948110331));
#30053=CARTESIAN_POINT('Ctrl Pts',(-33.9044368791735,-30.8357445655057,
174.532927677052));
#30054=CARTESIAN_POINT('Ctrl Pts',(-32.5391158564695,-29.6319738696303,
174.445863980699));
#30055=CARTESIAN_POINT('Ctrl Pts',(-30.3030006593535,-30.2626494600523,
174.334734191479));
#30056=CARTESIAN_POINT('Ctrl Pts',(-29.6199608556057,-32.4833294238526,
174.22360440226));
#30057=CARTESIAN_POINT('Ctrl Pts',(-31.1151070663578,-34.2616715404322,
174.11247461304));
#30058=CARTESIAN_POINT('Ctrl Pts',(-33.3806181402508,-33.9751494202814,
174.003248239133));
#30059=CARTESIAN_POINT('Ctrl Pts',(-34.0553091410954,-32.6447270552576,
173.931065128299));
#30060=CARTESIAN_POINT('Ctrl Pts',(-34.0579373711549,-31.9993626039982,
173.895925280538));
#30061=CARTESIAN_POINT('Ctrl Pts',(-34.0572422162926,-32.0012284952321,
174.654074719462));
#30062=CARTESIAN_POINT('Ctrl Pts',(-34.0529418306313,-31.3929900642036,
174.620985956712));
#30063=CARTESIAN_POINT('Ctrl Pts',(-33.4453673259805,-30.0963565660462,
174.550853930888));
#30064=CARTESIAN_POINT('Ctrl Pts',(-31.2413083934035,-29.6929280920661,
174.443678641991));
#30065=CARTESIAN_POINT('Ctrl Pts',(-29.65027152498,-31.3860213065764,174.332548852771));
#30066=CARTESIAN_POINT('Ctrl Pts',(-30.2096806751507,-33.6410211629863,
174.221419063552));
#30067=CARTESIAN_POINT('Ctrl Pts',(-32.4075706562188,-34.3941762471646,
174.110289274332));
#30068=CARTESIAN_POINT('Ctrl Pts',(-33.8709432996413,-33.2410714072619,
174.021174492969));
#30069=CARTESIAN_POINT('Ctrl Pts',(-34.0531608554243,-32.2790898140443,
173.969102974679));
#30070=CARTESIAN_POINT('Ctrl Pts',(-34.051927426606,-32.0010073135544,173.954074719462));
#30071=CARTESIAN_POINT('Origin',(-32.,-32.,180.545925280538));
#30072=CARTESIAN_POINT('',(-34.0556515894835,-31.9982099441992,175.354074719462));
#30073=CARTESIAN_POINT('',(-34.0526241547008,-32.0014692827344,175.295925280538));
#30074=CARTESIAN_POINT('',(-34.05475,-31.9999999999998,180.545925280538));
#30075=CARTESIAN_POINT('Ctrl Pts',(-34.0526241547008,-32.0014692827344,
175.295925280538));
#30076=CARTESIAN_POINT('Ctrl Pts',(-34.0496841418774,-31.5568102952538,
175.271874355438));
#30077=CARTESIAN_POINT('Ctrl Pts',(-33.6893168078909,-30.4229458230359,
175.210780167264));
#30078=CARTESIAN_POINT('Ctrl Pts',(-31.8196126680302,-29.5780887565239,
175.112642716018));
#30079=CARTESIAN_POINT('Ctrl Pts',(-29.8674684359538,-30.837888650276,175.001512926798));
#30080=CARTESIAN_POINT('Ctrl Pts',(-29.8669939649505,-33.1612402487227,
174.890383137578));
#30081=CARTESIAN_POINT('Ctrl Pts',(-31.8186234857374,-34.4218373646645,
174.779253348358));
#30082=CARTESIAN_POINT('Ctrl Pts',(-33.6889615682118,-33.5776135643453,
174.681100729345));
#30083=CARTESIAN_POINT('Ctrl Pts',(-34.0496820721784,-32.4434638637377,
174.619991373405));
#30084=CARTESIAN_POINT('Ctrl Pts',(-34.0526303238172,-31.9985278132817,
174.595925280538));
#30085=CARTESIAN_POINT('Ctrl Pts',(-34.0556515894835,-31.9982099441992,
175.354074719462));
#30086=CARTESIAN_POINT('Ctrl Pts',(-34.0568507282045,-31.8670800986484,
175.346955464891));
#30087=CARTESIAN_POINT('Ctrl Pts',(-33.9856839203566,-31.0549454486666,
175.302792947247));
#30088=CARTESIAN_POINT('Ctrl Pts',(-32.9044115461845,-29.7460626678129,
175.221587166529));
#30089=CARTESIAN_POINT('Ctrl Pts',(-30.5969869463981,-30.0176407707682,
175.110457377309));
#30090=CARTESIAN_POINT('Ctrl Pts',(-29.5735846782254,-32.1034525425256,
174.99932758809));
#30091=CARTESIAN_POINT('Ctrl Pts',(-30.7708113991622,-34.0945856692598,
174.88819779887));
#30092=CARTESIAN_POINT('Ctrl Pts',(-33.0929781975906,-34.168776706323,174.77706800965));
#30093=CARTESIAN_POINT('Ctrl Pts',(-34.0212735122584,-32.8270205551761,
174.699026983181));
#30094=CARTESIAN_POINT('Ctrl Pts',(-34.057756163478,-32.0739202150757,174.658029219785));
#30095=CARTESIAN_POINT('Ctrl Pts',(-34.0572422162926,-32.0012284952321,
174.654074719462));
#30096=CARTESIAN_POINT('Origin',(-32.,-32.,180.545925280538));
#30097=CARTESIAN_POINT('',(-34.0514446334927,-31.9999002033549,176.054074719462));
#30098=CARTESIAN_POINT('',(-34.0579336950432,-32.0006422348519,175.995925280538));
#30099=CARTESIAN_POINT('',(-34.05475,-31.9999999999998,180.545925280538));
#30100=CARTESIAN_POINT('Ctrl Pts',(-34.0579336950432,-32.0006422348519,
175.995925280538));
#30101=CARTESIAN_POINT('Ctrl Pts',(-34.0552889475514,-31.355553276007,175.960800600544));
#30102=CARTESIAN_POINT('Ctrl Pts',(-33.3811101636429,-30.0253747230238,
175.888632657477));
#30103=CARTESIAN_POINT('Ctrl Pts',(-31.116030889737,-29.7379672254987,175.779421451336));
#30104=CARTESIAN_POINT('Ctrl Pts',(-29.6201584635808,-31.5156985212241,
175.668291662116));
#30105=CARTESIAN_POINT('Ctrl Pts',(-30.302291203249,-33.7366572782917,175.557161872896));
#30106=CARTESIAN_POINT('Ctrl Pts',(-32.5381486228183,-34.368246127532,175.446032083677));
#30107=CARTESIAN_POINT('Ctrl Pts',(-33.9041991402115,-33.1648235619611,
175.358953219557));
#30108=CARTESIAN_POINT('Ctrl Pts',(-34.0542123530794,-32.2416745897686,
175.308917618511));
#30109=CARTESIAN_POINT('Ctrl Pts',(-34.0526241547008,-32.0014692827344,
175.295925280538));
#30110=CARTESIAN_POINT('Ctrl Pts',(-34.0514446334927,-31.9999002033549,
176.054074719462));
#30111=CARTESIAN_POINT('Ctrl Pts',(-34.0515905855125,-31.6630591976112,
176.035881709997));
#30112=CARTESIAN_POINT('Ctrl Pts',(-33.8137831278114,-30.6405614822225,
175.980645437459));
#30113=CARTESIAN_POINT('Ctrl Pts',(-32.2023060098439,-29.5798210767118,
175.888365901848));
#30114=CARTESIAN_POINT('Ctrl Pts',(-30.0764987310374,-30.5173211370632,
175.777236112628));
#30115=CARTESIAN_POINT('Ctrl Pts',(-29.7110589540984,-32.8117528137747,
175.666106323408));
#30116=CARTESIAN_POINT('Ctrl Pts',(-31.4404331998289,-34.3632771184206,
175.554976534188));
#30117=CARTESIAN_POINT('Ctrl Pts',(-33.5383218130657,-33.7911186162802,
175.45096599954));
#30118=CARTESIAN_POINT('Ctrl Pts',(-34.0506113093635,-32.5493814993046,
175.383998727964));
#30119=CARTESIAN_POINT('Ctrl Pts',(-34.0556515894835,-31.9982099441992,
175.354074719462));
#30120=CARTESIAN_POINT('Origin',(-32.,-32.,180.545925280538));
#30121=CARTESIAN_POINT('',(-34.0552853531323,-32.0018424761811,176.754074719462));
#30122=CARTESIAN_POINT('',(-34.0545155617762,-31.9981228561659,176.695925280538));
#30123=CARTESIAN_POINT('',(-34.05475,-31.9999999999998,180.545925280538));
#30124=CARTESIAN_POINT('Ctrl Pts',(-34.0545155617762,-31.9981228561659,
176.695925280538));
#30125=CARTESIAN_POINT('Ctrl Pts',(-34.0560468001527,-31.8292542102386,
176.686770108723));
#30126=CARTESIAN_POINT('Ctrl Pts',(-33.9597818464189,-30.9788389613939,
176.640571673835));
#30127=CARTESIAN_POINT('Ctrl Pts',(-32.7795469135615,-29.6998912483741,
176.557329975874));
#30128=CARTESIAN_POINT('Ctrl Pts',(-30.4904703040065,-30.0974980267845,
176.446200186654));
#30129=CARTESIAN_POINT('Ctrl Pts',(-29.5828989020006,-32.2362539796973,
176.335070397435));
#30130=CARTESIAN_POINT('Ctrl Pts',(-30.8874322125415,-34.1587928522671,
176.223940608215));
#30131=CARTESIAN_POINT('Ctrl Pts',(-33.2101754968556,-34.1056279176698,
176.112810818995));
#30132=CARTESIAN_POINT('Ctrl Pts',(-34.0412910572988,-32.7512989933157,
176.036805709769));
#30133=CARTESIAN_POINT('Ctrl Pts',(-34.0580781566522,-32.0358783355439,
175.997843863617));
#30134=CARTESIAN_POINT('Ctrl Pts',(-34.0579336950432,-32.0006422348519,
175.995925280538));
#30135=CARTESIAN_POINT('Ctrl Pts',(-34.0552853531323,-32.0018424761811,
176.754074719462));
#30136=CARTESIAN_POINT('Ctrl Pts',(-34.050307789522,-31.4625295426181,176.724807955103));
#30137=CARTESIAN_POINT('Ctrl Pts',(-33.5565883388568,-30.232536523623,176.658497927671));
#30138=CARTESIAN_POINT('Ctrl Pts',(-31.4823444699111,-29.6271901683823,
176.555144637166));
#30139=CARTESIAN_POINT('Ctrl Pts',(-29.7257832609726,-31.1478662270158,
176.444014847946));
#30140=CARTESIAN_POINT('Ctrl Pts',(-30.0505605498502,-33.4484058724806,
176.332885058726));
#30141=CARTESIAN_POINT('Ctrl Pts',(-32.1594436821683,-34.4233801713471,
176.221755269507));
#30142=CARTESIAN_POINT('Ctrl Pts',(-33.8010500299471,-33.3839740631711,
176.128818489752));
#30143=CARTESIAN_POINT('Ctrl Pts',(-34.0512934087822,-32.3489099917655,
176.072924973071));
#30144=CARTESIAN_POINT('Ctrl Pts',(-34.0514446334927,-31.9999002033549,
176.054074719462));
#30145=CARTESIAN_POINT('Origin',(-32.,-32.,180.545925280538));
#30146=CARTESIAN_POINT('',(-34.0575044331327,-31.9989451554411,177.454074719462));
#30147=CARTESIAN_POINT('',(-34.0515583595145,-32.0005123628719,177.395925280538));
#30148=CARTESIAN_POINT('',(-34.05475,-31.9999999999998,180.545925280538));
#30149=CARTESIAN_POINT('Ctrl Pts',(-34.0515583595145,-32.0005123628719,
177.395925280538));
#30150=CARTESIAN_POINT('Ctrl Pts',(-34.0507226101221,-31.6260284434929,
177.375696353829));
#30151=CARTESIAN_POINT('Ctrl Pts',(-33.773348995474,-30.5646358407676,177.318424164047));
#30152=CARTESIAN_POINT('Ctrl Pts',(-32.0693869216736,-29.5723717254276,
177.224108711192));
#30153=CARTESIAN_POINT('Ctrl Pts',(-29.9981443603627,-30.6249481189457,
177.112978921973));
#30154=CARTESIAN_POINT('Ctrl Pts',(-29.7589783672204,-32.9359571099918,
177.001849132753));
#30155=CARTESIAN_POINT('Ctrl Pts',(-31.5707710714985,-34.3903882903498,
176.890719343533));
#30156=CARTESIAN_POINT('Ctrl Pts',(-33.5937670274845,-33.7175671934565,
176.788744726128));
#30157=CARTESIAN_POINT('Ctrl Pts',(-34.049851169185,-32.5125232741679,176.723813371796));
#30158=CARTESIAN_POINT('Ctrl Pts',(-34.0545155617762,-31.9981228561659,
176.695925280538));
#30159=CARTESIAN_POINT('Ctrl Pts',(-34.0575044331327,-31.9989451554411,
177.454074719462));
#30160=CARTESIAN_POINT('Ctrl Pts',(-34.0578837517277,-31.9383552486882,
177.450777463283));
#30161=CARTESIAN_POINT('Ctrl Pts',(-34.0279764047848,-31.1974433913819,
177.41043694403));
#30162=CARTESIAN_POINT('Ctrl Pts',(-33.1311884386701,-29.8509058112995,
177.333053161704));
#30163=CARTESIAN_POINT('Ctrl Pts',(-30.8080724679209,-29.8839889892312,
177.221923372484));
#30164=CARTESIAN_POINT('Ctrl Pts',(-29.5757954873418,-31.853622670774,177.110793583265));
#30165=CARTESIAN_POINT('Ctrl Pts',(-30.562124266553,-33.9572192112968,176.999663794045));
#30166=CARTESIAN_POINT('Ctrl Pts',(-32.8643812849987,-34.2695899967097,
176.888534004825));
#30167=CARTESIAN_POINT('Ctrl Pts',(-33.9775854780963,-32.9696108085324,
176.806670979964));
#30168=CARTESIAN_POINT('Ctrl Pts',(-34.0566079461098,-32.1451438088147,
176.761851218177));
#30169=CARTESIAN_POINT('Ctrl Pts',(-34.0552853531323,-32.0018424761811,
176.754074719462));
#30170=CARTESIAN_POINT('Origin',(-32.,-32.,180.545925280538));
#30171=CARTESIAN_POINT('',(-34.0521188940875,-31.9988328896354,178.154074719462));
#30172=CARTESIAN_POINT('',(-34.0563934268478,-32.0016074868405,178.095925280538));
#30173=CARTESIAN_POINT('',(-34.05475,-31.9999999999998,180.545925280538));
#30174=CARTESIAN_POINT('Ctrl Pts',(-34.0563934268478,-32.0016074868405,
178.095925280538));
#30175=CARTESIAN_POINT('Ctrl Pts',(-34.0514421339048,-31.4255805212877,
178.064622598935));
#30176=CARTESIAN_POINT('Ctrl Pts',(-33.4988525573121,-30.1595633443075,
177.99627665426));
#30177=CARTESIAN_POINT('Ctrl Pts',(-31.3531025202806,-29.6591214698943,
177.890887446511));
#30178=CARTESIAN_POINT('Ctrl Pts',(-29.6825069802633,-31.2737629901632,
177.779757657291));
#30179=CARTESIAN_POINT('Ctrl Pts',(-30.1328556342944,-33.5530507267704,
177.668627868071));
#30180=CARTESIAN_POINT('Ctrl Pts',(-32.2919947036809,-34.4110023075711,
177.557498078851));
#30181=CARTESIAN_POINT('Ctrl Pts',(-33.839519683589,-33.3079112493542,177.46659721634));
#30182=CARTESIAN_POINT('Ctrl Pts',(-34.0522530365779,-32.31178436827,177.412739616902));
#30183=CARTESIAN_POINT('Ctrl Pts',(-34.0515583595145,-32.0005123628719,
177.395925280538));
#30184=CARTESIAN_POINT('Ctrl Pts',(-34.0521188940875,-31.9988328896354,
178.154074719462));
#30185=CARTESIAN_POINT('Ctrl Pts',(-34.053500164455,-31.7329725109556,178.139703708389));
#30186=CARTESIAN_POINT('Ctrl Pts',(-33.881982536996,-30.7835296150249,178.088289434242));
#30187=CARTESIAN_POINT('Ctrl Pts',(-32.4498708176529,-29.6134185829238,
177.999831897022));
#30188=CARTESIAN_POINT('Ctrl Pts',(-30.23900588914,-30.3275485827783,177.888702107803));
#30189=CARTESIAN_POINT('Ctrl Pts',(-29.6397721844782,-32.5723003600472,
177.777572318583));
#30190=CARTESIAN_POINT('Ctrl Pts',(-31.2005990238776,-34.293282975036,177.666442529363));
#30191=CARTESIAN_POINT('Ctrl Pts',(-33.42500915292,-33.9266903753032,177.558609996323));
#30192=CARTESIAN_POINT('Ctrl Pts',(-34.0536222695325,-32.619056939197,177.487820726356));
#30193=CARTESIAN_POINT('Ctrl Pts',(-34.0575044331327,-31.9989451554411,
177.454074719462));
#30194=CARTESIAN_POINT('Origin',(-32.,-32.,180.545925280538));
#30195=CARTESIAN_POINT('',(-34.0526600126176,-32.0021813586275,178.854074719462));
#30196=CARTESIAN_POINT('',(-34.0565967959177,-31.9984978779484,178.795925280538));
#30197=CARTESIAN_POINT('',(-34.05475,-31.9999999999998,180.545925280538));
#30198=CARTESIAN_POINT('',(-32.5301702171889,-33.9851743256717,179.));
#30199=CARTESIAN_POINT('Ctrl Pts',(-32.5301702171889,-33.9851743256717,
179.));
#30200=CARTESIAN_POINT('Ctrl Pts',(-33.190239790753,-33.8088929660697,178.962956736927));
#30201=CARTESIAN_POINT('Ctrl Pts',(-33.9248822331584,-33.1125975988824,
178.914314976748));
#30202=CARTESIAN_POINT('Ctrl Pts',(-34.0542719683944,-32.2164508334355,
178.865673216568));
#30203=CARTESIAN_POINT('Ctrl Pts',(-34.0526600126176,-32.0021813586275,
178.854074719462));
#30204=CARTESIAN_POINT('',(-31.4686665305884,-33.9887337536768,179.));
#30205=CARTESIAN_POINT('Origin',(-32.,-32.,179.));
#30206=CARTESIAN_POINT('Ctrl Pts',(-31.4686656554569,-33.9887364314853,
179.));
#30207=CARTESIAN_POINT('Ctrl Pts',(-32.1131053683168,-34.1599912916281,
178.963685183163));
#30208=CARTESIAN_POINT('Ctrl Pts',(-33.4929540196752,-33.8408666928276,
178.895660276675));
#30209=CARTESIAN_POINT('Ctrl Pts',(-34.0517538459607,-32.5817482158403,
178.827635370188));
#30210=CARTESIAN_POINT('Ctrl Pts',(-34.0565967959177,-31.9984978779484,
178.795925280538));
#30211=CARTESIAN_POINT('Origin',(32.,32.,172.));
#30212=CARTESIAN_POINT('',(30.3314948391898,32.0006151205084,166.67148036339));
#30213=CARTESIAN_POINT('',(30.3351639991694,32.0014707476285,166.47851963661));
#30214=CARTESIAN_POINT('',(30.334,32.,172.));
#30215=CARTESIAN_POINT('',(32.6750771856741,30.4769022377462,166.));
#30216=CARTESIAN_POINT('Ctrl Pts',(30.3351639991694,32.0014707476285,166.47851963661));
#30217=CARTESIAN_POINT('Ctrl Pts',(30.3338126182148,32.1712147141657,166.467186143366));
#30218=CARTESIAN_POINT('Ctrl Pts',(30.3576887331272,32.3405776321984,166.455852650123));
#30219=CARTESIAN_POINT('Ctrl Pts',(30.4083704059759,32.5014768155649,166.444519156879));
#30220=CARTESIAN_POINT('Ctrl Pts',(30.574022292818,33.0273721110032,166.407475893806));
#30221=CARTESIAN_POINT('Ctrl Pts',(31.0260364143234,33.4628498154943,166.370432630732));
#30222=CARTESIAN_POINT('Ctrl Pts',(31.557848973733,33.6090488989997,166.333389367659));
#30223=CARTESIAN_POINT('Ctrl Pts',(32.0896615331426,33.755247982505,166.296346104586));
#30224=CARTESIAN_POINT('Ctrl Pts',(32.7012725304564,33.6121684450247,166.259302841513));
#30225=CARTESIAN_POINT('Ctrl Pts',(33.11224753475,33.2444370308748,166.222259578439));
#30226=CARTESIAN_POINT('Ctrl Pts',(33.5232225390436,32.876705616725,166.185216315366));
#30227=CARTESIAN_POINT('Ctrl Pts',(33.7335615503171,32.2843223259056,166.148173052293));
#30228=CARTESIAN_POINT('Ctrl Pts',(33.6481325428054,31.7404871965806,166.11112978922));
#30229=CARTESIAN_POINT('Ctrl Pts',(33.5627035352937,31.1966520672555,166.074086526147));
#30230=CARTESIAN_POINT('Ctrl Pts',(33.1815065089967,30.7013650994246,166.037043263073));
#30231=CARTESIAN_POINT('Ctrl Pts',(32.6750771856741,30.4769022377462,166.));
#30232=CARTESIAN_POINT('',(30.334,32.,166.));
#30233=CARTESIAN_POINT('Origin',(32.,32.,166.));
#30234=CARTESIAN_POINT('',(30.334,32.,165.));
#30235=CARTESIAN_POINT('',(30.334,32.,172.));
#30236=CARTESIAN_POINT('Origin',(32.,32.,165.));
#30237=CARTESIAN_POINT('',(30.3853154136487,31.5775542237606,166.));
#30238=CARTESIAN_POINT('Origin',(32.,32.,166.));
#30239=CARTESIAN_POINT('Ctrl Pts',(30.3853131747228,31.5775537673674,166.));
#30240=CARTESIAN_POINT('Ctrl Pts',(30.5228540701568,31.0546921657189,166.036314816837));
#30241=CARTESIAN_POINT('Ctrl Pts',(30.9381272764309,30.6037509899059,166.072629633674));
#30242=CARTESIAN_POINT('Ctrl Pts',(31.4484542245311,30.4250924216085,166.108944450512));
#30243=CARTESIAN_POINT('Ctrl Pts',(31.9690179238214,30.2428501050523,166.145987713585));
#30244=CARTESIAN_POINT('Ctrl Pts',(32.5884870162225,30.3439234982855,166.183030976658));
#30245=CARTESIAN_POINT('Ctrl Pts',(33.0238560935078,30.6822432557804,166.220074239731));
#30246=CARTESIAN_POINT('Ctrl Pts',(33.4592251707931,31.0205630132753,166.257117502805));
#30247=CARTESIAN_POINT('Ctrl Pts',(33.7104942329626,31.596129135032,166.294160765878));
#30248=CARTESIAN_POINT('Ctrl Pts',(33.6624582200325,32.1454771760265,166.331204028951));
#30249=CARTESIAN_POINT('Ctrl Pts',(33.6144222071025,32.6948252170211,166.368247292024));
#30250=CARTESIAN_POINT('Ctrl Pts',(33.267081119073,33.2179551772535,166.405290555098));
#30251=CARTESIAN_POINT('Ctrl Pts',(32.7794871827661,33.4755290749605,166.442333818171));
#30252=CARTESIAN_POINT('Ctrl Pts',(32.2918932464593,33.7331029726675,166.479377081244));
#30253=CARTESIAN_POINT('Ctrl Pts',(31.6640464618751,33.7251208078489,166.516420344317));
#30254=CARTESIAN_POINT('Ctrl Pts',(31.1831916842018,33.4552138375921,166.553463607391));
#30255=CARTESIAN_POINT('Ctrl Pts',(30.7023369065286,33.1853068673354,166.590506870464));
#30256=CARTESIAN_POINT('Ctrl Pts',(30.3684741357662,32.6534750916404,166.627550133537));
#30257=CARTESIAN_POINT('Ctrl Pts',(30.33440389687,32.1030923269707,166.66459339661));
#30258=CARTESIAN_POINT('Ctrl Pts',(30.3322924863733,32.0689838503585,166.666889052204));
#30259=CARTESIAN_POINT('Ctrl Pts',(30.3313324482509,32.0348041274879,166.669184707797));
#30260=CARTESIAN_POINT('Ctrl Pts',(30.3314948391898,32.0006151205084,166.67148036339));
#30261=CARTESIAN_POINT('Origin',(32.,32.,172.));
#30262=CARTESIAN_POINT('',(30.3358443517282,32.0011304728208,167.37148036339));
#30263=CARTESIAN_POINT('',(30.3361975399048,31.9991033790422,167.17851963661));
#30264=CARTESIAN_POINT('',(30.334,32.,172.));
#30265=CARTESIAN_POINT('Ctrl Pts',(30.3361975399048,31.9991033790422,167.17851963661));
#30266=CARTESIAN_POINT('Ctrl Pts',(30.3378409217978,32.3352358809299,167.156112388472));
#30267=CARTESIAN_POINT('Ctrl Pts',(30.4366194744036,32.6722563487497,167.133705140335));
#30268=CARTESIAN_POINT('Ctrl Pts',(30.6258906729461,32.9469160000523,167.111297892197));
#30269=CARTESIAN_POINT('Ctrl Pts',(30.9387904434473,33.4009784380794,167.074254629124));
#30270=CARTESIAN_POINT('Ctrl Pts',(31.4990076363489,33.6846080609293,167.037211366051));
#30271=CARTESIAN_POINT('Ctrl Pts',(32.050193769109,33.6680232454317,167.000168102978));
#30272=CARTESIAN_POINT('Ctrl Pts',(32.6013799018691,33.6514384299341,166.963124839904));
#30273=CARTESIAN_POINT('Ctrl Pts',(33.1435349744877,33.334639176089,166.926081576831));
#30274=CARTESIAN_POINT('Ctrl Pts',(33.4285638919976,32.8625793893597,166.889038313758));
#30275=CARTESIAN_POINT('Ctrl Pts',(33.7135928095075,32.3905196026303,166.851995050685));
#30276=CARTESIAN_POINT('Ctrl Pts',(33.7414955719087,31.7631992830168,166.814951787611));
#30277=CARTESIAN_POINT('Ctrl Pts',(33.4995200560992,31.2677006586916,166.777908524538));
#30278=CARTESIAN_POINT('Ctrl Pts',(33.2575445402896,30.7722020343664,166.740865261465));
#30279=CARTESIAN_POINT('Ctrl Pts',(32.7456907462693,30.4085251053296,166.703821998392));
#30280=CARTESIAN_POINT('Ctrl Pts',(32.1981475596803,30.343037902655,166.666778735318));
#30281=CARTESIAN_POINT('Ctrl Pts',(31.6506043730913,30.2775506999803,166.629735472245));
#30282=CARTESIAN_POINT('Ctrl Pts',(31.0673717939337,30.5102532236679,166.592692209172));
#30283=CARTESIAN_POINT('Ctrl Pts',(30.7154003304443,30.9347609287045,166.555648946099));
#30284=CARTESIAN_POINT('Ctrl Pts',(30.4711155519947,31.2293892762612,166.529939176269));
#30285=CARTESIAN_POINT('Ctrl Pts',(30.3382295759115,31.6164104475238,166.504229406439));
#30286=CARTESIAN_POINT('Ctrl Pts',(30.3351639991694,32.0014707476285,166.47851963661));
#30287=CARTESIAN_POINT('Ctrl Pts',(30.3314948391898,32.0006151205084,166.67148036339));
#30288=CARTESIAN_POINT('Ctrl Pts',(30.3339528283677,31.4831219050117,166.70622797087));
#30289=CARTESIAN_POINT('Ctrl Pts',(30.5935659814505,30.9635016450492,166.74097557835));
#30290=CARTESIAN_POINT('Ctrl Pts',(31.0099645669336,30.6566269199928,166.77572318583));
#30291=CARTESIAN_POINT('Ctrl Pts',(31.4538731829234,30.329478031329,166.812766448903));
#30292=CARTESIAN_POINT('Ctrl Pts',(32.075968121933,30.2441140076456,166.849809711977));
#30293=CARTESIAN_POINT('Ctrl Pts',(32.5915885607143,30.4395994910286,166.88685297505));
#30294=CARTESIAN_POINT('Ctrl Pts',(33.1072089994956,30.6350849744116,166.923896238123));
#30295=CARTESIAN_POINT('Ctrl Pts',(33.5163549380486,31.1114199648611,166.960939501196));
#30296=CARTESIAN_POINT('Ctrl Pts',(33.6318002467858,31.6506349121444,166.99798276427));
#30297=CARTESIAN_POINT('Ctrl Pts',(33.747245555523,32.1898498594278,167.035026027343));
#30298=CARTESIAN_POINT('Ctrl Pts',(33.5689902344443,32.791944763545,167.072069290416));
#30299=CARTESIAN_POINT('Ctrl Pts',(33.1786045071229,33.1814048707878,167.109112553489));
#30300=CARTESIAN_POINT('Ctrl Pts',(32.7882187798016,33.5708649780306,167.146155816562));
#30301=CARTESIAN_POINT('Ctrl Pts',(32.1857026462376,33.747690288399,167.183199079636));
#30302=CARTESIAN_POINT('Ctrl Pts',(31.6467634583476,33.6309661992293,167.220242342709));
#30303=CARTESIAN_POINT('Ctrl Pts',(31.1078242704576,33.5142421100596,167.257285605782));
#30304=CARTESIAN_POINT('Ctrl Pts',(30.6324620282417,33.1039686213518,167.294328868856));
#30305=CARTESIAN_POINT('Ctrl Pts',(30.4382002913112,32.5878848039827,167.331372131929));
#30306=CARTESIAN_POINT('Ctrl Pts',(30.3680886249107,32.4016232323021,167.344741542416));
#30307=CARTESIAN_POINT('Ctrl Pts',(30.3345926862457,32.201578966841,167.358110952903));
#30308=CARTESIAN_POINT('Ctrl Pts',(30.3358443517282,32.0011304728208,167.37148036339));
#30309=CARTESIAN_POINT('Origin',(32.,32.,172.));
#30310=CARTESIAN_POINT('',(30.3355908397978,31.9987501653433,168.07148036339));
#30311=CARTESIAN_POINT('',(30.3318493159965,31.9990863362845,167.87851963661));
#30312=CARTESIAN_POINT('',(30.334,32.,172.));
#30313=CARTESIAN_POINT('Ctrl Pts',(30.3318493159965,31.9990863362845,167.87851963661));
#30314=CARTESIAN_POINT('Ctrl Pts',(30.3351438813141,32.4979922732345,167.845038633578));
#30315=CARTESIAN_POINT('Ctrl Pts',(30.5738270354749,32.9996326545442,167.811557630547));
#30316=CARTESIAN_POINT('Ctrl Pts',(30.9647290575101,33.3088316952852,167.778076627516));
#30317=CARTESIAN_POINT('Ctrl Pts',(31.3972216690526,33.6509284179376,167.741033364442));
#30318=CARTESIAN_POINT('Ctrl Pts',(32.0160473933025,33.7574551714892,167.703990101369));
#30319=CARTESIAN_POINT('Ctrl Pts',(32.538034988592,33.5796659719367,167.666946838296));
#30320=CARTESIAN_POINT('Ctrl Pts',(33.0600225838815,33.4018767723843,167.629903575223));
#30321=CARTESIAN_POINT('Ctrl Pts',(33.4851720502105,32.9397716197278,167.592860312149));
#30322=CARTESIAN_POINT('Ctrl Pts',(33.6189371865014,32.4048071616505,167.555817049076));
#30323=CARTESIAN_POINT('Ctrl Pts',(33.7527023227924,31.8698427035731,167.518773786003));
#30324=CARTESIAN_POINT('Ctrl Pts',(33.5950831290453,31.2620189400749,167.48173052293));
#30325=CARTESIAN_POINT('Ctrl Pts',(33.21820551876,30.859473064477,167.444687259856));
#30326=CARTESIAN_POINT('Ctrl Pts',(32.8413279084747,30.4569271888792,167.407643996783));
#30327=CARTESIAN_POINT('Ctrl Pts',(32.2451918816511,30.2596592011817,167.37060073371));
#30328=CARTESIAN_POINT('Ctrl Pts',(31.7025855934752,30.3579371810217,167.333557470637));
#30329=CARTESIAN_POINT('Ctrl Pts',(31.1599793052994,30.4562151608616,167.296514207563));
#30330=CARTESIAN_POINT('Ctrl Pts',(30.6709027557713,30.8500391082389,167.25947094449));
#30331=CARTESIAN_POINT('Ctrl Pts',(30.4591556550577,31.3591987085298,167.222427681417));
#30332=CARTESIAN_POINT('Ctrl Pts',(30.3754931083076,31.5603707138087,167.207791666481));
#30333=CARTESIAN_POINT('Ctrl Pts',(30.3351241121558,31.779547622449,167.193155651545));
#30334=CARTESIAN_POINT('Ctrl Pts',(30.3361975399048,31.9991033790422,167.17851963661));
#30335=CARTESIAN_POINT('Ctrl Pts',(30.3358443517282,32.0011304728208,167.37148036339));
#30336=CARTESIAN_POINT('Ctrl Pts',(30.3380607354761,31.6461867673313,167.395154215976));
#30337=CARTESIAN_POINT('Ctrl Pts',(30.4492298770393,31.2899755840575,167.418828068562));
#30338=CARTESIAN_POINT('Ctrl Pts',(30.658979462611,31.0067776828098,167.442501921148));
#30339=CARTESIAN_POINT('Ctrl Pts',(30.9871816024865,30.5636485250366,167.479545184222));
#30340=CARTESIAN_POINT('Ctrl Pts',(31.5567471138823,30.2992843555205,167.516588447295));
#30341=CARTESIAN_POINT('Ctrl Pts',(32.1070459976037,30.3346568202484,167.553631710368));
#30342=CARTESIAN_POINT('Ctrl Pts',(32.6573448813252,30.3700292849762,167.590674973441));
#30343=CARTESIAN_POINT('Ctrl Pts',(33.1883771373722,30.7051383839478,167.627718236515));
#30344=CARTESIAN_POINT('Ctrl Pts',(33.4571452403435,31.1866399931067,167.664761499588));
#30345=CARTESIAN_POINT('Ctrl Pts',(33.7259133433149,31.6681416022655,167.701804762661));
#30346=CARTESIAN_POINT('Ctrl Pts',(33.7324172932105,32.2960357216114,167.738848025734));
#30347=CARTESIAN_POINT('Ctrl Pts',(33.4736809396483,32.7830014153016,167.775891288808));
#30348=CARTESIAN_POINT('Ctrl Pts',(33.2149445860862,33.2699671089917,167.812934551881));
#30349=CARTESIAN_POINT('Ctrl Pts',(32.6909679290662,33.6160043770262,167.849977814954));
#30350=CARTESIAN_POINT('Ctrl Pts',(32.1415198349773,33.6627684376593,167.887021078027));
#30351=CARTESIAN_POINT('Ctrl Pts',(31.5920717408885,33.7095324982925,167.924064341101));
#30352=CARTESIAN_POINT('Ctrl Pts',(31.0171522097308,33.4570233515244,167.961107604174));
#30353=CARTESIAN_POINT('Ctrl Pts',(30.6798413068547,33.0207878158059,167.998150867247));
#30354=CARTESIAN_POINT('Ctrl Pts',(30.4572651756015,32.7329358162782,168.022594032628));
#30355=CARTESIAN_POINT('Ctrl Pts',(30.3381457458446,32.3650878741953,168.047037198009));
#30356=CARTESIAN_POINT('Ctrl Pts',(30.3355908397978,31.9987501653433,168.07148036339));
#30357=CARTESIAN_POINT('Origin',(32.,32.,172.));
#30358=CARTESIAN_POINT('',(30.3313481286181,31.9995820784511,168.77148036339));
#30359=CARTESIAN_POINT('',(30.3334458852718,32.0014790085581,168.57851963661));
#30360=CARTESIAN_POINT('',(30.334,32.,172.));
#30361=CARTESIAN_POINT('Ctrl Pts',(30.3334458852718,32.0014790085581,168.57851963661));
#30362=CARTESIAN_POINT('Ctrl Pts',(30.3324126167116,32.113688095481,168.571008141758));
#30363=CARTESIAN_POINT('Ctrl Pts',(30.3427777067538,32.225707371916,168.563496646906));
#30364=CARTESIAN_POINT('Ctrl Pts',(30.3652410885464,32.3352456102263,168.555985152054));
#30365=CARTESIAN_POINT('Ctrl Pts',(30.4760202314001,32.875438189497,168.51894188898));
#30366=CARTESIAN_POINT('Ctrl Pts',(30.8810312884822,33.3552916224022,168.481898625907));
#30367=CARTESIAN_POINT('Ctrl Pts',(31.3949433957783,33.5552275793839,168.444855362834));
#30368=CARTESIAN_POINT('Ctrl Pts',(31.9088555030743,33.7551635363657,168.407812099761));
#30369=CARTESIAN_POINT('Ctrl Pts',(32.5316686605844,33.675182017424,168.370768836687));
#30370=CARTESIAN_POINT('Ctrl Pts',(32.9783869452582,33.3518821330796,168.333725573614));
#30371=CARTESIAN_POINT('Ctrl Pts',(33.425105229932,33.0285822487352,168.296682310541));
#30372=CARTESIAN_POINT('Ctrl Pts',(33.6957286417695,32.4619639989881,168.259639047468));
#30373=CARTESIAN_POINT('Ctrl Pts',(33.6664213733557,31.9113088202529,168.222595784395));
#30374=CARTESIAN_POINT('Ctrl Pts',(33.6371141049419,31.3606536415177,168.185552521321));
#30375=CARTESIAN_POINT('Ctrl Pts',(33.3078761562767,30.8259615337943,168.148509258248));
#30376=CARTESIAN_POINT('Ctrl Pts',(32.8293650306118,30.5519047110331,168.111465995175));
#30377=CARTESIAN_POINT('Ctrl Pts',(32.3508539049469,30.2778478882719,168.074422732102));
#30378=CARTESIAN_POINT('Ctrl Pts',(31.7230696022823,30.2644263504728,168.037379469028));
#30379=CARTESIAN_POINT('Ctrl Pts',(31.2332828090634,30.517781710982,168.000336205955));
#30380=CARTESIAN_POINT('Ctrl Pts',(30.7434960158445,30.7711370714911,167.963292942882));
#30381=CARTESIAN_POINT('Ctrl Pts',(30.3917067320712,31.2912693303086,167.926249679809));
#30382=CARTESIAN_POINT('Ctrl Pts',(30.338891839602,31.840168805594,167.889206416735));
#30383=CARTESIAN_POINT('Ctrl Pts',(30.3338129030979,31.8929536443358,167.885644156694));
#30384=CARTESIAN_POINT('Ctrl Pts',(30.331498785925,31.9460045130738,167.882081896652));
#30385=CARTESIAN_POINT('Ctrl Pts',(30.3318493159965,31.9990863362845,167.87851963661));
#30386=CARTESIAN_POINT('Ctrl Pts',(30.3355908397978,31.9987501653433,168.07148036339));
#30387=CARTESIAN_POINT('Ctrl Pts',(30.3342738227387,31.8099083828695,168.084080461082));
#30388=CARTESIAN_POINT('Ctrl Pts',(30.363930950585,31.6214679075983,168.096680558775));
#30389=CARTESIAN_POINT('Ctrl Pts',(30.4263577007272,31.4445932559108,168.109280656467));
#30390=CARTESIAN_POINT('Ctrl Pts',(30.6098872720703,30.924596156403,168.14632391954));
#30391=CARTESIAN_POINT('Ctrl Pts',(31.0766486893511,30.5045638820563,168.183367182613));
#30392=CARTESIAN_POINT('Ctrl Pts',(31.6130544602,30.3767009245792,168.220410445687));
#30393=CARTESIAN_POINT('Ctrl Pts',(32.1494602310488,30.2488379671021,168.25745370876));
#30394=CARTESIAN_POINT('Ctrl Pts',(32.7555103554658,30.4131443264948,168.294496971833));
#30395=CARTESIAN_POINT('Ctrl Pts',(33.153879582064,30.7944343033687,168.331540234906));
#30396=CARTESIAN_POINT('Ctrl Pts',(33.5522488086622,31.1757242802426,168.368583497979));
#30397=CARTESIAN_POINT('Ctrl Pts',(33.7429371374417,31.7739978745979,168.405626761053));
#30398=CARTESIAN_POINT('Ctrl Pts',(33.6386866234236,32.315488333781,168.442670024126));
#30399=CARTESIAN_POINT('Ctrl Pts',(33.5344361094055,32.8569787929641,168.479713287199));
#30400=CARTESIAN_POINT('Ctrl Pts',(33.1352467525898,33.3416861169752,168.516756550273));
#30401=CARTESIAN_POINT('Ctrl Pts',(32.6237854379909,33.5478108625037,168.553799813346));
#30402=CARTESIAN_POINT('Ctrl Pts',(32.112324123392,33.7539356080322,168.590843076419));
#30403=CARTESIAN_POINT('Ctrl Pts',(31.4885908510098,33.6814777750783,168.627886339492));
#30404=CARTESIAN_POINT('Ctrl Pts',(31.0380025843074,33.3635936751443,168.664929602565));
#30405=CARTESIAN_POINT('Ctrl Pts',(30.6059805047824,33.0588077762426,168.70044652284));
#30406=CARTESIAN_POINT('Ctrl Pts',(30.3331287484094,32.5284041757398,168.735963443115));
#30407=CARTESIAN_POINT('Ctrl Pts',(30.3313481286181,31.9995820784511,168.77148036339));
#30408=CARTESIAN_POINT('Origin',(32.,32.,172.));
#30409=CARTESIAN_POINT('',(30.3343646149627,32.0015150182665,169.47148036339));
#30410=CARTESIAN_POINT('',(30.3366835095906,31.9999843286223,169.27851963661));
#30411=CARTESIAN_POINT('',(30.334,32.,172.));
#30412=CARTESIAN_POINT('Ctrl Pts',(30.3366835095906,31.9999843286223,169.27851963661));
#30413=CARTESIAN_POINT('Ctrl Pts',(30.3367069203412,32.2789861477807,169.259934386864));
#30414=CARTESIAN_POINT('Ctrl Pts',(30.4031258058091,32.5579984414641,169.241349137118));
#30415=CARTESIAN_POINT('Ctrl Pts',(30.535878000075,32.8007328436966,169.222763887372));
#30416=CARTESIAN_POINT('Ctrl Pts',(30.8004735542359,33.2845398649497,169.185720624299));
#30417=CARTESIAN_POINT('Ctrl Pts',(31.3285889555581,33.6242270679139,169.148677361226));
#30418=CARTESIAN_POINT('Ctrl Pts',(31.8785614599778,33.6643554303822,169.111634098152));
#30419=CARTESIAN_POINT('Ctrl Pts',(32.4285339643976,33.7044837928504,169.074590835079));
#30420=CARTESIAN_POINT('Ctrl Pts',(33.000363571915,33.4450533148228,169.037547572006));
#30421=CARTESIAN_POINT('Ctrl Pts',(33.3323841547577,33.0047779763573,169.000504308933));
#30422=CARTESIAN_POINT('Ctrl Pts',(33.6644047376003,32.5645026378919,168.963461045859));
#30423=CARTESIAN_POINT('Ctrl Pts',(33.7566162957683,31.9433824389887,168.926417782786));
#30424=CARTESIAN_POINT('Ctrl Pts',(33.5668233202183,31.4256386147494,168.889374519713));
#30425=CARTESIAN_POINT('Ctrl Pts',(33.3770303446684,30.9078947905101,168.85233125664));
#30426=CARTESIAN_POINT('Ctrl Pts',(32.9052328354007,30.4935273409347,168.815287993566));
#30427=CARTESIAN_POINT('Ctrl Pts',(32.367322774485,30.3721485642009,168.778244730493));
#30428=CARTESIAN_POINT('Ctrl Pts',(31.8294127135693,30.2507697874672,168.74120146742));
#30429=CARTESIAN_POINT('Ctrl Pts',(31.2253901010056,30.4223796835752,168.704158204347));
#30430=CARTESIAN_POINT('Ctrl Pts',(30.8316524090365,30.8084504944473,168.667114941273));
#30431=CARTESIAN_POINT('Ctrl Pts',(30.517755379064,31.1162353049026,168.637583173052));
#30432=CARTESIAN_POINT('Ctrl Pts',(30.3375082254896,31.5603241102872,168.608051404831));
#30433=CARTESIAN_POINT('Ctrl Pts',(30.3334458852718,32.0014790085581,168.57851963661));
#30434=CARTESIAN_POINT('Ctrl Pts',(30.3313481286181,31.9995820784511,168.77148036339));
#30435=CARTESIAN_POINT('Ctrl Pts',(30.3312716063247,31.9768559019265,168.773006706189));
#30436=CARTESIAN_POINT('Ctrl Pts',(30.3316957139953,31.9541326462143,168.774533048987));
#30437=CARTESIAN_POINT('Ctrl Pts',(30.332629333074,31.9314303438645,168.776059391785));
#30438=CARTESIAN_POINT('Ctrl Pts',(30.3552876095656,31.3804614794328,168.813102654858));
#30439=CARTESIAN_POINT('Ctrl Pts',(30.6780474235711,30.8418341174834,168.850145917932));
#30440=CARTESIAN_POINT('Ctrl Pts',(31.1532156343118,30.5620212182661,168.887189181005));
#30441=CARTESIAN_POINT('Ctrl Pts',(31.6283838450525,30.2822083190488,168.924232444078));
#30442=CARTESIAN_POINT('Ctrl Pts',(32.2559604525283,30.2612098825636,168.961275707151));
#30443=CARTESIAN_POINT('Ctrl Pts',(32.748769804042,30.5086346794834,168.998318970225));
#30444=CARTESIAN_POINT('Ctrl Pts',(33.2415791555557,30.7560594764032,169.035362233298));
#30445=CARTESIAN_POINT('Ctrl Pts',(33.5996212511073,31.271907506728,169.072405496371));
#30446=CARTESIAN_POINT('Ctrl Pts',(33.6590579691791,31.8201295088524,169.109448759444));
#30447=CARTESIAN_POINT('Ctrl Pts',(33.7184946872509,32.3683515109768,169.146492022518));
#30448=CARTESIAN_POINT('Ctrl Pts',(33.479326027843,32.9489474849006,169.183535285591));
#30449=CARTESIAN_POINT('Ctrl Pts',(33.0509942726601,33.2962398611062,169.220578548664));
#30450=CARTESIAN_POINT('Ctrl Pts',(32.6226625174773,33.6435322373118,169.257621811737));
#30451=CARTESIAN_POINT('Ctrl Pts',(32.0051676665196,33.7575210157991,169.294665074811));
#30452=CARTESIAN_POINT('Ctrl Pts',(31.4810720153599,33.5860455496112,169.331708337884));
#30453=CARTESIAN_POINT('Ctrl Pts',(30.9569763642001,33.4145700834232,169.368751600957));
#30454=CARTESIAN_POINT('Ctrl Pts',(30.5262799128384,32.95763037256,169.40579486403));
#30455=CARTESIAN_POINT('Ctrl Pts',(30.3860670220631,32.4243195510599,169.442838127103));
#30456=CARTESIAN_POINT('Ctrl Pts',(30.3499290002398,32.2868657263839,169.452385539199));
#30457=CARTESIAN_POINT('Ctrl Pts',(30.3330872953841,32.144338701851,169.461932951295));
#30458=CARTESIAN_POINT('Ctrl Pts',(30.3343646149627,32.0015150182665,169.47148036339));
#30459=CARTESIAN_POINT('Origin',(32.,32.,172.));
#30460=CARTESIAN_POINT('',(30.3365390106164,31.9994923848488,170.17148036339));
#30461=CARTESIAN_POINT('',(30.3333883716037,31.9985292209557,169.97851963661));
#30462=CARTESIAN_POINT('',(30.334,32.,172.));
#30463=CARTESIAN_POINT('Ctrl Pts',(30.3333883716037,31.9985292209557,169.97851963661));
#30464=CARTESIAN_POINT('Ctrl Pts',(30.3374605996998,32.4415454791333,169.94886063197));
#30465=CARTESIAN_POINT('Ctrl Pts',(30.5194350922995,32.8875165487396,169.91920162733));
#30466=CARTESIAN_POINT('Ctrl Pts',(30.835741762519,33.1955455131847,169.88954262269));
#30467=CARTESIAN_POINT('Ctrl Pts',(31.2307999021651,33.5802650310069,169.852499359617));
#30468=CARTESIAN_POINT('Ctrl Pts',(31.8354069406125,33.7498044129371,169.815456096544));
#30469=CARTESIAN_POINT('Ctrl Pts',(32.3728979754128,33.6265833570929,169.778412833471));
#30470=CARTESIAN_POINT('Ctrl Pts',(32.910389010213,33.5033623012487,169.741369570397));
#30471=CARTESIAN_POINT('Ctrl Pts',(33.3807640413661,33.0873808076302,169.704326307324));
#30472=CARTESIAN_POINT('Ctrl Pts',(33.5687820051189,32.5689897521516,169.667283044251));
#30473=CARTESIAN_POINT('Ctrl Pts',(33.7567999688717,32.050598696673,169.630239781178));
#30474=CARTESIAN_POINT('Ctrl Pts',(33.6624608652242,31.4297980793344,169.593196518104));
#30475=CARTESIAN_POINT('Ctrl Pts',(33.3289337564728,30.9906628964783,169.556153255031));
#30476=CARTESIAN_POINT('Ctrl Pts',(32.9954066477213,30.5515277136221,169.519109991958));
#30477=CARTESIAN_POINT('Ctrl Pts',(32.4226915338659,30.2940579652485,169.482066728885));
#30478=CARTESIAN_POINT('Ctrl Pts',(31.872859745589,30.3360704121425,169.445023465812));
#30479=CARTESIAN_POINT('Ctrl Pts',(31.323027957312,30.3780828590364,169.407980202738));
#30480=CARTESIAN_POINT('Ctrl Pts',(30.7960794946136,30.7195775011981,169.370936939665));
#30481=CARTESIAN_POINT('Ctrl Pts',(30.5331431167641,31.2042882420498,169.333893676592));
#30482=CARTESIAN_POINT('Ctrl Pts',(30.4021264955506,31.4458111688191,169.315435663264));
#30483=CARTESIAN_POINT('Ctrl Pts',(30.3366602591122,31.7228925829223,169.296977649937));
#30484=CARTESIAN_POINT('Ctrl Pts',(30.3366835095906,31.9999843286223,169.27851963661));
#30485=CARTESIAN_POINT('Ctrl Pts',(30.3343646149627,32.0015150182665,169.47148036339));
#30486=CARTESIAN_POINT('Ctrl Pts',(30.3380432022527,31.5901932191653,169.498976214368));
#30487=CARTESIAN_POINT('Ctrl Pts',(30.492000619283,31.1764109357676,169.526472065346));
#30488=CARTESIAN_POINT('Ctrl Pts',(30.7681159877996,30.8742609009325,169.553967916323));
#30489=CARTESIAN_POINT('Ctrl Pts',(31.1401071745005,30.467195004442,169.591011179397));
#30490=CARTESIAN_POINT('Ctrl Pts',(31.7338188780912,30.262745143598,169.62805444247));
#30491=CARTESIAN_POINT('Ctrl Pts',(32.2775718422762,30.3544664661395,169.665097705543));
#30492=CARTESIAN_POINT('Ctrl Pts',(32.8213248064612,30.4461877886809,169.702140968616));
#30493=CARTESIAN_POINT('Ctrl Pts',(33.3151190312405,30.8340802946078,169.73918423169));
#30494=CARTESIAN_POINT('Ctrl Pts',(33.5329969568429,31.3406464764675,169.776227494763));
#30495=CARTESIAN_POINT('Ctrl Pts',(33.7508748824452,31.8472126583272,169.813270757836));
#30496=CARTESIAN_POINT('Ctrl Pts',(33.6928365088705,32.4724525161198,169.850314020909));
#30497=CARTESIAN_POINT('Ctrl Pts',(33.3854398811667,32.9302596811413,169.887357283983));
#30498=CARTESIAN_POINT('Ctrl Pts',(33.0780432534628,33.3880668461628,169.924400547056));
#30499=CARTESIAN_POINT('Ctrl Pts',(32.5212883716297,33.6784413184132,169.961443810129));
#30500=CARTESIAN_POINT('Ctrl Pts',(31.9699432507166,33.6685093138807,169.998487073202));
#30501=CARTESIAN_POINT('Ctrl Pts',(31.4185981298035,33.6585773093483,170.035530336275));
#30502=CARTESIAN_POINT('Ctrl Pts',(30.8726627698104,33.348338828033,170.072573599349));
#30503=CARTESIAN_POINT('Ctrl Pts',(30.5819542312589,32.8797573167866,170.109616862422));
#30504=CARTESIAN_POINT('Ctrl Pts',(30.4201232039306,32.6189083313048,170.130238029411));
#30505=CARTESIAN_POINT('Ctrl Pts',(30.3373844972543,32.3089903740528,170.150859196401));
#30506=CARTESIAN_POINT('Ctrl Pts',(30.3365390106164,31.9994923848488,170.17148036339));
#30507=CARTESIAN_POINT('Origin',(32.,32.,172.));
#30508=CARTESIAN_POINT('',(30.3325050746568,31.9987546321113,170.87148036339));
#30509=CARTESIAN_POINT('',(30.3318905055228,32.0009409351765,170.67851963661));
#30510=CARTESIAN_POINT('',(30.334,32.,172.));
#30511=CARTESIAN_POINT('Ctrl Pts',(30.3318905055228,32.0009409351765,170.67851963661));
#30512=CARTESIAN_POINT('Ctrl Pts',(30.3315188134717,32.0559223042009,170.674830140149));
#30513=CARTESIAN_POINT('Ctrl Pts',(30.3340015814678,32.1108696948638,170.671140643689));
#30514=CARTESIAN_POINT('Ctrl Pts',(30.3394492078326,32.1655215522844,170.667451147229));
#30515=CARTESIAN_POINT('Ctrl Pts',(30.3941444375797,32.7142368454346,170.630407884155));
#30516=CARTESIAN_POINT('Ctrl Pts',(30.7477137303999,33.2331607590674,170.593364621082));
#30517=CARTESIAN_POINT('Ctrl Pts',(31.2383656950483,33.4848365240522,170.556321358009));
#30518=CARTESIAN_POINT('Ctrl Pts',(31.7290176596967,33.736512289037,170.519278094935));
#30519=CARTESIAN_POINT('Ctrl Pts',(32.3567522961734,33.7209399053737,170.482234831862));
#30520=CARTESIAN_POINT('Ctrl Pts',(32.8343216385758,33.445245211389,170.445191568789));
#30521=CARTESIAN_POINT('Ctrl Pts',(33.3118909809782,33.1695505174043,170.408148305716));
#30522=CARTESIAN_POINT('Ctrl Pts',(33.6392950293065,32.6337335130981,170.371105042643));
#30523=CARTESIAN_POINT('Ctrl Pts',(33.6667154663201,32.0829811542943,170.334061779569));
#30524=CARTESIAN_POINT('Ctrl Pts',(33.6941359033337,31.5322287954904,170.297018516496));
#30525=CARTESIAN_POINT('Ctrl Pts',(33.4215727290326,30.9665410821889,170.259975253423));
#30526=CARTESIAN_POINT('Ctrl Pts',(32.9737493740648,30.6447736446826,170.22293199035));
#30527=CARTESIAN_POINT('Ctrl Pts',(32.525926019097,30.3230062071763,170.185888727276));
#30528=CARTESIAN_POINT('Ctrl Pts',(31.9028424834624,30.2451590454651,170.148845464203));
#30529=CARTESIAN_POINT('Ctrl Pts',(31.3896184145377,30.4468545986395,170.11180220113));
#30530=CARTESIAN_POINT('Ctrl Pts',(30.8763943456129,30.648550151814,170.074758938057));
#30531=CARTESIAN_POINT('Ctrl Pts',(30.473029743398,31.129788419874,170.037715674983));
#30532=CARTESIAN_POINT('Ctrl Pts',(30.364102062713,31.6703573807611,170.00067241191));
#30533=CARTESIAN_POINT('Ctrl Pts',(30.3423882589603,31.7781151908759,169.993288153477));
#30534=CARTESIAN_POINT('Ctrl Pts',(30.3323745012792,31.888230625965,169.985903895043));
#30535=CARTESIAN_POINT('Ctrl Pts',(30.3333883716037,31.9985292209557,169.97851963661));
#30536=CARTESIAN_POINT('Ctrl Pts',(30.3365390106164,31.9994923848488,170.17148036339));
#30537=CARTESIAN_POINT('Ctrl Pts',(30.3358656897121,31.753017211109,170.187902459474));
#30538=CARTESIAN_POINT('Ctrl Pts',(30.3871295825161,31.5068083838415,170.204324555558));
#30539=CARTESIAN_POINT('Ctrl Pts',(30.491745321287,31.2858609639402,170.220746651642));
#30540=CARTESIAN_POINT('Ctrl Pts',(30.7277266669766,30.7874706635177,170.257789914715));
#30541=CARTESIAN_POINT('Ctrl Pts',(31.2351710754656,30.4176146038501,170.294833177788));
#30542=CARTESIAN_POINT('Ctrl Pts',(31.7818747369324,30.3455369123804,170.331876440861));
#30543=CARTESIAN_POINT('Ctrl Pts',(32.3285783983991,30.2734592209107,170.368919703935));
#30544=CARTESIAN_POINT('Ctrl Pts',(32.9145413128434,30.4991598976388,170.405962967008));
#30545=CARTESIAN_POINT('Ctrl Pts',(33.2716300278673,30.919359536705,170.443006230081));
#30546=CARTESIAN_POINT('Ctrl Pts',(33.6287187428911,31.3395591757712,170.480049493154));
#30547=CARTESIAN_POINT('Ctrl Pts',(33.7569332584945,31.9542577771753,170.517092756228));
#30548=CARTESIAN_POINT('Ctrl Pts',(33.5976033075515,32.4821725939794,170.554136019301));
#30549=CARTESIAN_POINT('Ctrl Pts',(33.4382733566085,33.0100874107834,170.591179282374));
#30550=CARTESIAN_POINT('Ctrl Pts',(32.9913989391192,33.4512184429872,170.628222545447));
#30551=CARTESIAN_POINT('Ctrl Pts',(32.461467365451,33.6037065221879,170.665265808521));
#30552=CARTESIAN_POINT('Ctrl Pts',(31.9315357917828,33.7561946013885,170.702309071594));
#30553=CARTESIAN_POINT('Ctrl Pts',(31.3185470619358,33.6200397275859,170.739352334667));
#30554=CARTESIAN_POINT('Ctrl Pts',(30.9030014948949,33.2575456327631,170.77639559774));
#30555=CARTESIAN_POINT('Ctrl Pts',(30.5474527879603,32.9473887765523,170.808090519624));
#30556=CARTESIAN_POINT('Ctrl Pts',(30.3364490562282,32.471532604018,170.839785441507));
#30557=CARTESIAN_POINT('Ctrl Pts',(30.3325050746568,31.9987546321113,170.87148036339));
#30558=CARTESIAN_POINT('Origin',(32.,32.,172.));
#30559=CARTESIAN_POINT('',(30.3326609038217,32.0013000933536,171.57148036339));
#30560=CARTESIAN_POINT('',(30.3362278621005,32.0008713646937,171.37851963661));
#30561=CARTESIAN_POINT('',(30.334,32.,172.));
#30562=CARTESIAN_POINT('Ctrl Pts',(30.3362278621005,32.0008713646937,171.37851963661));
#30563=CARTESIAN_POINT('Ctrl Pts',(30.3351774463097,32.2223456968917,171.363756385255));
#30564=CARTESIAN_POINT('Ctrl Pts',(30.3762757543327,32.4434460199116,171.348993133901));
#30565=CARTESIAN_POINT('Ctrl Pts',(30.4613604710716,32.6460764023376,171.334229882547));
#30566=CARTESIAN_POINT('Ctrl Pts',(30.6748510816438,33.1545071255354,171.297186619474));
#30567=CARTESIAN_POINT('Ctrl Pts',(31.165273569148,33.5466538540894,171.2601433564));
#30568=CARTESIAN_POINT('Ctrl Pts',(31.7082132625074,33.6430723713403,171.223100093327));
#30569=CARTESIAN_POINT('Ctrl Pts',(32.2511529558667,33.7394908885913,171.186056830254));
#30570=CARTESIAN_POINT('Ctrl Pts',(32.8466098550813,33.5401811945391,171.149013567181));
#30571=CARTESIAN_POINT('Ctrl Pts',(33.222106111801,33.1363463244703,171.111970304107));
#30572=CARTESIAN_POINT('Ctrl Pts',(33.5976023685207,32.7325114544016,171.074927041034));
#30573=CARTESIAN_POINT('Ctrl Pts',(33.7531379827457,32.1241514083162,171.037883777961));
#30574=CARTESIAN_POINT('Ctrl Pts',(33.6175407007633,31.5896484446078,171.000840514888));
#30575=CARTESIAN_POINT('Ctrl Pts',(33.4819434187809,31.0551454808995,170.963797251814));
#30576=CARTESIAN_POINT('Ctrl Pts',(33.0552132405911,30.5944995995682,170.926753988741));
#30577=CARTESIAN_POINT('Ctrl Pts',(32.5326195818855,30.4184998581629,170.889710725668));
#30578=CARTESIAN_POINT('Ctrl Pts',(32.0100259231799,30.2425001167576,170.852667462595));
#30579=CARTESIAN_POINT('Ctrl Pts',(31.3915687839586,30.3511465152783,170.815624199521));
#30580=CARTESIAN_POINT('Ctrl Pts',(30.9602507976849,30.6947230508724,170.778580936448));
#30581=CARTESIAN_POINT('Ctrl Pts',(30.5718919368139,31.0040794798452,170.745227169835));
#30582=CARTESIAN_POINT('Ctrl Pts',(30.3352506740603,31.5038986503701,170.711873403223));
#30583=CARTESIAN_POINT('Ctrl Pts',(30.3318905055228,32.0009409351765,170.67851963661));
#30584=CARTESIAN_POINT('Ctrl Pts',(30.3325050746568,31.9987546321113,170.87148036339));
#30585=CARTESIAN_POINT('Ctrl Pts',(30.3318395497766,31.9189759877552,170.87682870458));
#30586=CARTESIAN_POINT('Ctrl Pts',(30.3370699848296,31.8392849941742,170.88217704577));
#30587=CARTESIAN_POINT('Ctrl Pts',(30.3484967597576,31.760492617748,170.88752538696));
#30588=CARTESIAN_POINT('Ctrl Pts',(30.4276399958959,31.2147670133988,170.924568650033));
#30589=CARTESIAN_POINT('Ctrl Pts',(30.804028872407,30.7121491205435,170.961611913106));
#30590=CARTESIAN_POINT('Ctrl Pts',(31.3054298802833,30.4826341616206,170.99865517618));
#30591=CARTESIAN_POINT('Ctrl Pts',(31.8068308881596,30.2531192026977,171.035698439253));
#30592=CARTESIAN_POINT('Ctrl Pts',(32.4332440274009,30.2967071777072,171.072741702326));
#30593=CARTESIAN_POINT('Ctrl Pts',(32.8980260420744,30.5934524656307,171.109784965399));
#30594=CARTESIAN_POINT('Ctrl Pts',(33.3628080567478,30.8901977535542,171.146828228473));
#30595=CARTESIAN_POINT('Ctrl Pts',(33.6659589468533,31.4401003543917,171.183871491546));
#30596=CARTESIAN_POINT('Ctrl Pts',(33.6687585088459,31.9915278197227,171.220914754619));
#30597=CARTESIAN_POINT('Ctrl Pts',(33.6715580708384,32.5429552850537,171.257958017692));
#30598=CARTESIAN_POINT('Ctrl Pts',(33.374006304718,33.0959076148782,171.295001280766));
#30599=CARTESIAN_POINT('Ctrl Pts',(32.9122612852541,33.3973568213276,171.332044543839));
#30600=CARTESIAN_POINT('Ctrl Pts',(32.4505162657902,33.698806027777,171.369087806912));
#30601=CARTESIAN_POINT('Ctrl Pts',(31.8245779929827,33.7487521108513,171.406131069985));
#30602=CARTESIAN_POINT('Ctrl Pts',(31.3208724264595,33.5243400137571,171.443174333059));
#30603=CARTESIAN_POINT('Ctrl Pts',(30.8171668599362,33.299927916663,171.480217596132));
#30604=CARTESIAN_POINT('Ctrl Pts',(30.4356939996972,32.8011576394003,171.517260859205));
#30605=CARTESIAN_POINT('Ctrl Pts',(30.3510137581373,32.2562637563753,171.554304122278));
#30606=CARTESIAN_POINT('Ctrl Pts',(30.3379255640836,32.1720448553858,171.560029535982));
#30607=CARTESIAN_POINT('Ctrl Pts',(30.3319274048857,32.0867241144181,171.565754949686));
#30608=CARTESIAN_POINT('Ctrl Pts',(30.3326609038217,32.0013000933536,171.57148036339));
#30609=CARTESIAN_POINT('Origin',(32.,32.,172.));
#30610=CARTESIAN_POINT('',(30.3365860283557,32.0004190115501,172.27148036339));
#30611=CARTESIAN_POINT('',(30.3350677280756,31.9985848365712,172.07851963661));
#30612=CARTESIAN_POINT('',(30.334,32.,172.));
#30613=CARTESIAN_POINT('Ctrl Pts',(30.3350677280756,31.9985848365712,172.07851963661));
#30614=CARTESIAN_POINT('Ctrl Pts',(30.3381924982781,32.3855055066604,172.052682630362));
#30615=CARTESIAN_POINT('Ctrl Pts',(30.4725557093059,32.7743832562982,172.026845624113));
#30616=CARTESIAN_POINT('Ctrl Pts',(30.7190756776316,33.0696070297093,172.001008617865));
#30617=CARTESIAN_POINT('Ctrl Pts',(31.072518485663,33.4928778916226,171.963965354792));
#30618=CARTESIAN_POINT('Ctrl Pts',(31.6565083257521,33.723635642604,171.926922091719));
#30619=CARTESIAN_POINT('Ctrl Pts',(32.2038146136273,33.6562867870361,171.889878828646));
#30620=CARTESIAN_POINT('Ctrl Pts',(32.7511209015025,33.5889379314683,171.852835565572));
#30621=CARTESIAN_POINT('Ctrl Pts',(33.2617436371637,33.2234824693511,171.815792302499));
#30622=CARTESIAN_POINT('Ctrl Pts',(33.5020246255088,32.7271508385498,171.778749039426));
#30623=CARTESIAN_POINT('Ctrl Pts',(33.7423056138539,32.2308192077485,171.741705776353));
#30624=CARTESIAN_POINT('Ctrl Pts',(33.712244854883,31.6036114082629,171.704662513279));
#30625=CARTESIAN_POINT('Ctrl Pts',(33.4255979889034,31.1325343282452,171.667619250206));
#30626=CARTESIAN_POINT('Ctrl Pts',(33.1389511229238,30.6614572482273,171.630575987133));
#30627=CARTESIAN_POINT('Ctrl Pts',(32.5957181499356,30.3465108876772,171.59353272406));
#30628=CARTESIAN_POINT('Ctrl Pts',(32.04447953282,30.3318129934571,171.556489460986));
#30629=CARTESIAN_POINT('Ctrl Pts',(31.4932409157044,30.3171150992369,171.519446197913));
#30630=CARTESIAN_POINT('Ctrl Pts',(30.9339966544615,30.6026656713466,171.48240293484));
#30631=CARTESIAN_POINT('Ctrl Pts',(30.6226538906602,31.0577983163223,171.445359671767));
#30632=CARTESIAN_POINT('Ctrl Pts',(30.4353939181147,31.3315420371081,171.423079660048));
#30633=CARTESIAN_POINT('Ctrl Pts',(30.3378131007155,31.6666326121062,171.400799648329));
#30634=CARTESIAN_POINT('Ctrl Pts',(30.3362278621005,32.0008713646937,171.37851963661));
#30635=CARTESIAN_POINT('Ctrl Pts',(30.3326609038217,32.0013000933536,171.57148036339));
#30636=CARTESIAN_POINT('Ctrl Pts',(30.3366731220436,31.5340331389412,171.60279821276));
#30637=CARTESIAN_POINT('Ctrl Pts',(30.5421005058999,31.0636759833655,171.634116062129));
#30638=CARTESIAN_POINT('Ctrl Pts',(30.8902894158567,30.7536576882235,171.665433911498));
#30639=CARTESIAN_POINT('Ctrl Pts',(31.3021329380168,30.386962991884,171.702477174571));
#30640=CARTESIAN_POINT('Ctrl Pts',(31.9137076052177,30.2445910879924,171.739520437645));
#30641=CARTESIAN_POINT('Ctrl Pts',(32.4451601658739,30.39169058779,171.776563700718));
#30642=CARTESIAN_POINT('Ctrl Pts',(32.9766127265301,30.5387900875876,171.813606963791));
#30643=CARTESIAN_POINT('Ctrl Pts',(33.4279431806416,30.9753609910743,171.850650226864));
#30644=CARTESIAN_POINT('Ctrl Pts',(33.5926251596443,31.5016308200218,171.887693489938));
#30645=CARTESIAN_POINT('Ctrl Pts',(33.7573071386471,32.0279006489693,171.924736753011));
#30646=CARTESIAN_POINT('Ctrl Pts',(33.6353406425412,32.6438694033776,171.961780016084));
#30647=CARTESIAN_POINT('Ctrl Pts',(33.2825368786089,33.067673121181,171.998823279157));
#30648=CARTESIAN_POINT('Ctrl Pts',(32.9297331146766,33.4914768389843,172.035866542231));
#30649=CARTESIAN_POINT('Ctrl Pts',(32.3460920829179,33.7231155201827,172.072909805304));
#30650=CARTESIAN_POINT('Ctrl Pts',(31.7986847548039,33.6565925602682,172.109953068377));
#30651=CARTESIAN_POINT('Ctrl Pts',(31.2512774266899,33.5900696003537,172.14699633145));
#30652=CARTESIAN_POINT('Ctrl Pts',(30.7401038022206,33.2253849993263,172.184039594523));
#30653=CARTESIAN_POINT('Ctrl Pts',(30.4990741602295,32.7294164531962,172.221082857597));
#30654=CARTESIAN_POINT('Ctrl Pts',(30.3897669000973,32.5044940642262,172.237882026195));
#30655=CARTESIAN_POINT('Ctrl Pts',(30.3360183819722,32.2525713668698,172.254681194792));
#30656=CARTESIAN_POINT('Ctrl Pts',(30.3365860283557,32.0004190115501,172.27148036339));
#30657=CARTESIAN_POINT('Origin',(32.,32.,172.));
#30658=CARTESIAN_POINT('',(30.3341968101826,31.9984781516629,172.97148036339));
#30659=CARTESIAN_POINT('',(30.3312207490626,31.9999631491892,172.77851963661));
#30660=CARTESIAN_POINT('',(30.334,32.,172.));
#30661=CARTESIAN_POINT('Ctrl Pts',(30.3312211427064,31.9999631544086,172.77851963661));
#30662=CARTESIAN_POINT('Ctrl Pts',(30.331399935389,32.5494261488841,172.741608875468));
#30663=CARTESIAN_POINT('Ctrl Pts',(30.6293022294751,33.0990552818063,172.704698114326));
#30664=CARTESIAN_POINT('Ctrl Pts',(31.0898482772994,33.398731625189,172.667787353184));
#30665=CARTESIAN_POINT('Ctrl Pts',(31.5520475893435,33.6994837441175,172.63074409011));
#30666=CARTESIAN_POINT('Ctrl Pts',(32.1780604653325,33.7484852957398,172.593700827037));
#30667=CARTESIAN_POINT('Ctrl Pts',(32.6814268076273,33.5233134357333,172.556657563964));
#30668=CARTESIAN_POINT('Ctrl Pts',(33.184793149922,33.2981415757268,172.519614300891));
#30669=CARTESIAN_POINT('Ctrl Pts',(33.5655129585226,32.7987963040915,172.482571037817));
#30670=CARTESIAN_POINT('Ctrl Pts',(33.6493709133806,32.2537753095408,172.445527774744));
#30671=CARTESIAN_POINT('Ctrl Pts',(33.7332288682386,31.7087543149901,172.408484511671));
#30672=CARTESIAN_POINT('Ctrl Pts',(33.520224969354,31.1180575975239,172.371441248598));
#30673=CARTESIAN_POINT('Ctrl Pts',(33.1078286458908,30.7519847721352,172.334397985524));
#30674=CARTESIAN_POINT('Ctrl Pts',(32.6954323224276,30.3859119467466,172.297354722451));
#30675=CARTESIAN_POINT('Ctrl Pts',(32.0836435743859,30.2444630134353,172.260311459378));
#30676=CARTESIAN_POINT('Ctrl Pts',(31.5524136155831,30.3923642371099,172.223268196305));
#30677=CARTESIAN_POINT('Ctrl Pts',(31.0211836567803,30.5402654607845,172.186224933231));
#30678=CARTESIAN_POINT('Ctrl Pts',(30.5705124872166,30.9775168414449,172.149181670158));
#30679=CARTESIAN_POINT('Ctrl Pts',(30.4066247904215,31.5040345181977,172.112138407085));
#30680=CARTESIAN_POINT('Ctrl Pts',(30.3570457990374,31.6633156349002,172.10093215026));
#30681=CARTESIAN_POINT('Ctrl Pts',(30.3337124248693,31.8307661520737,172.089725893435));
#30682=CARTESIAN_POINT('Ctrl Pts',(30.3350677280756,31.9985848365712,172.07851963661));
#30683=CARTESIAN_POINT('Ctrl Pts',(30.3365860283557,32.0004190115501,172.27148036339));
#30684=CARTESIAN_POINT('Ctrl Pts',(30.3372700792925,31.6965589679093,172.291724457866));
#30685=CARTESIAN_POINT('Ctrl Pts',(30.4168311019023,31.3923654190436,172.311968552341));
#30686=CARTESIAN_POINT('Ctrl Pts',(30.5730946173501,31.1346863183511,172.332212646816));
#30687=CARTESIAN_POINT('Ctrl Pts',(30.8590303759745,30.6631772208688,172.36925590989));
#30688=CARTESIAN_POINT('Ctrl Pts',(31.4017875527363,30.347411517137,172.406299172963));
#30689=CARTESIAN_POINT('Ctrl Pts',(31.9530034065273,30.331881881015,172.443342436036));
#30690=CARTESIAN_POINT('Ctrl Pts',(32.5042192603184,30.316352244893,172.480385699109));
#30691=CARTESIAN_POINT('Ctrl Pts',(33.0638937911388,30.6010586763809,172.517428962183));
#30692=CARTESIAN_POINT('Ctrl Pts',(33.375922968394,31.0557210561862,172.554472225256));
#30693=CARTESIAN_POINT('Ctrl Pts',(33.6879521456491,31.5103834359915,172.591515488329));
#30694=CARTESIAN_POINT('Ctrl Pts',(33.7523359693389,32.1350017641142,172.628558751402));
#30695=CARTESIAN_POINT('Ctrl Pts',(33.5396127508497,32.6437540804571,172.665602014476));
#30696=CARTESIAN_POINT('Ctrl Pts',(33.3268895323605,33.1525063968,172.702645277549));
#30697=CARTESIAN_POINT('Ctrl Pts',(32.8370592716923,33.5453927013633,172.739688540622));
#30698=CARTESIAN_POINT('Ctrl Pts',(32.2942656401328,33.6426303515159,172.776731803695));
#30699=CARTESIAN_POINT('Ctrl Pts',(31.7514720085734,33.7398680016686,172.813775066769));
#30700=CARTESIAN_POINT('Ctrl Pts',(31.1557150061227,33.5414569974107,172.850818329842));
#30701=CARTESIAN_POINT('Ctrl Pts',(30.7796098067444,33.1381891384518,172.887861592915));
#30702=CARTESIAN_POINT('Ctrl Pts',(30.4966122903972,32.8347532840774,172.915734516407));
#30703=CARTESIAN_POINT('Ctrl Pts',(30.3379749552747,32.4153336990011,172.943607439898));
#30704=CARTESIAN_POINT('Ctrl Pts',(30.3341968101826,31.9984781516629,172.97148036339));
#30705=CARTESIAN_POINT('Origin',(32.,32.,172.));
#30706=CARTESIAN_POINT('',(30.331415601616,32.0005168033969,173.67148036339));
#30707=CARTESIAN_POINT('',(30.3349603589764,32.0014384974263,173.47851963661));
#30708=CARTESIAN_POINT('',(30.334,32.,172.));
#30709=CARTESIAN_POINT('Ctrl Pts',(30.3349603589764,32.0014384974263,173.47851963661));
#30710=CARTESIAN_POINT('Ctrl Pts',(30.3336089417427,32.1652618982138,173.467578383647));
#30711=CARTESIAN_POINT('Ctrl Pts',(30.355830596873,32.3287266852567,173.456637130684));
#30712=CARTESIAN_POINT('Ctrl Pts',(30.4031261763844,32.4845826132764,173.445695877722));
#30713=CARTESIAN_POINT('Ctrl Pts',(30.5632524982974,33.0122563781393,173.408652614648));
#30714=CARTESIAN_POINT('Ctrl Pts',(31.0107919906657,33.4527125913275,173.371609351575));
#30715=CARTESIAN_POINT('Ctrl Pts',(31.5409530084635,33.6044008779603,173.334566088502));
#30716=CARTESIAN_POINT('Ctrl Pts',(32.0711140262613,33.7560891645932,173.297522825429));
#30717=CARTESIAN_POINT('Ctrl Pts',(32.6838965694886,33.6190095246707,173.260479562355));
#30718=CARTESIAN_POINT('Ctrl Pts',(33.0988946690395,33.255888858138,173.223436299282));
#30719=CARTESIAN_POINT('Ctrl Pts',(33.5138927685904,32.8927681916053,173.186393036209));
#30720=CARTESIAN_POINT('Ctrl Pts',(33.731106424465,32.3036064984624,173.149349773136));
#30721=CARTESIAN_POINT('Ctrl Pts',(33.651139845527,31.7580009748953,173.112306510062));
#30722=CARTESIAN_POINT('Ctrl Pts',(33.571173266589,31.2123954513282,173.075263246989));
#30723=CARTESIAN_POINT('Ctrl Pts',(33.1940264528385,30.7103460973368,173.038219983916));
#30724=CARTESIAN_POINT('Ctrl Pts',(32.6922797412542,30.4815879750583,173.001176720843));
#30725=CARTESIAN_POINT('Ctrl Pts',(32.1905330296699,30.2528298527798,172.96413345777));
#30726=CARTESIAN_POINT('Ctrl Pts',(31.5641864202519,30.2973629622143,172.927090194696));
#30727=CARTESIAN_POINT('Ctrl Pts',(31.0998527252467,30.5948091939552,172.890046931623));
#30728=CARTESIAN_POINT('Ctrl Pts',(30.6355190302416,30.8922554256961,172.85300366855));
#30729=CARTESIAN_POINT('Ctrl Pts',(30.3331982496493,31.4426147797435,172.815960405477));
#30730=CARTESIAN_POINT('Ctrl Pts',(30.3312307334027,31.9940457998846,172.778917142403));
#30731=CARTESIAN_POINT('Ctrl Pts',(30.3312236956938,31.9960182415379,172.778784640472));
#30732=CARTESIAN_POINT('Ctrl Pts',(30.331220500878,31.9979906969028,172.778652138541));
#30733=CARTESIAN_POINT('Ctrl Pts',(30.3312211427064,31.9999631544086,172.77851963661));
#30734=CARTESIAN_POINT('Ctrl Pts',(30.3341968101826,31.9984781516629,172.97148036339));
#30735=CARTESIAN_POINT('Ctrl Pts',(30.3329537804196,31.8613304668622,172.980650702972));
#30736=CARTESIAN_POINT('Ctrl Pts',(30.3484734044008,31.7244603250137,172.989821042553));
#30737=CARTESIAN_POINT('Ctrl Pts',(30.3818418436429,31.5920895690238,172.998991382135));
#30738=CARTESIAN_POINT('Ctrl Pts',(30.5166324762257,31.0573825722146,173.036034645208));
#30739=CARTESIAN_POINT('Ctrl Pts',(30.9426671376973,30.5960932922563,173.073077908281));
#30740=CARTESIAN_POINT('Ctrl Pts',(31.464994677045,30.4193052024208,173.110121171354));
#30741=CARTESIAN_POINT('Ctrl Pts',(31.9873222163927,30.2425171125853,173.147164434428));
#30742=CARTESIAN_POINT('Ctrl Pts',(32.6059426336165,30.3502302128725,173.184207697501));
#30743=CARTESIAN_POINT('Ctrl Pts',(33.0377785801244,30.693155572641,173.221250960574));
#30744=CARTESIAN_POINT('Ctrl Pts',(33.4696145266322,31.0360809324095,173.258294223647));
#30745=CARTESIAN_POINT('Ctrl Pts',(33.7146660024241,31.6142185516594,173.295337486721));
#30746=CARTESIAN_POINT('Ctrl Pts',(33.660798780914,32.1630157906425,173.332380749794));
#30747=CARTESIAN_POINT('Ctrl Pts',(33.6069315594039,32.7118130296256,173.369424012867));
#30748=CARTESIAN_POINT('Ctrl Pts',(33.2541456405917,33.231269888342,173.40646727594));
#30749=CARTESIAN_POINT('Ctrl Pts',(32.7638739480239,33.4836857248806,173.443510539014));
#30750=CARTESIAN_POINT('Ctrl Pts',(32.2736022554562,33.7361015614192,173.480553802087));
#30751=CARTESIAN_POINT('Ctrl Pts',(31.6458447891329,33.72147637578,173.51759706516));
#30752=CARTESIAN_POINT('Ctrl Pts',(31.1678599617704,33.4465025736097,173.554640328233));
#30753=CARTESIAN_POINT('Ctrl Pts',(30.6898751344079,33.1715287714394,173.591683591307));
#30754=CARTESIAN_POINT('Ctrl Pts',(30.3616629460063,32.636206352738,173.62872685438));
#30755=CARTESIAN_POINT('Ctrl Pts',(30.3334115143217,32.0854959536384,173.665770117453));
#30756=CARTESIAN_POINT('Ctrl Pts',(30.331959854743,32.0571984841561,173.667673532766));
#30757=CARTESIAN_POINT('Ctrl Pts',(30.331300173107,32.0288603862224,173.669576948078));
#30758=CARTESIAN_POINT('Ctrl Pts',(30.331415601616,32.0005168033969,173.67148036339));
#30759=CARTESIAN_POINT('Origin',(32.,32.,172.));
#30760=CARTESIAN_POINT('',(30.3357185782339,32.0011936552705,174.37148036339));
#30761=CARTESIAN_POINT('',(30.336288627554,31.999183265941,174.17851963661));
#30762=CARTESIAN_POINT('',(30.334,32.,172.));
#30763=CARTESIAN_POINT('Ctrl Pts',(30.336288627554,31.999183265941,174.17851963661));
#30764=CARTESIAN_POINT('Ctrl Pts',(30.3377536367914,32.3294766934183,174.156504628753));
#30765=CARTESIAN_POINT('Ctrl Pts',(30.4328676987764,32.6605477827672,174.134489620897));
#30766=CARTESIAN_POINT('Ctrl Pts',(30.6159654584887,32.9323490256026,174.11247461304));
#30767=CARTESIAN_POINT('Ctrl Pts',(30.9240524928118,33.389691807743,174.075431349967));
#30768=CARTESIAN_POINT('Ctrl Pts',(31.4812448413513,33.679225846665,174.038388086894));
#30769=CARTESIAN_POINT('Ctrl Pts',(32.032574306665,33.6684619360908,174.00134482382));
#30770=CARTESIAN_POINT('Ctrl Pts',(32.5839037719788,33.6576980255166,173.964301560747));
#30771=CARTESIAN_POINT('Ctrl Pts',(33.1293703540669,33.3466361654461,173.927258297674));
#30772=CARTESIAN_POINT('Ctrl Pts',(33.4193715026352,32.877616576385,173.890215034601));
#30773=CARTESIAN_POINT('Ctrl Pts',(33.7093726512035,32.4085969873239,173.853171771527));
#30774=CARTESIAN_POINT('Ctrl Pts',(33.743908366252,31.781619669272,173.816128508454));
#30775=CARTESIAN_POINT('Ctrl Pts',(33.5071752918366,31.2835860433271,173.779085245381));
#30776=CARTESIAN_POINT('Ctrl Pts',(33.2704422174213,30.7855524173822,173.742041982308));
#30777=CARTESIAN_POINT('Ctrl Pts',(32.762440353542,30.4164624835441,173.704998719234));
#30778=CARTESIAN_POINT('Ctrl Pts',(32.2156285985846,30.3452097942304,173.667955456161));
#30779=CARTESIAN_POINT('Ctrl Pts',(31.6688168436272,30.2739571049167,173.630912193088));
#30780=CARTESIAN_POINT('Ctrl Pts',(31.0831951975917,30.5005416601273,173.593868930015));
#30781=CARTESIAN_POINT('Ctrl Pts',(30.7267409503027,30.9212795960015,173.556825666941));
#30782=CARTESIAN_POINT('Ctrl Pts',(30.4755705189,31.2177466171263,173.530723656831));
#30783=CARTESIAN_POINT('Ctrl Pts',(30.3381843687327,31.6106130519071,173.50462164672));
#30784=CARTESIAN_POINT('Ctrl Pts',(30.3349603589764,32.0014384974263,173.47851963661));
#30785=CARTESIAN_POINT('Ctrl Pts',(30.331415601616,32.0005168033969,173.67148036339));
#30786=CARTESIAN_POINT('Ctrl Pts',(30.3335465817587,31.477252553602,173.706620211151));
#30787=CARTESIAN_POINT('Ctrl Pts',(30.5998552011771,30.9521189104532,173.741760058912));
#30788=CARTESIAN_POINT('Ctrl Pts',(31.0242067755662,30.6462443640623,173.776899906673));
#30789=CARTESIAN_POINT('Ctrl Pts',(31.4715441434631,30.3238015530837,173.813943169746));
#30790=CARTESIAN_POINT('Ctrl Pts',(32.0945095542247,30.2450143106244,173.850986432819));
#30791=CARTESIAN_POINT('Ctrl Pts',(32.6080374137757,30.4459352516278,173.888029695893));
#30792=CARTESIAN_POINT('Ctrl Pts',(33.1215652733267,30.6468561926312,173.925072958966));
#30793=CARTESIAN_POINT('Ctrl Pts',(33.5256555816671,31.1274853170972,173.962116222039));
#30794=CARTESIAN_POINT('Ctrl Pts',(33.6353988047888,31.6678893437732,173.999159485112));
#30795=CARTESIAN_POINT('Ctrl Pts',(33.7451420279106,32.2082933704491,174.036202748185));
#30796=CARTESIAN_POINT('Ctrl Pts',(33.5605381658136,32.808472299335,174.073246011259));
#30797=CARTESIAN_POINT('Ctrl Pts',(33.1660609448208,33.1937875069073,174.110289274332));
#30798=CARTESIAN_POINT('Ctrl Pts',(32.771583723828,33.5791027144796,174.147332537405));
#30799=CARTESIAN_POINT('Ctrl Pts',(32.1672331439392,33.7495542007383,174.184375800478));
#30800=CARTESIAN_POINT('Ctrl Pts',(31.6295567535571,33.6271442898062,174.221419063552));
#30801=CARTESIAN_POINT('Ctrl Pts',(31.0918803631751,33.5047343788742,174.258462326625));
#30802=CARTESIAN_POINT('Ctrl Pts',(30.6208781622996,33.0894630707512,174.295505589698));
#30803=CARTESIAN_POINT('Ctrl Pts',(30.4320782041483,32.5713562643196,174.332548852772));
#30804=CARTESIAN_POINT('Ctrl Pts',(30.3659369145156,32.3898506502273,174.345526022978));
#30805=CARTESIAN_POINT('Ctrl Pts',(30.3344295720944,32.1957243029137,174.358503193184));
#30806=CARTESIAN_POINT('Ctrl Pts',(30.3357185782339,32.0011936552705,174.37148036339));
#30807=CARTESIAN_POINT('Origin',(32.,32.,172.));
#30808=CARTESIAN_POINT('',(30.3357235801798,31.9988086992918,175.07148036339));
#30809=CARTESIAN_POINT('',(30.3319793737621,31.999003930908,174.87851963661));
#30810=CARTESIAN_POINT('',(30.334,32.,172.));
#30811=CARTESIAN_POINT('Ctrl Pts',(30.3319793737621,31.999003930908,174.87851963661));
#30812=CARTESIAN_POINT('Ctrl Pts',(30.3354661445113,32.4921662044565,174.845430873859));
#30813=CARTESIAN_POINT('Ctrl Pts',(30.5678894507187,32.988184128635,174.812342111109));
#30814=CARTESIAN_POINT('Ctrl Pts',(30.950962884132,33.2978241202759,174.779253348358));
#30815=CARTESIAN_POINT('Ctrl Pts',(31.3798181446719,33.6444697701856,174.742210085285));
#30816=CARTESIAN_POINT('Ctrl Pts',(31.9974842423223,33.7575266796541,174.705166822212));
#30817=CARTESIAN_POINT('Ctrl Pts',(32.5213205199536,33.5852606199341,174.668123559139));
#30818=CARTESIAN_POINT('Ctrl Pts',(33.0451567975848,33.4129945602141,174.631080296065));
#30819=CARTESIAN_POINT('Ctrl Pts',(33.4751632551969,32.9554055313057,174.594037032992));
#30820=CARTESIAN_POINT('Ctrl Pts',(33.6145712693993,32.4218837916642,174.556993769919));
#30821=CARTESIAN_POINT('Ctrl Pts',(33.7539792836017,31.8883620520226,174.519950506846));
#30822=CARTESIAN_POINT('Ctrl Pts',(33.6027888543946,31.2789076016479,174.482907243772));
#30823=CARTESIAN_POINT('Ctrl Pts',(33.230183902387,30.8724034924024,174.445863980699));
#30824=CARTESIAN_POINT('Ctrl Pts',(32.8575789503795,30.4658993831569,174.408820717626));
#30825=CARTESIAN_POINT('Ctrl Pts',(32.2635594755717,30.2623456150405,174.371777454553));
#30826=CARTESIAN_POINT('Ctrl Pts',(31.7199455686991,30.354887288619,174.33473419148));
#30827=CARTESIAN_POINT('Ctrl Pts',(31.1763316618265,30.4474289621975,174.297690928406));
#30828=CARTESIAN_POINT('Ctrl Pts',(30.6831233228891,30.8360660774709,174.260647665333));
#30829=CARTESIAN_POINT('Ctrl Pts',(30.4660100134739,31.3429603977871,174.22360440226));
#30830=CARTESIAN_POINT('Ctrl Pts',(30.3779282962027,31.5486047331285,174.208576147043));
#30831=CARTESIAN_POINT('Ctrl Pts',(30.3352885582895,31.7737128070232,174.193547891827));
#30832=CARTESIAN_POINT('Ctrl Pts',(30.336288627554,31.999183265941,174.17851963661));
#30833=CARTESIAN_POINT('Ctrl Pts',(30.3357185782339,32.0011936552705,174.37148036339));
#30834=CARTESIAN_POINT('Ctrl Pts',(30.338109033238,31.640437607747,174.395546456257));
#30835=CARTESIAN_POINT('Ctrl Pts',(30.4532910651195,31.2782911105634,174.419612549124));
#30836=CARTESIAN_POINT('Ctrl Pts',(30.6695446788991,30.9926691818284,174.443678641991));
#30837=CARTESIAN_POINT('Ctrl Pts',(31.0024088272283,30.5530312105091,174.480721905065));
#30838=CARTESIAN_POINT('Ctrl Pts',(31.574734839314,30.2946975726108,174.517765168138));
#30839=CARTESIAN_POINT('Ctrl Pts',(32.1246294353343,30.3358803400799,174.554808431211));
#30840=CARTESIAN_POINT('Ctrl Pts',(32.6745240313545,30.3770631075491,174.591851694284));
#30841=CARTESIAN_POINT('Ctrl Pts',(33.2019872113094,30.7177622803858,174.628894957357));
#30842=CARTESIAN_POINT('Ctrl Pts',(33.4656546841015,31.2020757644642,174.665938220431));
#30843=CARTESIAN_POINT('Ctrl Pts',(33.7293221568936,31.6863892485425,174.702981483504));
#30844=CARTESIAN_POINT('Ctrl Pts',(33.729193922523,32.3143170438626,174.740024746577));
#30845=CARTESIAN_POINT('Ctrl Pts',(33.4653286603423,32.7985227960827,174.77706800965));
#30846=CARTESIAN_POINT('Ctrl Pts',(33.2014633981616,33.2827285483028,174.814111272724));
#30847=CARTESIAN_POINT('Ctrl Pts',(32.6738611081708,33.6232122574229,174.851154535797));
#30848=CARTESIAN_POINT('Ctrl Pts',(32.1239497374654,33.6641704243456,174.88819779887));
#30849=CARTESIAN_POINT('Ctrl Pts',(31.57403836676,33.7051285912683,174.925241061943));
#30850=CARTESIAN_POINT('Ctrl Pts',(31.0018179153401,33.4465612159936,174.962284325017));
#30851=CARTESIAN_POINT('Ctrl Pts',(30.6691333590391,33.0067873274241,174.99932758809));
#30852=CARTESIAN_POINT('Ctrl Pts',(30.4531326430722,32.7212571668096,175.02337851319));
#30853=CARTESIAN_POINT('Ctrl Pts',(30.3381073551171,32.3593401029738,175.04742943829));
#30854=CARTESIAN_POINT('Ctrl Pts',(30.3357235801798,31.9988086992918,175.07148036339));
#30855=CARTESIAN_POINT('Origin',(32.,32.,172.));
#30856=CARTESIAN_POINT('',(30.331418582223,31.9994792732426,175.77148036339));
#30857=CARTESIAN_POINT('',(30.3332690606571,32.0014513847588,175.57851963661));
#30858=CARTESIAN_POINT('',(30.334,32.,172.));
#30859=CARTESIAN_POINT('Ctrl Pts',(30.3332690606571,32.0014513847588,175.57851963661));
#30860=CARTESIAN_POINT('Ctrl Pts',(30.3322967939476,32.1077720140763,175.571400382039));
#30861=CARTESIAN_POINT('Ctrl Pts',(30.3415987476557,32.2139231700336,175.564281127468));
#30862=CARTESIAN_POINT('Ctrl Pts',(30.3617914024463,32.3179605455706,175.557161872896));
#30863=CARTESIAN_POINT('Ctrl Pts',(30.4668588383814,32.8592930450568,175.520118609823));
#30864=CARTESIAN_POINT('Ctrl Pts',(30.8667790797961,33.3433974485404,175.48307534675));
#30865=CARTESIAN_POINT('Ctrl Pts',(31.3785507926964,33.5487502059339,175.446032083677));
#30866=CARTESIAN_POINT('Ctrl Pts',(31.8903225055966,33.7541029633274,175.408988820603));
#30867=CARTESIAN_POINT('Ctrl Pts',(32.5139456899825,33.6807040746309,175.37194555753));
#30868=CARTESIAN_POINT('Ctrl Pts',(32.9640537581348,33.362140473323,175.334902294457));
#30869=CARTESIAN_POINT('Ctrl Pts',(33.4141618262871,33.0435768720152,175.297859031384));
#30870=CARTESIAN_POINT('Ctrl Pts',(33.6907547782058,32.4798485580959,175.260815768311));
#30871=CARTESIAN_POINT('Ctrl Pts',(33.6672651788558,31.9289145513253,175.223772505237));
#30872=CARTESIAN_POINT('Ctrl Pts',(33.6437755795059,31.3779805445546,175.186729242164));
#30873=CARTESIAN_POINT('Ctrl Pts',(33.3202034288872,30.8398408449325,175.149685979091));
#30874=CARTESIAN_POINT('Ctrl Pts',(32.844613588626,30.560745261065,175.112642716018));
#30875=CARTESIAN_POINT('Ctrl Pts',(32.3690237483648,30.2816496771975,175.075599452944));
#30876=CARTESIAN_POINT('Ctrl Pts',(31.7414162184611,30.2615982090847,175.038556189871));
#30877=CARTESIAN_POINT('Ctrl Pts',(31.2489808015386,30.5097662998103,175.001512926798));
#30878=CARTESIAN_POINT('Ctrl Pts',(30.7565453846161,30.757934390536,174.964469663725));
#30879=CARTESIAN_POINT('Ctrl Pts',(30.399282080675,31.2743220401002,174.927426400651));
#30880=CARTESIAN_POINT('Ctrl Pts',(30.340672640419,31.8226330600577,174.890383137578));
#30881=CARTESIAN_POINT('Ctrl Pts',(30.3344158738391,31.8811672151375,174.886428637255));
#30882=CARTESIAN_POINT('Ctrl Pts',(30.3315626632264,31.9400651792653,174.882474136933));
#30883=CARTESIAN_POINT('Ctrl Pts',(30.3319793737621,31.999003930908,174.87851963661));
#30884=CARTESIAN_POINT('Ctrl Pts',(30.3357235801798,31.9988086992918,175.07148036339));
#30885=CARTESIAN_POINT('Ctrl Pts',(30.3344358621602,31.8040492117858,175.084472701363));
#30886=CARTESIAN_POINT('Ctrl Pts',(30.3660188872735,31.6096940838962,175.097465039336));
#30887=CARTESIAN_POINT('Ctrl Pts',(30.4323116977725,31.428003386598,175.11045737731));
#30888=CARTESIAN_POINT('Ctrl Pts',(30.6213232539889,30.9099737362059,175.147500640383));
#30889=CARTESIAN_POINT('Ctrl Pts',(31.0924950276034,30.4948948372859,175.184543903456));
#30890=CARTESIAN_POINT('Ctrl Pts',(31.6302213698328,30.3727045433124,175.221587166529));
#30891=CARTESIAN_POINT('Ctrl Pts',(32.1679477120622,30.250514249339,175.258630429603));
#30892=CARTESIAN_POINT('Ctrl Pts',(32.7722286229063,30.421212560312,175.295673692676));
#30893=CARTESIAN_POINT('Ctrl Pts',(33.1665484341398,30.8066888547031,175.332716955749));
#30894=CARTESIAN_POINT('Ctrl Pts',(33.5608682453733,31.1921651490941,175.369760218822));
#30895=CARTESIAN_POINT('Ctrl Pts',(33.7452269569961,31.7924194269032,175.406803481896));
#30896=CARTESIAN_POINT('Ctrl Pts',(33.6352630222131,32.3327785853487,175.443846744969));
#30897=CARTESIAN_POINT('Ctrl Pts',(33.52529908743,32.8731377437941,175.480890008042));
#30898=CARTESIAN_POINT('Ctrl Pts',(33.1210125062411,33.3536017828761,175.517933271115));
#30899=CARTESIAN_POINT('Ctrl Pts',(32.6074026260459,33.5543129635172,175.554976534188));
#30900=CARTESIAN_POINT('Ctrl Pts',(32.0937927458506,33.7550241441583,175.592019797262));
#30901=CARTESIAN_POINT('Ctrl Pts',(31.470859566649,33.6759824663586,175.629063060335));
#30902=CARTESIAN_POINT('Ctrl Pts',(31.0236539335289,33.3533569732959,175.666106323408));
#30903=CARTESIAN_POINT('Ctrl Pts',(30.5996104381214,33.0474412341954,175.701231003402));
#30904=CARTESIAN_POINT('Ctrl Pts',(30.3335629547701,32.5225201526135,175.736355683396));
#30905=CARTESIAN_POINT('Ctrl Pts',(30.331418582223,31.9994792732426,175.77148036339));
#30906=CARTESIAN_POINT('Origin',(32.,32.,172.));
#30907=CARTESIAN_POINT('',(30.3341900192556,32.0015219962278,176.47148036339));
#30908=CARTESIAN_POINT('',(30.3366800782372,32.0000809155388,176.27851963661));
#30909=CARTESIAN_POINT('',(30.334,32.,172.));
#30910=CARTESIAN_POINT('Ctrl Pts',(30.3366800782372,32.0000809155388,176.27851963661));
#30911=CARTESIAN_POINT('Ctrl Pts',(30.3365617397268,32.2731930172127,176.260326627145));
#30912=CARTESIAN_POINT('Ctrl Pts',(30.4000687460146,32.5462532881901,176.24213361768));
#30913=CARTESIAN_POINT('Ctrl Pts',(30.5275023079567,32.7852240855635,176.223940608215));
#30914=CARTESIAN_POINT('Ctrl Pts',(30.7869731210985,33.2717987850903,176.186897345142));
#30915=CARTESIAN_POINT('Ctrl Pts',(31.3114712794713,33.6170450085694,176.149854082068));
#30916=CARTESIAN_POINT('Ctrl Pts',(31.8609892697898,33.6629799561425,176.112810818995));
#30917=CARTESIAN_POINT('Ctrl Pts',(32.4105072601082,33.7089149037156,176.075767555922));
#30918=CARTESIAN_POINT('Ctrl Pts',(32.9850450823722,33.4555385753826,176.038724292849));
#30919=CARTESIAN_POINT('Ctrl Pts',(33.321697344409,33.0187946051197,176.001681029775));
#30920=CARTESIAN_POINT('Ctrl Pts',(33.6583496064458,32.5820506348568,175.964637766702));
#30921=CARTESIAN_POINT('Ctrl Pts',(33.7571163082553,31.961939022664,175.927594503629));
#30922=CARTESIAN_POINT('Ctrl Pts',(33.5728023426329,31.4422194798622,175.890551240556));
#30923=CARTESIAN_POINT('Ctrl Pts',(33.3884883770104,30.9224999370603,175.853507977482));
#30924=CARTESIAN_POINT('Ctrl Pts',(32.921093743956,30.5031724636493,175.816464714409));
#30925=CARTESIAN_POINT('Ctrl Pts',(32.3844956932118,30.3761190377552,175.779421451336));
#30926=CARTESIAN_POINT('Ctrl Pts',(31.8478976424677,30.2490656118612,175.742378188263));
#30927=CARTESIAN_POINT('Ctrl Pts',(31.2420961740338,30.414286233484,175.705334925189));
#30928=CARTESIAN_POINT('Ctrl Pts',(30.8443027550447,30.7961768420398,175.668291662116));
#30929=CARTESIAN_POINT('Ctrl Pts',(30.522960285069,31.1046728240138,175.638367653614));
#30930=CARTESIAN_POINT('Ctrl Pts',(30.3373557409398,31.5545591738029,175.608443645112));
#30931=CARTESIAN_POINT('Ctrl Pts',(30.3332690606571,32.0014513847588,175.57851963661));
#30932=CARTESIAN_POINT('Ctrl Pts',(30.331418582223,31.9994792732426,175.77148036339));
#30933=CARTESIAN_POINT('Ctrl Pts',(30.3313014521343,31.9709096925072,175.773398946469));
#30934=CARTESIAN_POINT('Ctrl Pts',(30.3319716958771,31.9423457214897,175.775317529549));
#30935=CARTESIAN_POINT('Ctrl Pts',(30.3334465730137,31.9138233576617,175.777236112628));
#30936=CARTESIAN_POINT('Ctrl Pts',(30.3619229326574,31.363124543416,175.814279375701));
#30937=CARTESIAN_POINT('Ctrl Pts',(30.6903537389835,30.8279362232504,175.851322638774));
#30938=CARTESIAN_POINT('Ctrl Pts',(31.1684508358577,30.5531576705442,175.888365901848));
#30939=CARTESIAN_POINT('Ctrl Pts',(31.6465479327319,30.278379117838,175.925409164921));
#30940=CARTESIAN_POINT('Ctrl Pts',(32.2743113201543,30.2640103325911,175.962452427994));
#30941=CARTESIAN_POINT('Ctrl Pts',(32.7644798759482,30.5166263930021,175.999495691067));
#30942=CARTESIAN_POINT('Ctrl Pts',(33.2546484317422,30.7692424534132,176.036538954141));
#30943=CARTESIAN_POINT('Ctrl Pts',(33.6072221559078,31.2888433594821,176.073582217214));
#30944=CARTESIAN_POINT('Ctrl Pts',(33.6608652240127,31.8376625540489,176.110625480287));
#30945=CARTESIAN_POINT('Ctrl Pts',(33.7145082921176,32.3864817486158,176.14766874336));
#30946=CARTESIAN_POINT('Ctrl Pts',(33.4692207041618,32.9645192316805,176.184712006434));
#30947=CARTESIAN_POINT('Ctrl Pts',(33.0372447303886,33.307268185192,176.221755269507));
#30948=CARTESIAN_POINT('Ctrl Pts',(32.6052687566154,33.6500171387034,176.25879853258));
#30949=CARTESIAN_POINT('Ctrl Pts',(31.9866043970249,33.7574775626615,176.295841795653));
#30950=CARTESIAN_POINT('Ctrl Pts',(31.4643491079747,33.5804761499029,176.332885058727));
#30951=CARTESIAN_POINT('Ctrl Pts',(30.9420938189246,33.4034747371442,176.3699283218));
#30952=CARTESIAN_POINT('Ctrl Pts',(30.5162476004149,32.9420114876688,176.406971584873));
#30953=CARTESIAN_POINT('Ctrl Pts',(30.3816753730276,32.4072494819308,176.444014847946));
#30954=CARTESIAN_POINT('Ctrl Pts',(30.3484161037031,32.2750840721826,176.453170019761));
#30955=CARTESIAN_POINT('Ctrl Pts',(30.3329484846486,32.138441414632,176.462325191576));
#30956=CARTESIAN_POINT('Ctrl Pts',(30.3341900192556,32.0015219962278,176.47148036339));
#30957=CARTESIAN_POINT('Origin',(32.,32.,172.));
#30958=CARTESIAN_POINT('',(30.3365877314637,31.9995845740104,177.17148036339));
#30959=CARTESIAN_POINT('',(30.3335660066275,31.9985061125779,176.97851963661));
#30960=CARTESIAN_POINT('',(30.334,32.,172.));
#30961=CARTESIAN_POINT('Ctrl Pts',(30.3335660066275,31.9985061125779,176.97851963661));
#30962=CARTESIAN_POINT('Ctrl Pts',(30.3376018361009,32.4357833033998,176.949252872251));
#30963=CARTESIAN_POINT('Ctrl Pts',(30.5142836011723,32.8759469172232,176.919986107892));
#30964=CARTESIAN_POINT('Ctrl Pts',(30.8231793229629,33.1831819008459,176.890719343533));
#30965=CARTESIAN_POINT('Ctrl Pts',(31.2141520093921,33.5720525728505,176.85367608046));
#30966=CARTESIAN_POINT('Ctrl Pts',(31.8169346432747,33.7479683732478,176.816632817387));
#30967=CARTESIAN_POINT('Ctrl Pts',(32.3556971607286,33.6304311846374,176.779589554313));
#30968=CARTESIAN_POINT('Ctrl Pts',(32.8944596781825,33.5128939960271,176.74254629124));
#30969=CARTESIAN_POINT('Ctrl Pts',(33.3692020792077,33.1019038184092,176.705503028167));
#30970=CARTESIAN_POINT('Ctrl Pts',(33.5626848148218,32.5855275290525,176.668459765094));
#30971=CARTESIAN_POINT('Ctrl Pts',(33.7561675504359,32.0691512396958,176.63141650202));
#30972=CARTESIAN_POINT('Ctrl Pts',(33.6683906206388,31.4473888386002,176.594373238947));
#30973=CARTESIAN_POINT('Ctrl Pts',(33.3395202727796,31.0047554288992,176.557329975874));
#30974=CARTESIAN_POINT('Ctrl Pts',(33.0106499249203,30.5621220191981,176.520286712801));
#30975=CARTESIAN_POINT('Ctrl Pts',(32.4406861589989,30.2986176008915,176.483243449727));
#30976=CARTESIAN_POINT('Ctrl Pts',(31.8904413036908,30.3348203671221,176.446200186654));
#30977=CARTESIAN_POINT('Ctrl Pts',(31.3401964483828,30.3710231333526,176.409156923581));
#30978=CARTESIAN_POINT('Ctrl Pts',(30.8096705036882,30.7069330841203,176.372113660508));
#30979=CARTESIAN_POINT('Ctrl Pts',(30.5416292652962,31.1888396472913,176.335070397435));
#30980=CARTESIAN_POINT('Ctrl Pts',(30.4052307706181,31.4340680688071,176.316220143826));
#30981=CARTESIAN_POINT('Ctrl Pts',(30.3368026918674,31.717102313789,176.297369890218));
#30982=CARTESIAN_POINT('Ctrl Pts',(30.3366800782372,32.0000809155388,176.27851963661));
#30983=CARTESIAN_POINT('Ctrl Pts',(30.3341900192556,32.0015219962278,176.47148036339));
#30984=CARTESIAN_POINT('Ctrl Pts',(30.3379719286637,31.5844439432072,176.499368454649));
#30985=CARTESIAN_POINT('Ctrl Pts',(30.4967992918917,31.1647978060687,176.527256545907));
#30986=CARTESIAN_POINT('Ctrl Pts',(30.7800747867322,30.8613125042108,176.555144637166));
#30987=CARTESIAN_POINT('Ctrl Pts',(31.1563446640889,30.4581982942296,176.592187900239));
#30988=CARTESIAN_POINT('Ctrl Pts',(31.7521826550671,30.2600306362681,176.629231163313));
#30989=CARTESIAN_POINT('Ctrl Pts',(32.294936525987,30.3574899747402,176.666274426386));
#30990=CARTESIAN_POINT('Ctrl Pts',(32.8376903969068,30.4549493132123,176.703317689459));
#30991=CARTESIAN_POINT('Ctrl Pts',(33.3273601477684,30.8480356481179,176.740360952532));
#30992=CARTESIAN_POINT('Ctrl Pts',(33.5398755553043,31.3568748067747,176.777404215605));
#30993=CARTESIAN_POINT('Ctrl Pts',(33.7523909628403,31.8657139654314,176.814447478679));
#30994=CARTESIAN_POINT('Ctrl Pts',(33.6877520270506,32.4903059478392,176.851490741752));
#30995=CARTESIAN_POINT('Ctrl Pts',(33.3755371752704,32.9448408439612,176.888534004825));
#30996=CARTESIAN_POINT('Ctrl Pts',(33.0633223234901,33.3993757400832,176.925577267898));
#30997=CARTESIAN_POINT('Ctrl Pts',(32.5035315557193,33.6838535499193,176.962620530972));
#30998=CARTESIAN_POINT('Ctrl Pts',(31.9523220903062,33.6680987815996,176.999663794045));
#30999=CARTESIAN_POINT('Ctrl Pts',(31.4011126248931,33.65234401328,177.036707057118));
#31000=CARTESIAN_POINT('Ctrl Pts',(30.8584844618377,33.3363566668047,177.073750320191));
#31001=CARTESIAN_POINT('Ctrl Pts',(30.5727413096241,32.86473081535,177.110793583265));
#31002=CARTESIAN_POINT('Ctrl Pts',(30.4167000539667,32.6071810210981,177.131022509973));
#31003=CARTESIAN_POINT('Ctrl Pts',(30.3372653606356,32.3032177331473,177.151251436682));
#31004=CARTESIAN_POINT('Ctrl Pts',(30.3365877314637,31.9995845740104,177.17148036339));
#31005=CARTESIAN_POINT('Origin',(32.,32.,172.));
#31006=CARTESIAN_POINT('',(30.3326674383851,31.998696643609,177.87148036339));
#31007=CARTESIAN_POINT('',(30.3317667672262,32.0008552724323,177.67851963661));
#31008=CARTESIAN_POINT('',(30.334,32.,172.));
#31009=CARTESIAN_POINT('Ctrl Pts',(30.3317667672262,32.0008552724323,177.67851963661));
#31010=CARTESIAN_POINT('Ctrl Pts',(30.3314592141136,32.0499818232188,177.67522238043));
#31011=CARTESIAN_POINT('Ctrl Pts',(30.3334412206569,32.0990832080451,177.671925124251));
#31012=CARTESIAN_POINT('Ctrl Pts',(30.3377935532569,32.1479735799601,177.668627868071));
#31013=CARTESIAN_POINT('Ctrl Pts',(30.3866901486996,32.6972359999809,177.631584604998));
#31014=CARTESIAN_POINT('Ctrl Pts',(30.7347589067126,33.2198652954923,177.594541341925));
#31015=CARTESIAN_POINT('Ctrl Pts',(31.22272531614,33.4767092800123,177.557498078852));
#31016=CARTESIAN_POINT('Ctrl Pts',(31.7106917255674,33.7335532645324,177.520454815778));
#31017=CARTESIAN_POINT('Ctrl Pts',(32.3385557864092,33.724611938061,177.483411552705));
#31018=CARTESIAN_POINT('Ctrl Pts',(32.8190103750928,33.4539767317386,177.446368289632));
#31019=CARTESIAN_POINT('Ctrl Pts',(33.2994649637764,33.1833415254162,177.409325026559));
#31020=CARTESIAN_POINT('Ctrl Pts',(33.6325100803019,32.6510124392426,177.372281763485));
#31021=CARTESIAN_POINT('Ctrl Pts',(33.6657460526844,32.1005804116725,177.335238500412));
#31022=CARTESIAN_POINT('Ctrl Pts',(33.698982025067,31.5501483841025,177.298195237339));
#31023=CARTESIAN_POINT('Ctrl Pts',(33.4324088533065,30.9816134151359,177.261151974266));
#31024=CARTESIAN_POINT('Ctrl Pts',(32.9880089913433,30.6551340066007,177.224108711192));
#31025=CARTESIAN_POINT('Ctrl Pts',(32.5436091293801,30.3286545980654,177.187065448119));
#31026=CARTESIAN_POINT('Ctrl Pts',(31.9213825772142,30.2442307499615,177.150022185046));
#31027=CARTESIAN_POINT('Ctrl Pts',(31.4060568233868,30.4404943658696,177.112978921973));
#31028=CARTESIAN_POINT('Ctrl Pts',(30.8907310695595,30.6367579817777,177.075935658899));
#31029=CARTESIAN_POINT('Ctrl Pts',(30.4823061140706,31.1137090616976,177.038892395826));
#31030=CARTESIAN_POINT('Ctrl Pts',(30.3676750058142,31.6530973734636,177.001849132753));
#31031=CARTESIAN_POINT('Ctrl Pts',(30.3436104771516,31.7663312563613,176.994072634039));
#31032=CARTESIAN_POINT('Ctrl Pts',(30.3324936426885,31.8823167904328,176.986296135324));
#31033=CARTESIAN_POINT('Ctrl Pts',(30.3335660066275,31.9985061125779,176.97851963661));
#31034=CARTESIAN_POINT('Ctrl Pts',(30.3365877314637,31.9995845740104,177.17148036339));
#31035=CARTESIAN_POINT('Ctrl Pts',(30.336024484338,31.7472039043504,177.188294699755));
#31036=CARTESIAN_POINT('Ctrl Pts',(30.3898743158847,31.4950513199463,177.20510903612));
#31037=CARTESIAN_POINT('Ctrl Pts',(30.4993722077054,31.2699705615928,177.221923372484));
#31038=CARTESIAN_POINT('Ctrl Pts',(30.740604399372,30.7741005157242,177.258966635558));
#31039=CARTESIAN_POINT('Ctrl Pts',(31.2519269240771,30.4096247804211,177.296009898631));
#31040=CARTESIAN_POINT('Ctrl Pts',(31.7993613809296,30.3433253796834,177.333053161704));
#31041=CARTESIAN_POINT('Ctrl Pts',(32.3467958377822,30.2770259789457,177.370096424777));
#31042=CARTESIAN_POINT('Ctrl Pts',(32.9303422267822,30.5089029127736,177.407139687851));
#31043=CARTESIAN_POINT('Ctrl Pts',(33.2829728562038,30.9328507493989,177.444182950924));
#31044=CARTESIAN_POINT('Ctrl Pts',(33.6356034856253,31.3567985860242,177.481226213997));
#31045=CARTESIAN_POINT('Ctrl Pts',(33.7573183554684,31.972817325447,177.51826947707));
#31046=CARTESIAN_POINT('Ctrl Pts',(33.5924214588221,32.4990197339482,177.555312740144));
#31047=CARTESIAN_POINT('Ctrl Pts',(33.4275245621758,33.0252221424493,177.592356003217));
#31048=CARTESIAN_POINT('Ctrl Pts',(32.9760158990401,33.4616082200288,177.62939926629));
#31049=CARTESIAN_POINT('Ctrl Pts',(32.444503268266,33.6084908757691,177.666442529363));
#31050=CARTESIAN_POINT('Ctrl Pts',(31.9129906374918,33.7553735315094,177.703485792436));
#31051=CARTESIAN_POINT('Ctrl Pts',(31.3014740390791,33.6127527654104,177.74052905551));
#31052=CARTESIAN_POINT('Ctrl Pts',(30.8897803912795,33.2458894134051,177.777572318583));
#31053=CARTESIAN_POINT('Ctrl Pts',(30.5418867635142,32.935878746237,177.808875000185));
#31054=CARTESIAN_POINT('Ctrl Pts',(30.3366819678508,32.4657417642871,177.840177681788));
#31055=CARTESIAN_POINT('Ctrl Pts',(30.3326674383851,31.998696643609,177.87148036339));
#31056=CARTESIAN_POINT('Origin',(32.,32.,172.));
#31057=CARTESIAN_POINT('',(30.3325025488117,32.0012179414303,178.57148036339));
#31058=CARTESIAN_POINT('',(30.3361333853116,32.0009462961084,178.37851963661));
#31059=CARTESIAN_POINT('',(30.334,32.,172.));
#31060=CARTESIAN_POINT('',(33.2690708798533,33.0793586530475,179.));
#31061=CARTESIAN_POINT('Ctrl Pts',(30.3325025488117,32.0012179414303,178.57148036339));
#31062=CARTESIAN_POINT('Ctrl Pts',(30.3364292156548,31.5283160549018,178.60319045304));
#31063=CARTESIAN_POINT('Ctrl Pts',(30.5476330207047,31.0524199115449,178.634900542691));
#31064=CARTESIAN_POINT('Ctrl Pts',(30.9034954080308,30.7421389970656,178.666610632341));
#31065=CARTESIAN_POINT('Ctrl Pts',(31.3192086455844,30.3796733696121,178.703653895414));
#31066=CARTESIAN_POINT('Ctrl Pts',(31.9323312413379,30.243215736475,178.740697158487));
#31067=CARTESIAN_POINT('Ctrl Pts',(32.4621594780356,30.3962147962734,178.777740421561));
#31068=CARTESIAN_POINT('Ctrl Pts',(32.9919877147334,30.5492138560719,178.814783684634));
#31069=CARTESIAN_POINT('Ctrl Pts',(33.4385215923753,30.9916696088058,178.851826947707));
#31070=CARTESIAN_POINT('Ctrl Pts',(33.5975139507523,31.518714433356,178.88887021078));
#31071=CARTESIAN_POINT('Ctrl Pts',(33.7565063091292,32.0457592579062,178.925913473853));
#31072=CARTESIAN_POINT('Ctrl Pts',(33.6279571482411,32.6573931542727,178.962956736927));
#31073=CARTESIAN_POINT('Ctrl Pts',(33.2690708798531,33.0793586530476,179.));
#31074=CARTESIAN_POINT('',(30.72851190076,33.0811958771907,179.));
#31075=CARTESIAN_POINT('Origin',(32.,32.,179.));
#31076=CARTESIAN_POINT('Ctrl Pts',(30.7285100828332,33.0811972589182,179.));
#31077=CARTESIAN_POINT('Ctrl Pts',(31.0792913246103,33.4926026794485,178.963685183163));
#31078=CARTESIAN_POINT('Ctrl Pts',(31.6490955279031,33.7187060371509,178.927370366326));
#31079=CARTESIAN_POINT('Ctrl Pts',(32.1864012108571,33.658249220712,178.891055549488));
#31080=CARTESIAN_POINT('Ctrl Pts',(32.7344848168854,33.5965796887974,178.854012286415));
#31081=CARTESIAN_POINT('Ctrl Pts',(33.2487530373446,33.2367383424031,178.816969023342));
#31082=CARTESIAN_POINT('Ctrl Pts',(33.4942155657675,32.7430232864054,178.779925760269));
#31083=CARTESIAN_POINT('Ctrl Pts',(33.7396780941904,32.2493082304078,178.742882497195));
#31084=CARTESIAN_POINT('Ctrl Pts',(33.716334930577,31.6217194648069,178.705839234122));
#31085=CARTESIAN_POINT('Ctrl Pts',(33.4347028183851,31.1476160413552,178.668795971049));
#31086=CARTESIAN_POINT('Ctrl Pts',(33.1530707061932,30.6735126179035,178.631752707976));
#31087=CARTESIAN_POINT('Ctrl Pts',(32.6131496454229,30.352894536601,178.594709444902));
#31088=CARTESIAN_POINT('Ctrl Pts',(32.0620856027671,30.3323875673963,178.557666181829));
#31089=CARTESIAN_POINT('Ctrl Pts',(31.5110215601112,30.3118805981917,178.520622918756));
#31090=CARTESIAN_POINT('Ctrl Pts',(30.9488145355698,30.5914847410848,178.483579655683));
#31091=CARTESIAN_POINT('Ctrl Pts',(30.6326876217354,31.0432975466902,178.446536392609));
#31092=CARTESIAN_POINT('Ctrl Pts',(30.4392028026414,31.319828633198,178.42386414061));
#31093=CARTESIAN_POINT('Ctrl Pts',(30.3379002457712,31.6608695415591,178.40119188861));
#31094=CARTESIAN_POINT('Ctrl Pts',(30.3361333853116,32.0009462961084,178.37851963661));
#31095=CARTESIAN_POINT('Origin',(32.,32.,180.545925280538));
#31096=CARTESIAN_POINT('',(29.9466856106202,32.0018139367885,166.254074719462));
#31097=CARTESIAN_POINT('',(29.9453305521271,31.9981395289548,166.195925280538));
#31098=CARTESIAN_POINT('',(29.94525,32.0000000000002,180.545925280538));
#31099=CARTESIAN_POINT('',(32.3836679988478,34.0186125009917,166.));
#31100=CARTESIAN_POINT('Ctrl Pts',(29.9453305521271,31.9981395289548,166.195925280538));
#31101=CARTESIAN_POINT('Ctrl Pts',(29.9505790914998,32.5195345061705,166.167660116765));
#31102=CARTESIAN_POINT('Ctrl Pts',(30.4181723873308,33.7318542488392,166.102351689919));
#31103=CARTESIAN_POINT('Ctrl Pts',(31.7124802469762,34.1461819386551,166.037043263073));
#31104=CARTESIAN_POINT('Ctrl Pts',(32.3836679988478,34.0186125009917,166.));
#31105=CARTESIAN_POINT('',(33.3415940970262,33.5612502368267,166.));
#31106=CARTESIAN_POINT('Origin',(32.,32.,166.));
#31107=CARTESIAN_POINT('Ctrl Pts',(29.9466856106202,32.0018139367885,166.254074719462));
#31108=CARTESIAN_POINT('Ctrl Pts',(29.9450188939236,32.21116652697,166.242741226219));
#31109=CARTESIAN_POINT('Ctrl Pts',(30.0707146480112,33.1027772339307,166.194364469902));
#31110=CARTESIAN_POINT('Ctrl Pts',(31.3452942359773,34.3307277928868,166.109672896748));
#31111=CARTESIAN_POINT('Ctrl Pts',(32.8352805948106,33.9951595674105,166.036314816837));
#31112=CARTESIAN_POINT('Ctrl Pts',(33.3415960466846,33.561252269086,166.));
#31113=CARTESIAN_POINT('Origin',(32.,32.,180.545925280538));
#31114=CARTESIAN_POINT('',(29.9479603212001,31.9988941585155,166.954074719462));
#31115=CARTESIAN_POINT('',(29.9421602766058,32.0007586547802,166.895925280538));
#31116=CARTESIAN_POINT('',(29.94525,32.0000000000002,180.545925280538));
#31117=CARTESIAN_POINT('Ctrl Pts',(29.9421602766058,32.0007586547802,166.895925280538));
#31118=CARTESIAN_POINT('Ctrl Pts',(29.9419599928232,32.0429254387486,166.893629624944));
#31119=CARTESIAN_POINT('Ctrl Pts',(29.9622502782122,32.7653095976581,166.854290706278));
#31120=CARTESIAN_POINT('Ctrl Pts',(30.8113032934655,34.1178215046619,166.777908524538));
#31121=CARTESIAN_POINT('Ctrl Pts',(33.1343552393677,34.1473557540512,166.666778735318));
#31122=CARTESIAN_POINT('Ctrl Pts',(34.4195276894793,32.2117592010123,166.555648946099));
#31123=CARTESIAN_POINT('Ctrl Pts',(33.4898246183641,30.0821472766194,166.444519156879));
#31124=CARTESIAN_POINT('Ctrl Pts',(31.1977703849704,29.7081726882415,166.333389367659));
#31125=CARTESIAN_POINT('Ctrl Pts',(30.034435938876,30.9926242945928,166.250524742212));
#31126=CARTESIAN_POINT('Ctrl Pts',(29.943700552734,31.8362138128461,166.204703379838));
#31127=CARTESIAN_POINT('Ctrl Pts',(29.9453305521271,31.9981395289548,166.195925280538));
#31128=CARTESIAN_POINT('Ctrl Pts',(29.9479603212001,31.9988941585155,166.954074719462));
#31129=CARTESIAN_POINT('Ctrl Pts',(29.9499871753085,32.4134609401804,166.931667471325));
#31130=CARTESIAN_POINT('Ctrl Pts',(30.2732187069358,33.5162878102792,166.872216960114));
#31131=CARTESIAN_POINT('Ctrl Pts',(32.073044548561,34.4275128335807,166.77572318583));
#31132=CARTESIAN_POINT('Ctrl Pts',(34.0790345884103,33.255346086573,166.66459339661));
#31133=CARTESIAN_POINT('Ctrl Pts',(34.1822756467128,30.9342420768624,166.553463607391));
#31134=CARTESIAN_POINT('Ctrl Pts',(32.2884012470789,29.5886265247524,166.442333818171));
#31135=CARTESIAN_POINT('Ctrl Pts',(30.3505030706617,30.3618237232923,166.342537522195));
#31136=CARTESIAN_POINT('Ctrl Pts',(29.9504665192701,31.5269023811822,166.279784489292));
#31137=CARTESIAN_POINT('Ctrl Pts',(29.9466856106202,32.0018139367885,166.254074719462));
#31138=CARTESIAN_POINT('Origin',(32.,32.,180.545925280538));
#31139=CARTESIAN_POINT('',(29.9425974682135,31.9988731389439,167.654074719462));
#31140=CARTESIAN_POINT('',(29.9475247189157,32.0013942611211,167.595925280538));
#31141=CARTESIAN_POINT('',(29.94525,32.0000000000002,180.545925280538));
#31142=CARTESIAN_POINT('Ctrl Pts',(29.9475247189157,32.0013942611211,167.595925280538));
#31143=CARTESIAN_POINT('Ctrl Pts',(29.9459809856321,32.2486160756999,167.582555870051));
#31144=CARTESIAN_POINT('Ctrl Pts',(30.1017580865117,33.1789472430918,167.53214319649));
#31145=CARTESIAN_POINT('Ctrl Pts',(31.4859258624946,34.3735884913369,167.444687259856));
#31146=CARTESIAN_POINT('Ctrl Pts',(33.7152536393985,33.7193295360918,167.333557470637));
#31147=CARTESIAN_POINT('Ctrl Pts',(34.3748036771893,31.4915603207829,167.222427681417));
#31148=CARTESIAN_POINT('Ctrl Pts',(32.8609514252531,29.7291065603519,167.111297892197));
#31149=CARTESIAN_POINT('Ctrl Pts',(30.606730126964,30.0384313727369,167.002463758571));
#31150=CARTESIAN_POINT('Ctrl Pts',(29.9451918211818,31.3625118453315,166.930672888018));
#31151=CARTESIAN_POINT('Ctrl Pts',(29.9421602766058,32.0007586547802,166.895925280538));
#31152=CARTESIAN_POINT('Ctrl Pts',(29.9425974682135,31.9988731389439,167.654074719462));
#31153=CARTESIAN_POINT('Ctrl Pts',(29.9466607983974,32.6141954522381,167.620593716431));
#31154=CARTESIAN_POINT('Ctrl Pts',(30.5667381595166,33.9174120322558,167.550069450326));
#31155=CARTESIAN_POINT('Ctrl Pts',(32.7830165295865,34.2989296881618,167.442501921148));
#31156=CARTESIAN_POINT('Ctrl Pts',(34.3560823145915,32.5891267546308,167.331372131929));
#31157=CARTESIAN_POINT('Ctrl Pts',(33.7728865672594,30.3401605876776,167.220242342709));
#31158=CARTESIAN_POINT('Ctrl Pts',(31.5671653767747,29.6102631127892,167.109112553489));
#31159=CARTESIAN_POINT('Ctrl Pts',(30.1224391142159,30.7736143308135,167.020390012407));
#31160=CARTESIAN_POINT('Ctrl Pts',(29.9466364162377,31.7281065289479,166.968710734398));
#31161=CARTESIAN_POINT('Ctrl Pts',(29.9479603212001,31.9988941585155,166.954074719462));
#31162=CARTESIAN_POINT('Origin',(32.,32.,180.545925280538));
#31163=CARTESIAN_POINT('',(29.9445665862919,32.0018241253517,168.354074719462));
#31164=CARTESIAN_POINT('',(29.9472120516653,31.998458524753,168.295925280538));
#31165=CARTESIAN_POINT('',(29.94525,32.0000000000002,180.545925280538));
#31166=CARTESIAN_POINT('Ctrl Pts',(29.9472120516653,31.998458524753,168.295925280538));
#31167=CARTESIAN_POINT('Ctrl Pts',(29.9503631280156,32.4502786971803,168.271482115157));
#31168=CARTESIAN_POINT('Ctrl Pts',(30.3199260724322,33.5915112303712,168.209995686702));
#31169=CARTESIAN_POINT('Ctrl Pts',(32.2059575727712,34.4198709905092,168.111465995175));
#31170=CARTESIAN_POINT('Ctrl Pts',(34.1446869293352,33.1395227135096,168.000336205955));
#31171=CARTESIAN_POINT('Ctrl Pts',(34.1206221195246,30.8162956275684,167.889206416735));
#31172=CARTESIAN_POINT('Ctrl Pts',(32.1557868348082,29.5763819040772,167.778076627516));
#31173=CARTESIAN_POINT('Ctrl Pts',(30.3019081319035,30.4368608022391,167.680316248783));
#31174=CARTESIAN_POINT('Ctrl Pts',(29.9502582810442,31.5636268068268,167.619599133124));
#31175=CARTESIAN_POINT('Ctrl Pts',(29.9475247189157,32.0013942611211,167.595925280538));
#31176=CARTESIAN_POINT('Ctrl Pts',(29.9445665862919,32.0018241253517,168.354074719462));
#31177=CARTESIAN_POINT('Ctrl Pts',(29.9432922113974,32.1402164550963,168.34656322461));
#31178=CARTESIAN_POINT('Ctrl Pts',(30.0191193705774,32.9597079858832,168.302008466685));
#31179=CARTESIAN_POINT('Ctrl Pts',(31.1194450837624,34.2633639270065,168.220410445687));
#31180=CARTESIAN_POINT('Ctrl Pts',(33.4238724584211,33.9674299065165,168.109280656467));
#31181=CARTESIAN_POINT('Ctrl Pts',(34.4251872041711,31.8709253771026,167.998150867247));
#31182=CARTESIAN_POINT('Ctrl Pts',(33.206996913019,29.8925485313441,167.887021078027));
#31183=CARTESIAN_POINT('Ctrl Pts',(30.8841761520946,29.8428884386802,167.775891288808));
#31184=CARTESIAN_POINT('Ctrl Pts',(29.9746984974497,31.187581664638,167.698242502619));
#31185=CARTESIAN_POINT('Ctrl Pts',(29.9421651442853,31.9334050259535,167.657636979504));
#31186=CARTESIAN_POINT('Ctrl Pts',(29.9425974682135,31.9988731389439,167.654074719462));
#31187=CARTESIAN_POINT('Origin',(32.,32.,180.545925280538));
#31188=CARTESIAN_POINT('',(29.9485596886742,31.9999806718114,169.054074719462));
#31189=CARTESIAN_POINT('',(29.9419793320997,31.9994845592423,168.995925280538));
#31190=CARTESIAN_POINT('',(29.94525,32.0000000000002,180.545925280538));
#31191=CARTESIAN_POINT('Ctrl Pts',(29.9419793320997,31.9994845592423,168.995925280538));
#31192=CARTESIAN_POINT('Ctrl Pts',(29.9441754476556,32.6517037695688,168.960408360263));
#31193=CARTESIAN_POINT('Ctrl Pts',(30.6316772116244,33.9881562660024,168.887848176915));
#31194=CARTESIAN_POINT('Ctrl Pts',(32.9078114849742,34.2525701817925,168.778244730493));
#31195=CARTESIAN_POINT('Ctrl Pts',(34.384824085665,32.4591385359132,168.667114941273));
#31196=CARTESIAN_POINT('Ctrl Pts',(33.6792715462419,30.2455082814088,168.555985152054));
#31197=CARTESIAN_POINT('Ctrl Pts',(31.43686789712,29.6375698204928,168.444855362834));
#31198=CARTESIAN_POINT('Ctrl Pts',(30.0896997832934,30.8498681507073,168.358168738995));
#31199=CARTESIAN_POINT('Ctrl Pts',(29.9455877174504,31.7655517705286,168.30852537823));
#31200=CARTESIAN_POINT('Ctrl Pts',(29.9472120516653,31.998458524753,168.295925280538));
#31201=CARTESIAN_POINT('Ctrl Pts',(29.9485596886742,31.9999806718114,169.054074719462));
#31202=CARTESIAN_POINT('Ctrl Pts',(29.9485885621676,32.3440857065745,169.035489469716));
#31203=CARTESIAN_POINT('Ctrl Pts',(30.1937796180674,33.3740837021047,168.979860956897));
#31204=CARTESIAN_POINT('Ctrl Pts',(31.8232672732892,34.4221805810845,168.887189181005));
#31205=CARTESIAN_POINT('Ctrl Pts',(33.9390539828564,33.4622800263533,168.776059391785));
#31206=CARTESIAN_POINT('Ctrl Pts',(34.2802395155314,31.1641166493491,168.664929602565));
#31207=CARTESIAN_POINT('Ctrl Pts',(32.5345745716517,29.6309446499222,168.553799813346));
#31208=CARTESIAN_POINT('Ctrl Pts',(30.4507344632293,30.2229880222625,168.450181518978));
#31209=CARTESIAN_POINT('Ctrl Pts',(29.9495768465332,31.4577286708363,168.383606487683));
#31210=CARTESIAN_POINT('Ctrl Pts',(29.9445665862919,32.0018241253517,168.354074719462));
#31211=CARTESIAN_POINT('Origin',(32.,32.,180.545925280538));
#31212=CARTESIAN_POINT('',(29.9444956521926,31.9981860244656,169.754074719462));
#31213=CARTESIAN_POINT('',(29.945699695435,32.0018685376852,169.695925280538));
#31214=CARTESIAN_POINT('',(29.94525,32.0000000000002,180.545925280538));
#31215=CARTESIAN_POINT('Ctrl Pts',(29.945699695435,32.0018685376852,169.695925280538));
#31216=CARTESIAN_POINT('Ctrl Pts',(29.944124321843,32.1780191762476,169.686377868442));
#31217=CARTESIAN_POINT('Ctrl Pts',(30.045488237746,33.0358359740345,169.639787193273));
#31218=CARTESIAN_POINT('Ctrl Pts',(31.2447903468041,34.3082141355403,169.556153255031));
#31219=CARTESIAN_POINT('Ctrl Pts',(33.5295398276061,33.8864522341055,169.445023465811));
#31220=CARTESIAN_POINT('Ctrl Pts',(34.4144710453466,31.738229705738,169.333893676592));
#31221=CARTESIAN_POINT('Ctrl Pts',(33.0897045462445,29.8295765119025,169.222763887372));
#31222=CARTESIAN_POINT('Ctrl Pts',(30.7676522637518,29.9072713571029,169.111634098153));
#31223=CARTESIAN_POINT('Ctrl Pts',(29.9551025731251,31.2632688429224,169.036021229208));
#31224=CARTESIAN_POINT('Ctrl Pts',(29.9418849538389,31.9714553808426,168.997451623336));
#31225=CARTESIAN_POINT('Ctrl Pts',(29.9419793320997,31.9994845592423,168.995925280538));
#31226=CARTESIAN_POINT('Ctrl Pts',(29.9444956521925,31.9981860244657,169.754074719462));
#31227=CARTESIAN_POINT('Ctrl Pts',(29.949518107583,32.5445771748198,169.724415714823));
#31228=CARTESIAN_POINT('Ctrl Pts',(30.454270674604,33.7815914342631,169.65771344711));
#31229=CARTESIAN_POINT('Ctrl Pts',(32.5426883094078,34.3672098814547,169.553967916323));
#31230=CARTESIAN_POINT('Ctrl Pts',(34.2830900415719,32.8280658706275,169.442838127104));
#31231=CARTESIAN_POINT('Ctrl Pts',(33.9340325267706,30.5310849550035,169.331708337884));
#31232=CARTESIAN_POINT('Ctrl Pts',(31.8149694171768,29.5784391588377,169.220578548664));
#31233=CARTESIAN_POINT('Ctrl Pts',(30.1913146327685,30.6306661769337,169.12803400919));
#31234=CARTESIAN_POINT('Ctrl Pts',(29.9485310128515,31.6582314134216,169.07253273279));
#31235=CARTESIAN_POINT('Ctrl Pts',(29.9485596886742,31.9999806718114,169.054074719462));
#31236=CARTESIAN_POINT('Origin',(32.,32.,180.545925280538));
#31237=CARTESIAN_POINT('',(29.9426482690414,32.0011604961315,170.454074719462));
#31238=CARTESIAN_POINT('',(29.9483814718272,31.9993739362355,170.395925280538));
#31239=CARTESIAN_POINT('',(29.94525,32.0000000000002,180.545925280538));
#31240=CARTESIAN_POINT('Ctrl Pts',(29.9483814718272,31.9993739362354,170.395925280538));
#31241=CARTESIAN_POINT('Ctrl Pts',(29.9494242471388,32.3810912191388,170.375304113548));
#31242=CARTESIAN_POINT('Ctrl Pts',(30.2347805600279,33.4499627199415,170.317639683485));
#31243=CARTESIAN_POINT('Ctrl Pts',(31.9562576159421,34.4282258378547,170.22293199035));
#31244=CARTESIAN_POINT('Ctrl Pts',(34.0162673880548,33.3538315758082,170.11180220113));
#31245=CARTESIAN_POINT('Ctrl Pts',(34.2310111121289,31.0404253372741,170.00067241191));
#31246=CARTESIAN_POINT('Ctrl Pts',(32.4039576606909,29.6052114239129,169.88954262269));
#31247=CARTESIAN_POINT('Ctrl Pts',(30.3959344072883,30.2966919391978,169.787960245566));
#31248=CARTESIAN_POINT('Ctrl Pts',(29.9502366565598,31.494567537263,169.723421131515));
#31249=CARTESIAN_POINT('Ctrl Pts',(29.945699695435,32.0018685376852,169.695925280538));
#31250=CARTESIAN_POINT('Ctrl Pts',(29.9426482690414,32.0011604961315,170.454074719462));
#31251=CARTESIAN_POINT('Ctrl Pts',(29.9421898451266,32.068971401295,170.450385223002));
#31252=CARTESIAN_POINT('Ctrl Pts',(29.9759960847807,32.8171543406774,170.409652463468));
#31253=CARTESIAN_POINT('Ctrl Pts',(30.8915734045388,34.1609219575215,170.331876440861));
#31254=CARTESIAN_POINT('Ctrl Pts',(33.2142103990771,34.1033036706089,170.220746651642));
#31255=CARTESIAN_POINT('Ctrl Pts',(34.4256152039436,32.1207646737337,170.109616862422));
#31256=CARTESIAN_POINT('Ctrl Pts',(33.4171232788624,30.0277031570956,169.998487073202));
#31257=CARTESIAN_POINT('Ctrl Pts',(31.1116954970284,29.7396663224151,169.887357283982));
#31258=CARTESIAN_POINT('Ctrl Pts',(30.0175516100133,31.0450458879601,169.805886499402));
#31259=CARTESIAN_POINT('Ctrl Pts',(29.9432452019828,31.8621499872163,169.761458977896));
#31260=CARTESIAN_POINT('Ctrl Pts',(29.9444956521925,31.9981860244657,169.754074719462));
#31261=CARTESIAN_POINT('Origin',(32.,32.,180.545925280538));
#31262=CARTESIAN_POINT('',(29.9479977188782,32.00107469184,171.154074719462));
#31263=CARTESIAN_POINT('',(29.9434062437882,31.9984640338121,171.095925280538));
#31264=CARTESIAN_POINT('',(29.94525,32.0000000000002,180.545925280538));
#31265=CARTESIAN_POINT('Ctrl Pts',(29.9434062437882,31.9984640338121,171.095925280538));
#31266=CARTESIAN_POINT('Ctrl Pts',(29.9482705271819,32.581561595502,171.064230358654));
#31267=CARTESIAN_POINT('Ctrl Pts',(30.5126646761233,33.8543847693451,170.995492173698));
#31268=CARTESIAN_POINT('Ctrl Pts',(32.6715856907677,34.3339166171362,170.889710725668));
#31269=CARTESIAN_POINT('Ctrl Pts',(34.3250344470753,32.7017185587553,170.778580936448));
#31270=CARTESIAN_POINT('Ctrl Pts',(33.8506368913683,30.4273152852224,170.667451147229));
#31271=CARTESIAN_POINT('Ctrl Pts',(31.6825565220024,29.5922160075984,170.556321358009));
#31272=CARTESIAN_POINT('Ctrl Pts',(30.1533956337356,30.7067605986327,170.465812735779));
#31273=CARTESIAN_POINT('Ctrl Pts',(29.947551035976,31.6953854228851,170.412347376621));
#31274=CARTESIAN_POINT('Ctrl Pts',(29.9483814718272,31.9993739362354,170.395925280538));
#31275=CARTESIAN_POINT('Ctrl Pts',(29.9479977188782,32.00107469184,171.154074719462));
#31276=CARTESIAN_POINT('Ctrl Pts',(29.9467021955612,32.2742285838469,171.139311468108));
#31277=CARTESIAN_POINT('Ctrl Pts',(30.1245753039347,33.2311487980768,171.087504953681));
#31278=CARTESIAN_POINT('Ctrl Pts',(31.5753550254538,34.3912067810244,170.99865517618));
#31279=CARTESIAN_POINT('Ctrl Pts',(33.7785634234029,33.6537549313479,170.88752538696));
#31280=CARTESIAN_POINT('Ctrl Pts',(34.3540498639709,31.4028045027273,170.77639559774));
#31281=CARTESIAN_POINT('Ctrl Pts',(32.7751353976405,29.6984009168952,170.66526580852));
#31282=CARTESIAN_POINT('Ctrl Pts',(30.5627970543453,30.087049665636,170.557825515761));
#31283=CARTESIAN_POINT('Ctrl Pts',(29.9467925105193,31.3881367057915,170.487428486075));
#31284=CARTESIAN_POINT('Ctrl Pts',(29.9426482690414,32.0011604961315,170.454074719462));
#31285=CARTESIAN_POINT('Origin',(32.,32.,180.545925280538));
#31286=CARTESIAN_POINT('',(29.9465668753081,31.9982546176146,171.854074719462));
#31287=CARTESIAN_POINT('',(29.9435984346504,32.0016034614759,171.795925280538));
#31288=CARTESIAN_POINT('',(29.94525,32.0000000000002,180.545925280538));
#31289=CARTESIAN_POINT('Ctrl Pts',(29.9435984346504,32.0016034614759,171.795925280538));
#31290=CARTESIAN_POINT('Ctrl Pts',(29.9426937786247,32.106960608704,171.790199866834));
#31291=CARTESIAN_POINT('Ctrl Pts',(29.9979550561808,32.8930239645319,171.747431190057));
#31292=CARTESIAN_POINT('Ctrl Pts',(31.0116476380733,34.2184124333546,171.667619250206));
#31293=CARTESIAN_POINT('Ctrl Pts',(33.3276380331233,34.0336104269975,171.556489460986));
#31294=CARTESIAN_POINT('Ctrl Pts',(34.4285884978939,31.987670211439,171.445359671767));
#31295=CARTESIAN_POINT('Ctrl Pts',(33.3069211063375,29.9530140846606,171.334229882547));
#31296=CARTESIAN_POINT('Ctrl Pts',(30.9891736912303,29.7917372689629,171.223100093327));
#31297=CARTESIAN_POINT('Ctrl Pts',(29.9937162190609,31.1210399352016,171.143665225991));
#31298=CARTESIAN_POINT('Ctrl Pts',(29.9425854231113,31.9000695743339,171.101273621728));
#31299=CARTESIAN_POINT('Ctrl Pts',(29.9434062437882,31.9984640338121,171.095925280538));
#31300=CARTESIAN_POINT('Ctrl Pts',(29.9465668753081,31.9982546176146,171.854074719462));
#31301=CARTESIAN_POINT('Ctrl Pts',(29.9504207898182,32.475460648146,171.828237713214));
#31302=CARTESIAN_POINT('Ctrl Pts',(30.3537285412576,33.6427251812827,171.765357443893));
#31303=CARTESIAN_POINT('Ctrl Pts',(32.2966168104817,34.41043807051,171.665433911498));
#31304=CARTESIAN_POINT('Ctrl Pts',(34.1859362572401,33.0582418926255,171.554304122278));
#31305=CARTESIAN_POINT('Ctrl Pts',(34.0747105468639,30.7375542107656,171.443174333058));
#31306=CARTESIAN_POINT('Ctrl Pts',(32.064732243297,29.5722432245585,171.332044543839));
#31307=CARTESIAN_POINT('Ctrl Pts',(30.2704012907663,30.4884300601829,171.235678005973));
#31308=CARTESIAN_POINT('Ctrl Pts',(29.9499528623619,31.5888435532568,171.176354731181));
#31309=CARTESIAN_POINT('Ctrl Pts',(29.9479977188782,32.00107469184,171.154074719462));
#31310=CARTESIAN_POINT('Origin',(32.,32.,180.545925280538));
#31311=CARTESIAN_POINT('',(29.9418222293735,31.9999545502986,172.554074719462));
#31312=CARTESIAN_POINT('',(29.9484394608427,32.0005167851038,172.495925280538));
#31313=CARTESIAN_POINT('',(29.94525,32.0000000000002,180.545925280538));
#31314=CARTESIAN_POINT('Ctrl Pts',(29.9484394608427,32.0005167851038,172.495925280538));
#31315=CARTESIAN_POINT('Ctrl Pts',(29.9477393579576,32.3115072125305,172.47912611194));
#31316=CARTESIAN_POINT('Ctrl Pts',(30.1602043414638,33.3073440021902,172.425283680269));
#31317=CARTESIAN_POINT('Ctrl Pts',(31.7070205866564,34.4108830704008,172.334397985525));
#31318=CARTESIAN_POINT('Ctrl Pts',(33.8665099204009,33.5538129980256,172.223268196305));
#31319=CARTESIAN_POINT('Ctrl Pts',(34.3177896164518,31.2747101202577,172.112138407085));
#31320=CARTESIAN_POINT('Ctrl Pts',(32.6478533909077,29.6593846749887,172.001008617865));
#31321=CARTESIAN_POINT('Ctrl Pts',(30.5015906644606,30.1590252373003,171.89560424235));
#31322=CARTESIAN_POINT('Ctrl Pts',(29.9485468772622,31.4253028764944,171.827243129907));
#31323=CARTESIAN_POINT('Ctrl Pts',(29.9435984346504,32.0016034614759,171.795925280538));
#31324=CARTESIAN_POINT('Ctrl Pts',(29.9418227148716,31.999954556736,172.554074719462));
#31325=CARTESIAN_POINT('Ctrl Pts',(29.9420432276356,32.6776310800843,172.51716395832));
#31326=CARTESIAN_POINT('Ctrl Pts',(30.6781937929071,34.0358273911652,172.443209934105));
#31327=CARTESIAN_POINT('Ctrl Pts',(32.9916984982474,34.2169184271411,172.332212646816));
#31328=CARTESIAN_POINT('Ctrl Pts',(34.4003732162344,32.369325935738,172.221082857597));
#31329=CARTESIAN_POINT('Ctrl Pts',(33.6122523976872,30.1837303531204,172.109953068377));
#31330=CARTESIAN_POINT('Ctrl Pts',(31.3486156689259,29.6603650547029,171.998823279157));
#31331=CARTESIAN_POINT('Ctrl Pts',(30.0688017848057,30.9020694849232,171.913530496186));
#31332=CARTESIAN_POINT('Ctrl Pts',(29.9448953211285,31.791276561209,171.865280976287));
#31333=CARTESIAN_POINT('Ctrl Pts',(29.9465668753081,31.9982546176146,171.854074719462));
#31334=CARTESIAN_POINT('Origin',(32.,32.,180.545925280538));
#31335=CARTESIAN_POINT('',(29.946434452345,32.0017741612164,173.254074719462));
#31336=CARTESIAN_POINT('',(29.9454927345275,31.9981230384932,173.195925280538));
#31337=CARTESIAN_POINT('',(29.94525,32.0000000000002,180.545925280538));
#31338=CARTESIAN_POINT('Ctrl Pts',(29.9454927345275,31.9981230384932,173.195925280538));
#31339=CARTESIAN_POINT('Ctrl Pts',(29.9501524846043,32.5122490504339,173.168052357046));
#31340=CARTESIAN_POINT('Ctrl Pts',(30.4058323872152,33.7170163615654,173.103136170481));
#31341=CARTESIAN_POINT('Ctrl Pts',(32.4282525872759,34.3905634978557,173.001176720843));
#31342=CARTESIAN_POINT('Ctrl Pts',(34.2406392525365,32.936872379666,172.890046931623));
#31343=CARTESIAN_POINT('Ctrl Pts',(34.0024171725965,30.6257658195639,172.778917142403));
#31344=CARTESIAN_POINT('Ctrl Pts',(31.9316046116063,29.5723434784478,172.667787353184));
#31345=CARTESIAN_POINT('Ctrl Pts',(30.2269632474166,30.5640710925998,172.573456732562));
#31346=CARTESIAN_POINT('Ctrl Pts',(29.9492831305079,31.6257530247971,172.516169375013));
#31347=CARTESIAN_POINT('Ctrl Pts',(29.9484394608427,32.0005167851038,172.495925280538));
#31348=CARTESIAN_POINT('Ctrl Pts',(29.946434452345,32.0017741612165,173.254074719462));
#31349=CARTESIAN_POINT('Ctrl Pts',(29.9447676909038,32.2038246610773,173.2431334665));
#31350=CARTESIAN_POINT('Ctrl Pts',(30.0649649197711,33.0880078735651,173.195148950464));
#31351=CARTESIAN_POINT('Ctrl Pts',(31.3319367435559,34.3349271314997,173.110121171355));
#31352=CARTESIAN_POINT('Ctrl Pts',(33.5992505443295,33.8277283497517,172.998991382135));
#31353=CARTESIAN_POINT('Ctrl Pts',(34.4029475900826,31.6478124031995,172.887861592915));
#31354=CARTESIAN_POINT('Ctrl Pts',(33.0074930602737,29.7902147259237,172.776731803695));
#31355=CARTESIAN_POINT('Ctrl Pts',(30.6899918075095,29.9549885673591,172.665602014476));
#31356=CARTESIAN_POINT('Ctrl Pts',(29.9429274456235,31.3149806222681,172.591382986398));
#31357=CARTESIAN_POINT('Ctrl Pts',(29.9418219232767,31.9975218394128,172.554207221394));
#31358=CARTESIAN_POINT('Ctrl Pts',(29.9418227148716,31.999954556736,172.554074719462));
#31359=CARTESIAN_POINT('Origin',(32.,32.,180.545925280538));
#31360=CARTESIAN_POINT('',(29.9480726635453,31.9989926864899,173.954074719462));
#31361=CARTESIAN_POINT('',(29.942062549472,32.0006373960264,173.895925280538));
#31362=CARTESIAN_POINT('',(29.94525,32.0000000000002,180.545925280538));
#31363=CARTESIAN_POINT('Ctrl Pts',(29.942062549472,32.0006373960264,173.895925280538));
#31364=CARTESIAN_POINT('Ctrl Pts',(29.9419201864895,32.0355947650604,173.894021865225));
#31365=CARTESIAN_POINT('Ctrl Pts',(29.958567925244,32.7507355624424,173.85507518684));
#31366=CARTESIAN_POINT('Ctrl Pts',(30.7889645417425,34.1051335431823,173.779085245381));
#31367=CARTESIAN_POINT('Ctrl Pts',(33.1116860073988,34.1592471689786,173.667955456161));
#31368=CARTESIAN_POINT('Ctrl Pts',(34.4170044948166,32.2372412017861,173.556825666941));
#31369=CARTESIAN_POINT('Ctrl Pts',(33.5103066799004,30.0981146594927,173.445695877722));
#31370=CARTESIAN_POINT('Ctrl Pts',(31.2213925701334,29.6995729557439,173.334566088502));
#31371=CARTESIAN_POINT('Ctrl Pts',(30.0404201711272,30.9782715144633,173.251309222774));
#31372=CARTESIAN_POINT('Ctrl Pts',(29.9439596520511,31.8289728552132,173.205095620119));
#31373=CARTESIAN_POINT('Ctrl Pts',(29.9454927345275,31.9981230384932,173.195925280538));
#31374=CARTESIAN_POINT('Ctrl Pts',(29.9480726635453,31.9989926864899,173.954074719462));
#31375=CARTESIAN_POINT('Ctrl Pts',(29.9498795229274,32.4063578846345,173.932059711606));
#31376=CARTESIAN_POINT('Ctrl Pts',(30.264575074801,33.501743750801,173.873001440676));
#31377=CARTESIAN_POINT('Ctrl Pts',(32.0474062520575,34.428156887701,173.776899906673));
#31378=CARTESIAN_POINT('Ctrl Pts',(34.0656489763292,33.2772186698503,173.665770117453));
#31379=CARTESIAN_POINT('Ctrl Pts',(34.1934321584947,30.9573837762123,173.554640328233));
#31380=CARTESIAN_POINT('Ctrl Pts',(32.3138100159872,29.5917399438827,173.443510539014));
#31381=CARTESIAN_POINT('Ctrl Pts',(30.3603257898609,30.3475681436841,173.343322002757));
#31382=CARTESIAN_POINT('Ctrl Pts',(29.9504107632974,31.5197522019245,173.280176729573));
#31383=CARTESIAN_POINT('Ctrl Pts',(29.946434452345,32.0017741612165,173.254074719462));
#31384=CARTESIAN_POINT('Origin',(32.,32.,180.545925280538));
#31385=CARTESIAN_POINT('',(29.9427578740922,31.9987715048219,174.654074719462));
#31386=CARTESIAN_POINT('',(29.9473695970145,32.0014721867752,174.595925280538));
#31387=CARTESIAN_POINT('',(29.94525,32.0000000000002,180.545925280538));
#31388=CARTESIAN_POINT('Ctrl Pts',(29.9473695970144,32.0014721867751,174.595925280538));
#31389=CARTESIAN_POINT('Ctrl Pts',(29.9457798098806,32.2413952649533,174.582948110331));
#31390=CARTESIAN_POINT('Ctrl Pts',(30.0955630473742,33.1642554793996,174.532927677052));
#31391=CARTESIAN_POINT('Ctrl Pts',(31.4608841227388,34.3680262217031,174.445863980699));
#31392=CARTESIAN_POINT('Ctrl Pts',(33.6969994060995,33.7373506069548,174.33473419148));
#31393=CARTESIAN_POINT('Ctrl Pts',(34.3800392361903,31.5166705575043,174.22360440226));
#31394=CARTESIAN_POINT('Ctrl Pts',(32.8848929677704,29.7383283723363,174.11247461304));
#31395=CARTESIAN_POINT('Ctrl Pts',(30.6193818064991,30.0248505035395,174.003248239133));
#31396=CARTESIAN_POINT('Ctrl Pts',(29.944690779633,31.3552729198763,173.931065128299));
#31397=CARTESIAN_POINT('Ctrl Pts',(29.942062549472,32.0006373960264,173.895925280538));
#31398=CARTESIAN_POINT('Ctrl Pts',(29.9427578740922,31.9987715048219,174.654074719462));
#31399=CARTESIAN_POINT('Ctrl Pts',(29.9470582595646,32.6070099091279,174.620985956712));
#31400=CARTESIAN_POINT('Ctrl Pts',(30.5546327375223,33.9036433503181,174.550853930888));
#31401=CARTESIAN_POINT('Ctrl Pts',(32.7586915732648,34.3070718065724,174.443678641991));
#31402=CARTESIAN_POINT('Ctrl Pts',(34.3497283717851,32.6139786664471,174.332548852772));
#31403=CARTESIAN_POINT('Ctrl Pts',(33.7903192461908,30.3589789091108,174.221419063552));
#31404=CARTESIAN_POINT('Ctrl Pts',(31.5924293616864,29.6058238580236,174.110289274332));
#31405=CARTESIAN_POINT('Ctrl Pts',(30.1290567825581,30.7589286472653,174.021174492969));
#31406=CARTESIAN_POINT('Ctrl Pts',(29.9468392347812,31.7209101982179,173.969102974679));
#31407=CARTESIAN_POINT('Ctrl Pts',(29.9480726635453,31.9989926864899,173.954074719462));
#31408=CARTESIAN_POINT('Origin',(32.,32.,180.545925280538));
#31409=CARTESIAN_POINT('',(29.9443485008314,32.0017900557221,175.354074719462));
#31410=CARTESIAN_POINT('',(29.947375766131,31.998530717209,175.295925280538));
#31411=CARTESIAN_POINT('',(29.94525,32.0000000000002,180.545925280538));
#31412=CARTESIAN_POINT('Ctrl Pts',(29.947375766131,31.998530717209,175.295925280538));
#31413=CARTESIAN_POINT('Ctrl Pts',(29.9503157790678,32.4431897218401,175.271874355438));
#31414=CARTESIAN_POINT('Ctrl Pts',(30.3106831269541,33.5770542377908,175.210780167264));
#31415=CARTESIAN_POINT('Ctrl Pts',(32.1803873389287,34.4219113368872,175.112642716017));
#31416=CARTESIAN_POINT('Ctrl Pts',(34.1325316462971,33.1621113945443,175.001512926798));
#31417=CARTESIAN_POINT('Ctrl Pts',(34.1330061173171,30.8387597064878,174.890383137578));
#31418=CARTESIAN_POINT('Ctrl Pts',(32.1813765212566,29.578162541927,174.779253348358));
#31419=CARTESIAN_POINT('Ctrl Pts',(30.3110383666457,30.4223863748083,174.681100729345));
#31420=CARTESIAN_POINT('Ctrl Pts',(29.9503178487669,31.5565361191587,174.619991373405));
#31421=CARTESIAN_POINT('Ctrl Pts',(29.9473695970144,32.0014721867751,174.595925280538));
#31422=CARTESIAN_POINT('Ctrl Pts',(29.9443485008314,32.0017900557221,175.354074719462));
#31423=CARTESIAN_POINT('Ctrl Pts',(29.9431493621631,32.1329198955122,175.346955464891));
#31424=CARTESIAN_POINT('Ctrl Pts',(30.0143161668846,32.9450545098133,175.302792947247));
#31425=CARTESIAN_POINT('Ctrl Pts',(31.0955884935522,34.2539372331611,175.221587166529));
#31426=CARTESIAN_POINT('Ctrl Pts',(33.4030129919618,33.982359142136,175.11045737731));
#31427=CARTESIAN_POINT('Ctrl Pts',(34.4264152151701,31.8965474620181,174.99932758809));
#31428=CARTESIAN_POINT('Ctrl Pts',(33.2291885468321,29.905414422765,174.88819779887));
#31429=CARTESIAN_POINT('Ctrl Pts',(30.9070218504281,29.8312233889627,174.77706800965));
#31430=CARTESIAN_POINT('Ctrl Pts',(29.9787265765459,31.1729794811598,174.699026983181));
#31431=CARTESIAN_POINT('Ctrl Pts',(29.9422439269294,31.9260797881724,174.658029219785));
#31432=CARTESIAN_POINT('Ctrl Pts',(29.9427578740922,31.9987715048219,174.654074719462));
#31433=CARTESIAN_POINT('Origin',(32.,32.,180.545925280538));
#31434=CARTESIAN_POINT('',(29.9485554566374,32.0000997966407,176.054074719462));
#31435=CARTESIAN_POINT('',(29.9420662255838,31.9993577651234,175.995925280538));
#31436=CARTESIAN_POINT('',(29.94525,32.0000000000002,180.545925280538));
#31437=CARTESIAN_POINT('Ctrl Pts',(29.9420662255838,31.9993577651234,175.995925280538));
#31438=CARTESIAN_POINT('Ctrl Pts',(29.9447109731776,32.6444467488492,175.960800600544));
#31439=CARTESIAN_POINT('Ctrl Pts',(30.6188897830895,33.9746253531368,175.888632657477));
#31440=CARTESIAN_POINT('Ctrl Pts',(32.8839691443584,34.2620328617456,175.779421451336));
#31441=CARTESIAN_POINT('Ctrl Pts',(34.3798416282082,32.4843014974535,175.668291662116));
#31442=CARTESIAN_POINT('Ctrl Pts',(33.6977088622292,30.2633426547257,175.557161872896));
#31443=CARTESIAN_POINT('Ctrl Pts',(31.4618513564243,29.6317537811269,175.446032083677));
#31444=CARTESIAN_POINT('Ctrl Pts',(30.0958007863447,30.8351763931134,175.358953219557));
#31445=CARTESIAN_POINT('Ctrl Pts',(29.9457875676912,31.7583254009107,175.308917618511));
#31446=CARTESIAN_POINT('Ctrl Pts',(29.947375766131,31.998530717209,175.295925280538));
#31447=CARTESIAN_POINT('Ctrl Pts',(29.9485554566374,32.0000997966407,176.054074719462));
#31448=CARTESIAN_POINT('Ctrl Pts',(29.948409504624,32.3369407875857,176.035881709997));
#31449=CARTESIAN_POINT('Ctrl Pts',(30.1862169518775,33.3594384580515,175.980645437459));
#31450=CARTESIAN_POINT('Ctrl Pts',(31.7976939990458,34.4201788169579,175.888365901848));
#31451=CARTESIAN_POINT('Ctrl Pts',(33.9235011844546,33.4826787977943,175.777236112628));
#31452=CARTESIAN_POINT('Ctrl Pts',(34.2889409453366,31.1882472218883,175.666106323408));
#31453=CARTESIAN_POINT('Ctrl Pts',(32.5595667755852,29.6367229854095,175.554976534189));
#31454=CARTESIAN_POINT('Ctrl Pts',(30.4616782545197,30.2088814624134,175.45096599954));
#31455=CARTESIAN_POINT('Ctrl Pts',(29.9493887807299,31.4506185248328,175.383998727964));
#31456=CARTESIAN_POINT('Ctrl Pts',(29.9443485008314,32.0017900557221,175.354074719462));
#31457=CARTESIAN_POINT('Origin',(32.,32.,180.545925280538));
#31458=CARTESIAN_POINT('',(29.9447147371656,31.9981575239013,176.754074719462));
#31459=CARTESIAN_POINT('',(29.9454843589828,32.0018771439066,176.695925280538));
#31460=CARTESIAN_POINT('',(29.94525,32.0000000000002,180.545925280538));
#31461=CARTESIAN_POINT('Ctrl Pts',(29.9454843589828,32.0018771439066,176.695925280538));
#31462=CARTESIAN_POINT('Ctrl Pts',(29.9439531205472,32.1707457963473,176.686770108723));
#31463=CARTESIAN_POINT('Ctrl Pts',(30.0402180779942,33.021161077992,176.640571673835));
#31464=CARTESIAN_POINT('Ctrl Pts',(31.2204530563734,34.3001088403402,176.557329975874));
#31465=CARTESIAN_POINT('Ctrl Pts',(33.5095297542162,33.9025020465923,176.446200186654));
#31466=CARTESIAN_POINT('Ctrl Pts',(34.417101191225,31.7637460111891,176.335070397435));
#31467=CARTESIAN_POINT('Ctrl Pts',(33.112567830368,29.8412070644691,176.223940608215));
#31468=CARTESIAN_POINT('Ctrl Pts',(30.7898244564675,29.8943720011186,176.112810818995));
#31469=CARTESIAN_POINT('Ctrl Pts',(29.95870886397,31.2487009777082,176.036805709769));
#31470=CARTESIAN_POINT('Ctrl Pts',(29.9419217639693,31.9641216630728,175.997843863617));
#31471=CARTESIAN_POINT('Ctrl Pts',(29.9420662255838,31.9993577651234,175.995925280538));
#31472=CARTESIAN_POINT('Ctrl Pts',(29.9447147371656,31.9981575239013,176.754074719462));
#31473=CARTESIAN_POINT('Ctrl Pts',(29.9496923005573,32.53747043377,176.724807955104));
#31474=CARTESIAN_POINT('Ctrl Pts',(30.4434117295339,33.7674633987223,176.658497927671));
#31475=CARTESIAN_POINT('Ctrl Pts',(32.5176555073463,34.3728097273692,176.555144637166));
#31476=CARTESIAN_POINT('Ctrl Pts',(34.2742166391108,32.8521337355438,176.444014847946));
#31477=CARTESIAN_POINT('Ctrl Pts',(33.9494393645001,30.5515941911541,176.332885058726));
#31478=CARTESIAN_POINT('Ctrl Pts',(31.8405563248355,29.5766199351239,176.221755269507));
#31479=CARTESIAN_POINT('Ctrl Pts',(30.1989500491814,30.6160259976346,176.128818489752));
#31480=CARTESIAN_POINT('Ctrl Pts',(29.9487066813412,31.6510900235642,176.072924973071));
#31481=CARTESIAN_POINT('Ctrl Pts',(29.9485554566374,32.0000997966407,176.054074719462));
#31482=CARTESIAN_POINT('Origin',(32.,32.,180.545925280538));
#31483=CARTESIAN_POINT('',(29.9424956572377,32.001054844556,177.454074719462));
#31484=CARTESIAN_POINT('',(29.9484415613596,31.9994876371231,177.395925280538));
#31485=CARTESIAN_POINT('',(29.94525,32.0000000000002,180.545925280538));
#31486=CARTESIAN_POINT('Ctrl Pts',(29.9484415613596,31.9994876371231,177.395925280538));
#31487=CARTESIAN_POINT('Ctrl Pts',(29.9492773107838,32.3739715709387,177.375696353829));
#31488=CARTESIAN_POINT('Ctrl Pts',(30.2266509361282,33.4353642145681,177.318424164048));
#31489=CARTESIAN_POINT('Ctrl Pts',(31.9306130756526,34.4276283682218,177.224108711192));
#31490=CARTESIAN_POINT('Ctrl Pts',(34.0018557168478,33.3750519340786,177.112978921973));
#31491=CARTESIAN_POINT('Ctrl Pts',(34.2410217192136,31.0640428539123,177.001849132753));
#31492=CARTESIAN_POINT('Ctrl Pts',(32.429228945055,29.6096116174522,176.890719343533));
#31493=CARTESIAN_POINT('Ctrl Pts',(30.4062329110444,30.2824327403001,176.788744726128));
#31494=CARTESIAN_POINT('Ctrl Pts',(29.9501487517539,31.4874767060651,176.723813371796));
#31495=CARTESIAN_POINT('Ctrl Pts',(29.9454843589828,32.0018771439066,176.695925280538));
#31496=CARTESIAN_POINT('Ctrl Pts',(29.9424956572377,32.001054844556,177.454074719462));
#31497=CARTESIAN_POINT('Ctrl Pts',(29.9421163386554,32.0616447486548,177.450777463283));
#31498=CARTESIAN_POINT('Ctrl Pts',(29.9720236842432,32.802556573488,177.41043694403));
#31499=CARTESIAN_POINT('Ctrl Pts',(30.8688116111015,34.1490940941566,177.333053161704));
#31500=CARTESIAN_POINT('Ctrl Pts',(33.1919274796751,34.1160109178655,177.221923372484));
#31501=CARTESIAN_POINT('Ctrl Pts',(34.4242044061711,32.1463773227603,177.110793583265));
#31502=CARTESIAN_POINT('Ctrl Pts',(33.4378756702622,30.0427808747097,176.999663794045));
#31503=CARTESIAN_POINT('Ctrl Pts',(31.135618752982,29.7304101029964,176.888534004825));
#31504=CARTESIAN_POINT('Ctrl Pts',(30.0224146087878,31.0303892340693,176.806670979964));
#31505=CARTESIAN_POINT('Ctrl Pts',(29.9433921442462,31.8548561975641,176.761851218177));
#31506=CARTESIAN_POINT('Ctrl Pts',(29.9447147371656,31.9981575239013,176.754074719462));
#31507=CARTESIAN_POINT('Origin',(32.,32.,180.545925280538));
#31508=CARTESIAN_POINT('',(29.94788119656,32.0011671080005,178.154074719462));
#31509=CARTESIAN_POINT('',(29.9436064940107,31.9983925140785,178.095925280538));
#31510=CARTESIAN_POINT('',(29.94525,32.0000000000002,180.545925280538));
#31511=CARTESIAN_POINT('Ctrl Pts',(29.9436064940107,31.9983925140785,178.095925280538));
#31512=CARTESIAN_POINT('Ctrl Pts',(29.9485577871795,32.5744195019018,178.064622598935));
#31513=CARTESIAN_POINT('Ctrl Pts',(30.5011473846441,33.8404367251789,177.99627665426));
#31514=CARTESIAN_POINT('Ctrl Pts',(32.6468975047867,34.3408786212549,177.890887446511));
#31515=CARTESIAN_POINT('Ctrl Pts',(34.3174931090689,32.7262370373898,177.779757657291));
#31516=CARTESIAN_POINT('Ctrl Pts',(33.8671444377423,30.4469492135679,177.668627868071));
#31517=CARTESIAN_POINT('Ctrl Pts',(31.7080052850452,29.5889975993134,177.557498078852));
#31518=CARTESIAN_POINT('Ctrl Pts',(30.1604802454635,30.6920887002321,177.46659721634));
#31519=CARTESIAN_POINT('Ctrl Pts',(29.9477468842698,31.688215619726,177.412739616902));
#31520=CARTESIAN_POINT('Ctrl Pts',(29.9484415613596,31.9994876371231,177.395925280538));
#31521=CARTESIAN_POINT('Ctrl Pts',(29.94788119656,32.0011671080005,178.154074719462));
#31522=CARTESIAN_POINT('Ctrl Pts',(29.9464999255155,32.2670274771179,178.139703708389));
#31523=CARTESIAN_POINT('Ctrl Pts',(30.1180175427899,33.2164703394171,178.088289434242));
#31524=CARTESIAN_POINT('Ctrl Pts',(31.5501292046485,34.3865813061288,177.999831897022));
#31525=CARTESIAN_POINT('Ctrl Pts',(33.7609940320372,33.6724513469602,177.888702107803));
#31526=CARTESIAN_POINT('Ctrl Pts',(34.3602277126424,31.4276996634035,177.777572318583));
#31527=CARTESIAN_POINT('Ctrl Pts',(32.7994009405473,29.7067171266042,177.666442529363));
#31528=CARTESIAN_POINT('Ctrl Pts',(30.5749909099132,30.073309708925,177.558609996323));
#31529=CARTESIAN_POINT('Ctrl Pts',(29.9463778207077,31.3809430879688,177.487820726356));
#31530=CARTESIAN_POINT('Ctrl Pts',(29.9424956572377,32.001054844556,177.454074719462));
#31531=CARTESIAN_POINT('Origin',(32.,32.,180.545925280538));
#31532=CARTESIAN_POINT('',(29.9473399467332,31.997818150837,178.854074719462));
#31533=CARTESIAN_POINT('',(29.943403128554,32.0015021399478,178.795925280538));
#31534=CARTESIAN_POINT('',(29.94525,32.0000000000002,180.545925280538));
#31535=CARTESIAN_POINT('',(31.4698297828098,30.0148256743287,179.));
#31536=CARTESIAN_POINT('Ctrl Pts',(31.4698297828098,30.0148256743287,179.));
#31537=CARTESIAN_POINT('Ctrl Pts',(30.8097602092458,30.191107033931,178.962956736927));
#31538=CARTESIAN_POINT('Ctrl Pts',(30.0751176592089,30.8874016782087,178.914314976748));
#31539=CARTESIAN_POINT('Ctrl Pts',(29.9457279749651,31.7835486120402,178.865673216568));
#31540=CARTESIAN_POINT('Ctrl Pts',(29.9473399467332,31.997818150837,178.854074719462));
#31541=CARTESIAN_POINT('',(32.5313335162366,30.0112662127558,179.));
#31542=CARTESIAN_POINT('Origin',(32.,32.,179.));
#31543=CARTESIAN_POINT('Ctrl Pts',(32.5313343916937,30.0112635340336,179.));
#31544=CARTESIAN_POINT('Ctrl Pts',(31.8868947492701,29.8400087423844,178.963685183163));
#31545=CARTESIAN_POINT('Ctrl Pts',(30.5070458206693,30.1591330867848,178.895660276675));
#31546=CARTESIAN_POINT('Ctrl Pts',(29.9482460569429,31.418251748985,178.827635370188));
#31547=CARTESIAN_POINT('Ctrl Pts',(29.943403128554,32.0015021399478,178.795925280538));
#31548=CARTESIAN_POINT('Origin',(32.,32.,166.));
#31549=CARTESIAN_POINT('Ctrl Pts',(32.6750771856741,30.4769022377462,166.));
#31550=CARTESIAN_POINT('Ctrl Pts',(32.7347503609899,30.4954853005658,166.));
#31551=CARTESIAN_POINT('Ctrl Pts',(32.7931107758957,30.517643791226,166.));
#31552=CARTESIAN_POINT('Ctrl Pts',(32.8500021112569,30.543078531189,166.));
#31553=CARTESIAN_POINT('Ctrl Pts',(32.8860692382174,30.5592032712681,166.));
#31554=CARTESIAN_POINT('Ctrl Pts',(32.9215459750197,30.5766458765615,166.));
#31555=CARTESIAN_POINT('Ctrl Pts',(32.9563915928315,30.595340546146,166.));
#31556=CARTESIAN_POINT('Ctrl Pts',(32.9799636192767,30.6079869353767,166.));
#31557=CARTESIAN_POINT('Ctrl Pts',(33.003246819653,30.6212064489651,166.));
#31558=CARTESIAN_POINT('Ctrl Pts',(33.026228134647,30.6349806231606,166.));
#31559=CARTESIAN_POINT('Ctrl Pts',(33.0386988538539,30.6424551240212,166.));
#31560=CARTESIAN_POINT('Ctrl Pts',(33.0510807692731,30.6500931856874,166.));
#31561=CARTESIAN_POINT('Ctrl Pts',(33.0633592146747,30.6578836587174,166.));
#31562=CARTESIAN_POINT('Ctrl Pts',(33.1190569517964,30.6932229630581,166.));
#31563=CARTESIAN_POINT('Ctrl Pts',(33.1726914481055,30.7317324396433,166.));
#31564=CARTESIAN_POINT('Ctrl Pts',(33.2240811435114,30.7731091649049,166.));
#31565=CARTESIAN_POINT('Ctrl Pts',(33.26116458371,30.8029671219278,166.));
#31566=CARTESIAN_POINT('Ctrl Pts',(33.2970790166423,30.8343193445405,166.));
#31567=CARTESIAN_POINT('Ctrl Pts',(33.3317509313883,30.8670679003715,166.));
#31568=CARTESIAN_POINT('Ctrl Pts',(33.3411297504378,30.8759264471671,166.));
#31569=CARTESIAN_POINT('Ctrl Pts',(33.3504176191284,30.8848872340675,166.));
#31570=CARTESIAN_POINT('Ctrl Pts',(33.3596130010376,30.8939484703997,166.));
#31571=CARTESIAN_POINT('Ctrl Pts',(33.3693213148669,30.9035151558146,166.));
#31572=CARTESIAN_POINT('Ctrl Pts',(33.3789211058175,30.9131885267339,166.));
#31573=CARTESIAN_POINT('Ctrl Pts',(33.3884063294392,30.9229612927792,166.));
#31574=CARTESIAN_POINT('Ctrl Pts',(33.4356623618964,30.971649881246,166.));
#31575=CARTESIAN_POINT('Ctrl Pts',(33.4801121956722,31.0228370852842,166.));
#31576=CARTESIAN_POINT('Ctrl Pts',(33.521572359897,31.076215396252,166.));
#31577=CARTESIAN_POINT('Ctrl Pts',(33.5636369413539,31.1303718703451,166.));
#31578=CARTESIAN_POINT('Ctrl Pts',(33.6026249400945,31.1867843836557,166.));
#31579=CARTESIAN_POINT('Ctrl Pts',(33.6383203879709,31.2451787105165,166.));
#31580=CARTESIAN_POINT('Ctrl Pts',(33.6604356779493,31.2813572024097,166.));
#31581=CARTESIAN_POINT('Ctrl Pts',(33.681286598243,31.3182973027154,166.));
#31582=CARTESIAN_POINT('Ctrl Pts',(33.7008148714994,31.3559410756793,166.));
#31583=CARTESIAN_POINT('Ctrl Pts',(33.7167939181414,31.3867431643266,166.));
#31584=CARTESIAN_POINT('Ctrl Pts',(33.7318873234198,31.4180165031838,166.));
#31585=CARTESIAN_POINT('Ctrl Pts',(33.7460598402509,31.4497315614662,166.));
#31586=CARTESIAN_POINT('Ctrl Pts',(33.7518824450571,31.4627613043825,166.));
#31587=CARTESIAN_POINT('Ctrl Pts',(33.7575504884881,31.4758681482794,166.));
#31588=CARTESIAN_POINT('Ctrl Pts',(33.7630523129776,31.4890274543404,166.));
#31589=CARTESIAN_POINT('Ctrl Pts',(33.7902428497693,31.5540619890274,166.));
#31590=CARTESIAN_POINT('Ctrl Pts',(33.8134282692681,31.6204867128424,166.));
#31591=CARTESIAN_POINT('Ctrl Pts',(33.8323971728471,31.6880059658203,166.));
#31592=CARTESIAN_POINT('Ctrl Pts',(33.8345003075094,31.6954920116385,166.));
#31593=CARTESIAN_POINT('Ctrl Pts',(33.8365515737096,31.7029915509816,166.));
#31594=CARTESIAN_POINT('Ctrl Pts',(33.8385506551699,31.7105042086362,166.));
#31595=CARTESIAN_POINT('Ctrl Pts',(33.8558906957491,31.7756690311676,166.));
#31596=CARTESIAN_POINT('Ctrl Pts',(33.8693083355635,31.841818801265,166.));
#31597=CARTESIAN_POINT('Ctrl Pts',(33.8789575263444,31.9086493575129,166.));
#31598=CARTESIAN_POINT('Ctrl Pts',(33.8893364873223,31.9805343218772,166.));
#31599=CARTESIAN_POINT('Ctrl Pts',(33.8953560454952,32.053207734444,166.));
#31600=CARTESIAN_POINT('Ctrl Pts',(33.8971476570148,32.1263135842633,166.));
#31601=CARTESIAN_POINT('Ctrl Pts',(33.8974689398799,32.139423377666,166.));
#31602=CARTESIAN_POINT('Ctrl Pts',(33.8976541013751,32.1525471118987,166.));
#31603=CARTESIAN_POINT('Ctrl Pts',(33.897703691189,32.1656827687867,166.));
#31604=CARTESIAN_POINT('Ctrl Pts',(33.8977482228948,32.1774786026478,166.));
#31605=CARTESIAN_POINT('Ctrl Pts',(33.8976833755783,32.1892753621347,166.));
#31606=CARTESIAN_POINT('Ctrl Pts',(33.8975100927964,32.2010683060168,166.));
#31607=CARTESIAN_POINT('Ctrl Pts',(33.8964659681176,32.2721273206843,166.));
#31608=CARTESIAN_POINT('Ctrl Pts',(33.8914890591272,32.3430829139215,166.));
#31609=CARTESIAN_POINT('Ctrl Pts',(33.8827593811525,32.4135998306956,166.));
#31610=CARTESIAN_POINT('Ctrl Pts',(33.8738459191009,32.4856013253083,166.));
#31611=CARTESIAN_POINT('Ctrl Pts',(33.8610200659792,32.5571464132172,166.));
#31612=CARTESIAN_POINT('Ctrl Pts',(33.8444207498015,32.6278943811675,166.));
#31613=CARTESIAN_POINT('Ctrl Pts',(33.8277211179619,32.6990699046362,166.));
#31614=CARTESIAN_POINT('Ctrl Pts',(33.8072021977498,32.7694397140702,166.));
#31615=CARTESIAN_POINT('Ctrl Pts',(33.7829530525617,32.838657794496,166.));
#31616=CARTESIAN_POINT('Ctrl Pts',(33.7769688688708,32.8557393742708,166.));
#31617=CARTESIAN_POINT('Ctrl Pts',(33.7707572694931,32.8727507741706,166.));
#31618=CARTESIAN_POINT('Ctrl Pts',(33.7643191147679,32.8896866837861,166.));
#31619=CARTESIAN_POINT('Ctrl Pts',(33.7592567630984,32.9030034700357,166.));
#31620=CARTESIAN_POINT('Ctrl Pts',(33.7540535771897,32.9162751484824,166.));
#31621=CARTESIAN_POINT('Ctrl Pts',(33.7487183848038,32.9294790135144,166.));
#31622=CARTESIAN_POINT('Ctrl Pts',(33.7204961526954,32.9993251440211,166.));
#31623=CARTESIAN_POINT('Ctrl Pts',(33.6885374698854,33.0674004678931,166.));
#31624=CARTESIAN_POINT('Ctrl Pts',(33.6530002833894,33.1333480759195,166.));
#31625=CARTESIAN_POINT('Ctrl Pts',(33.6174247832409,33.1993667839398,166.));
#31626=CARTESIAN_POINT('Ctrl Pts',(33.5782628879173,33.2632543000954,166.));
#31627=CARTESIAN_POINT('Ctrl Pts',(33.5356212918425,33.3246481266484,166.));
#31628=CARTESIAN_POINT('Ctrl Pts',(33.4939489743217,33.3846464210237,166.));
#31629=CARTESIAN_POINT('Ctrl Pts',(33.4489530129887,33.4422640865906,166.));
#31630=CARTESIAN_POINT('Ctrl Pts',(33.4006876508977,33.4971431728771,166.));
#31631=CARTESIAN_POINT('Ctrl Pts',(33.390360214247,33.5088857614027,166.));
#31632=CARTESIAN_POINT('Ctrl Pts',(33.3798829330801,33.5205028633375,166.));
#31633=CARTESIAN_POINT('Ctrl Pts',(33.3692560829687,33.5319907854683,166.));
#31634=CARTESIAN_POINT('Ctrl Pts',(33.3601453871862,33.541839702373,166.));
#31635=CARTESIAN_POINT('Ctrl Pts',(33.3509247547157,33.5515936692396,166.));
#31636=CARTESIAN_POINT('Ctrl Pts',(33.3415960466845,33.5612522690861,166.));
#31637=CARTESIAN_POINT('Ctrl Pts',(32.3836679988478,34.0186125009918,166.));
#31638=CARTESIAN_POINT('Ctrl Pts',(32.3093572659554,34.025632435417,166.));
#31639=CARTESIAN_POINT('Ctrl Pts',(32.2347977339105,34.0282488060548,166.));
#31640=CARTESIAN_POINT('Ctrl Pts',(32.1603115857106,34.0266257027317,166.));
#31641=CARTESIAN_POINT('Ctrl Pts',(32.0877757087159,34.0250450971313,166.));
#31642=CARTESIAN_POINT('Ctrl Pts',(32.0153086399907,34.0194434654372,166.));
#31643=CARTESIAN_POINT('Ctrl Pts',(31.9432211087107,34.0099284747844,166.));
#31644=CARTESIAN_POINT('Ctrl Pts',(31.9271313205272,34.0078047485109,166.));
#31645=CARTESIAN_POINT('Ctrl Pts',(31.9110583935699,34.0054855770819,166.));
#31646=CARTESIAN_POINT('Ctrl Pts',(31.8950127275189,34.0029729711849,166.));
#31647=CARTESIAN_POINT('Ctrl Pts',(31.8213764524233,33.9914421978003,166.));
#31648=CARTESIAN_POINT('Ctrl Pts',(31.7484594020235,33.9758656436188,166.));
#31649=CARTESIAN_POINT('Ctrl Pts',(31.6765936654897,33.9563833455214,166.));
#31650=CARTESIAN_POINT('Ctrl Pts',(31.6261432248504,33.9427065842289,166.));
#31651=CARTESIAN_POINT('Ctrl Pts',(31.5762111638781,33.9271039121742,166.));
#31652=CARTESIAN_POINT('Ctrl Pts',(31.5269203117965,33.9096106347237,166.));
#31653=CARTESIAN_POINT('Ctrl Pts',(31.5081989768218,33.9029664503949,166.));
#31654=CARTESIAN_POINT('Ctrl Pts',(31.489570224729,33.89604942776,166.));
#31655=CARTESIAN_POINT('Ctrl Pts',(31.4710411187568,33.8888611393757,166.));
#31656=CARTESIAN_POINT('Ctrl Pts',(31.453339056705,33.8819936991863,166.));
#31657=CARTESIAN_POINT('Ctrl Pts',(31.4357224678685,33.8748762081473,166.));
#31658=CARTESIAN_POINT('Ctrl Pts',(31.418228472615,33.8675232892194,166.));
#31659=CARTESIAN_POINT('Ctrl Pts',(31.3512969247421,33.839391222296,166.));
#31660=CARTESIAN_POINT('Ctrl Pts',(31.286085531597,33.8077910186021,166.));
#31661=CARTESIAN_POINT('Ctrl Pts',(31.222902662924,33.7728503444856,166.));
#31662=CARTESIAN_POINT('Ctrl Pts',(31.1610752783328,33.7386592648171,166.));
#31663=CARTESIAN_POINT('Ctrl Pts',(31.101189617399,33.7012688782765,166.));
#31664=CARTESIAN_POINT('Ctrl Pts',(31.0435669985648,33.6607619986751,166.));
#31665=CARTESIAN_POINT('Ctrl Pts',(30.9872087184241,33.6211439092098,166.));
#31666=CARTESIAN_POINT('Ctrl Pts',(30.9330146978204,33.5785440615488,166.));
#31667=CARTESIAN_POINT('Ctrl Pts',(30.881326012577,33.533012736002,166.));
#31668=CARTESIAN_POINT('Ctrl Pts',(30.8645070947255,33.518197353865,166.));
#31669=CARTESIAN_POINT('Ctrl Pts',(30.847953796244,33.5030714073101,166.));
#31670=CARTESIAN_POINT('Ctrl Pts',(30.8316789699842,33.4876361269411,166.));
#31671=CARTESIAN_POINT('Ctrl Pts',(30.822544331258,33.4789727035929,166.));
#31672=CARTESIAN_POINT('Ctrl Pts',(30.8134965950441,33.4702108648157,166.));
#31673=CARTESIAN_POINT('Ctrl Pts',(30.8045505016545,33.4613634585313,166.));
#31674=CARTESIAN_POINT('Ctrl Pts',(30.755981374825,33.4133301126647,166.));
#31675=CARTESIAN_POINT('Ctrl Pts',(30.7103172604148,33.362695681989,166.));
#31676=CARTESIAN_POINT('Ctrl Pts',(30.6678506938977,33.3095416270432,166.));
#31677=CARTESIAN_POINT('Ctrl Pts',(30.6617467956725,33.3019015711532,166.));
#31678=CARTESIAN_POINT('Ctrl Pts',(30.6557090297941,33.294209411133,166.));
#31679=CARTESIAN_POINT('Ctrl Pts',(30.6497383407345,33.2864653404541,166.));
#31680=CARTESIAN_POINT('Ctrl Pts',(30.6073793742087,33.231525143873,166.));
#31681=CARTESIAN_POINT('Ctrl Pts',(30.5683924357624,33.1739735703695,166.));
#31682=CARTESIAN_POINT('Ctrl Pts',(30.5328446438884,33.1141723821926,166.));
#31683=CARTESIAN_POINT('Ctrl Pts',(30.4996834403046,33.0583860936178,166.));
#31684=CARTESIAN_POINT('Ctrl Pts',(30.4695154958343,33.0006411409872,166.));
#31685=CARTESIAN_POINT('Ctrl Pts',(30.4424350121092,32.9412257684441,166.));
#31686=CARTESIAN_POINT('Ctrl Pts',(30.4365396641451,32.9282912027578,166.));
#31687=CARTESIAN_POINT('Ctrl Pts',(30.4307907839553,32.9152774801085,166.));
#31688=CARTESIAN_POINT('Ctrl Pts',(30.425189589237,32.9021876017612,166.));
#31689=CARTESIAN_POINT('Ctrl Pts',(30.4206630898284,32.8916092645353,166.));
#31690=CARTESIAN_POINT('Ctrl Pts',(30.4162332674005,32.8809814978217,166.));
#31691=CARTESIAN_POINT('Ctrl Pts',(30.4119057840018,32.8703189087348,166.));
#31692=CARTESIAN_POINT('Ctrl Pts',(30.3861953241676,32.8069702963444,166.));
#31693=CARTESIAN_POINT('Ctrl Pts',(30.3640424511415,32.7422771632775,166.));
#31694=CARTESIAN_POINT('Ctrl Pts',(30.3454933162505,32.6765891288769,166.));
#31695=CARTESIAN_POINT('Ctrl Pts',(30.3270294720946,32.6112031344786,166.));
#31696=CARTESIAN_POINT('Ctrl Pts',(30.312136294192,32.5448302322262,166.));
#31697=CARTESIAN_POINT('Ctrl Pts',(30.3009103653718,32.4778126146351,166.));
#31698=CARTESIAN_POINT('Ctrl Pts',(30.2899244778469,32.4122280183993,166.));
#31699=CARTESIAN_POINT('Ctrl Pts',(30.2824508141855,32.3460250202532,166.));
#31700=CARTESIAN_POINT('Ctrl Pts',(30.2786277887395,32.2795372024809,166.));
#31701=CARTESIAN_POINT('Ctrl Pts',(30.2778239402128,32.2655571400626,166.));
#31702=CARTESIAN_POINT('Ctrl Pts',(30.2771816595994,32.2515645602645,166.));
#31703=CARTESIAN_POINT('Ctrl Pts',(30.2767025029043,32.2375626988325,166.));
#31704=CARTESIAN_POINT('Ctrl Pts',(30.2762461158735,32.2242262098933,166.));
#31705=CARTESIAN_POINT('Ctrl Pts',(30.275937815966,32.2108794399599,166.));
#31706=CARTESIAN_POINT('Ctrl Pts',(30.2757789255977,32.1975468702567,166.));
#31707=CARTESIAN_POINT('Ctrl Pts',(30.2750003283029,32.1322143846253,166.));
#31708=CARTESIAN_POINT('Ctrl Pts',(30.2778000976172,32.0671060893232,166.));
#31709=CARTESIAN_POINT('Ctrl Pts',(30.2842564239881,32.0025315850275,166.));
#31710=CARTESIAN_POINT('Ctrl Pts',(30.2905901747519,31.9391830502096,166.));
#31711=CARTESIAN_POINT('Ctrl Pts',(30.3004431130711,31.8763473623559,166.));
#31712=CARTESIAN_POINT('Ctrl Pts',(30.313935719542,31.8143339857026,166.));
#31713=CARTESIAN_POINT('Ctrl Pts',(30.326990711639,31.7543319287344,166.));
#31714=CARTESIAN_POINT('Ctrl Pts',(30.3434533403295,31.6950990830377,166.));
#31715=CARTESIAN_POINT('Ctrl Pts',(30.3634738587928,31.6369426601543,166.));
#31716=CARTESIAN_POINT('Ctrl Pts',(30.3667806417163,31.6273369815383,166.));
#31717=CARTESIAN_POINT('Ctrl Pts',(30.3701845768421,31.6177607418433,166.));
#31718=CARTESIAN_POINT('Ctrl Pts',(30.3736864471722,31.608215416664,166.));
#31719=CARTESIAN_POINT('Ctrl Pts',(30.3774492972764,31.5979587182547,166.));
#31720=CARTESIAN_POINT('Ctrl Pts',(30.3813252251034,31.5877377137682,166.));
#31721=CARTESIAN_POINT('Ctrl Pts',(30.3853131747227,31.5775537673674,166.));
#31722=CARTESIAN_POINT('Origin',(32.,32.,180.545925280538));
#31723=CARTESIAN_POINT('Ctrl Pts',(29.943403128554,32.0015021399478,178.795925280538));
#31724=CARTESIAN_POINT('Ctrl Pts',(29.9425886188109,32.0995963275832,178.790592107115));
#31725=CARTESIAN_POINT('Ctrl Pts',(29.9935746829529,32.8782050744218,178.748215670618));
#31726=CARTESIAN_POINT('Ctrl Pts',(30.9882484770451,34.2080115613757,178.668795971049));
#31727=CARTESIAN_POINT('Ctrl Pts',(33.3060964076047,34.0474400400451,178.557666181829));
#31728=CARTESIAN_POINT('Ctrl Pts',(34.4285776240291,32.013360755941,178.446536392609));
#31729=CARTESIAN_POINT('Ctrl Pts',(33.3284712910932,29.9669128233058,178.33540660339));
#31730=CARTESIAN_POINT('Ctrl Pts',(31.0125524422092,29.7811934898284,178.22427681417));
#31731=CARTESIAN_POINT('Ctrl Pts',(29.9981273146683,31.1064095349383,178.144449706553));
#31732=CARTESIAN_POINT('Ctrl Pts',(29.9426984790942,31.8927552432854,178.101665862009));
#31733=CARTESIAN_POINT('Ctrl Pts',(29.9436064940107,31.9983925140785,178.095925280538));
#31734=CARTESIAN_POINT('Ctrl Pts',(29.9473399467332,31.997818150837,178.854074719462));
#31735=CARTESIAN_POINT('Ctrl Pts',(29.9508762880376,32.4678823512929,178.828629953495));
#31736=CARTESIAN_POINT('Ctrl Pts',(30.3432698080826,33.6292029591439,178.766141924455));
#31737=CARTESIAN_POINT('Ctrl Pts',(32.2716026719728,34.4129388487757,178.666610632341));
#31738=CARTESIAN_POINT('Ctrl Pts',(34.1744105218922,33.0815150675564,178.555480843121));
#31739=CARTESIAN_POINT('Ctrl Pts',(34.0880401159474,30.7594177996359,178.444351053901));
#31740=CARTESIAN_POINT('Ctrl Pts',(32.0903159869838,29.5731212764253,178.333221264682));
#31741=CARTESIAN_POINT('Ctrl Pts',(30.2791368816166,30.4738805328492,178.236462486535));
#31742=CARTESIAN_POINT('Ctrl Pts',(29.9500603421358,31.5817357085946,178.176746971462));
#31743=CARTESIAN_POINT('Ctrl Pts',(29.94788119656,32.0011671080005,178.154074719462));
#31744=CARTESIAN_POINT('Ctrl Pts',(33.2690708798531,33.0793586530476,179.));
#31745=CARTESIAN_POINT('Ctrl Pts',(33.6279571482411,32.6573931542727,178.962956736927));
#31746=CARTESIAN_POINT('Ctrl Pts',(33.8850554700173,31.4341253615397,178.88887021078));
#31747=CARTESIAN_POINT('Ctrl Pts',(32.5454538370914,30.106758103338,178.777740421561));
#31748=CARTESIAN_POINT('Ctrl Pts',(30.7060860498309,30.5161310027492,178.666610632341));
#31749=CARTESIAN_POINT('Ctrl Pts',(30.0511744117699,32.2815518680592,178.555480843121));
#31750=CARTESIAN_POINT('Ctrl Pts',(31.1796675813394,33.7902651228869,178.444351053901));
#31751=CARTESIAN_POINT('Ctrl Pts',(33.0589884974179,33.6600730535175,178.333221264682));
#31752=CARTESIAN_POINT('Ctrl Pts',(33.9691010203833,32.0108329574877,178.222091475462));
#31753=CARTESIAN_POINT('Ctrl Pts',(33.0771301476877,30.3515643088587,178.110961686242));
#31754=CARTESIAN_POINT('Ctrl Pts',(31.1993733391997,30.2009822869226,177.999831897022));
#31755=CARTESIAN_POINT('Ctrl Pts',(30.0543453491064,31.6968141855763,177.888702107803));
#31756=CARTESIAN_POINT('Ctrl Pts',(30.6899574406665,33.4701319993115,177.777572318583));
#31757=CARTESIAN_POINT('Ctrl Pts',(32.5245072359045,33.8979942976083,177.666442529363));
#31758=CARTESIAN_POINT('Ctrl Pts',(33.8790332253115,32.5888360648699,177.555312740143));
#31759=CARTESIAN_POINT('Ctrl Pts',(33.5138886157823,30.7407798466014,177.444182950924));
#31760=CARTESIAN_POINT('Ctrl Pts',(31.7632494487822,30.0451490451179,177.333053161704));
#31761=CARTESIAN_POINT('Ctrl Pts',(30.2292818746669,31.1385762510273,177.221923372484));
#31762=CARTESIAN_POINT('Ctrl Pts',(30.3158562987823,33.0203693203293,177.110793583265));
#31763=CARTESIAN_POINT('Ctrl Pts',(31.9437407879485,33.9683313597554,176.999663794045));
#31764=CARTESIAN_POINT('Ctrl Pts',(33.6231130912609,33.114897930247,176.888534004825));
#31765=CARTESIAN_POINT('Ctrl Pts',(33.8170298986299,31.2411219830236,176.777404215605));
#31766=CARTESIAN_POINT('Ctrl Pts',(32.3480206460453,30.0618629783066,176.666274426386));
#31767=CARTESIAN_POINT('Ctrl Pts',(30.5605066731107,30.6563659521911,176.555144637166));
#31768=CARTESIAN_POINT('Ctrl Pts',(30.0904013819051,32.4805482381934,176.444014847946));
#31769=CARTESIAN_POINT('Ctrl Pts',(31.3679400374343,33.8649379866196,176.332885058727));
#31770=CARTESIAN_POINT('Ctrl Pts',(33.223933116206,33.5425567147453,176.221755269507));
#31771=CARTESIAN_POINT('Ctrl Pts',(33.9597958800734,31.808444265551,176.110625480287));
#31772=CARTESIAN_POINT('Ctrl Pts',(32.9020747075766,30.2496415473443,175.999495691067));
#31773=CARTESIAN_POINT('Ctrl Pts',(31.0187845453096,30.2927479030848,175.888365901848));
#31774=CARTESIAN_POINT('Ctrl Pts',(30.0334921263313,31.8983128635815,175.777236112628));
#31775=CARTESIAN_POINT('Ctrl Pts',(30.8479263874474,33.596940788559,175.666106323408));
#31776=CARTESIAN_POINT('Ctrl Pts',(32.7167259250522,33.834065821958,175.554976534188));
#31777=CARTESIAN_POINT('Ctrl Pts',(33.929585668619,32.3926737047122,175.443846744969));
#31778=CARTESIAN_POINT('Ctrl Pts',(33.3765095337505,30.5919108712851,175.332716955749));
#31779=CARTESIAN_POINT('Ctrl Pts',(31.563666801218,30.0798159383659,175.22158716653));
#31780=CARTESIAN_POINT('Ctrl Pts',(30.1501514803743,31.3250526351259,175.110457377309));
#31781=CARTESIAN_POINT('Ctrl Pts',(30.4295974639201,33.1879938407189,174.99932758809));
#31782=CARTESIAN_POINT('Ctrl Pts',(32.14625881818,33.963695966543,174.88819779887));
#31783=CARTESIAN_POINT('Ctrl Pts',(33.7290656881523,32.9422448391827,174.777068009651));
#31784=CARTESIAN_POINT('Ctrl Pts',(33.7294503912643,31.0584614532224,174.66593822043));
#31785=CARTESIAN_POINT('Ctrl Pts',(32.1470608513997,30.0363639347125,174.554808431211));
#31786=CARTESIAN_POINT('Ctrl Pts',(30.4300828151426,30.8113648484074,174.443678641991));
#31787=CARTESIAN_POINT('Ctrl Pts',(30.1498759614241,32.6741917626283,174.332548852772));
#31788=CARTESIAN_POINT('Ctrl Pts',(31.5628825640505,33.9200056869971,174.221419063552));
#31789=CARTESIAN_POINT('Ctrl Pts',(33.3759343037167,33.4086512282208,174.110289274332));
#31790=CARTESIAN_POINT('Ctrl Pts',(33.9297458900076,31.6081144415633,173.999159485112));
#31791=CARTESIAN_POINT('Ctrl Pts',(32.7174749649862,30.1662270681651,173.888029695893));
#31792=CARTESIAN_POINT('Ctrl Pts',(30.8485787327015,30.4025887955429,173.776899906673));
#31793=CARTESIAN_POINT('Ctrl Pts',(30.0334507576047,32.1008839340366,173.665770117453));
#31794=CARTESIAN_POINT('Ctrl Pts',(31.0180873228095,33.7068511901408,173.554640328233));
#31795=CARTESIAN_POINT('Ctrl Pts',(32.9013597217795,33.7507267470584,173.443510539014));
#31796=CARTESIAN_POINT('Ctrl Pts',(33.959717478216,32.1923561709092,173.332380749794));
#31797=CARTESIAN_POINT('Ctrl Pts',(33.2245630508403,30.4579433131597,173.221250960574));
#31798=CARTESIAN_POINT('Ctrl Pts',(31.3687017991688,30.134804012298,173.110121171354));
#31799=CARTESIAN_POINT('Ctrl Pts',(30.0905978147541,31.5186718521729,172.998991382135));
#31800=CARTESIAN_POINT('Ctrl Pts',(30.559958003672,33.3430459931528,172.887861592915));
#31801=CARTESIAN_POINT('Ctrl Pts',(32.347229011024,33.9382790059265,172.776731803695));
#31802=CARTESIAN_POINT('Ctrl Pts',(33.8167197930288,32.7596200922368,172.665602014476));
#31803=CARTESIAN_POINT('Ctrl Pts',(33.6235683219593,30.8857651078688,172.554472225256));
#31804=CARTESIAN_POINT('Ctrl Pts',(31.944544729498,30.0316458134051,172.443342436036));
#31805=CARTESIAN_POINT('Ctrl Pts',(30.3162731992128,30.9789429246006,172.332212646816));
#31806=CARTESIAN_POINT('Ctrl Pts',(30.2289301777512,32.8607003982989,172.221082857597));
#31807=CARTESIAN_POINT('Ctrl Pts',(31.7624510511593,33.954754201381,172.109953068377));
#31808=CARTESIAN_POINT('Ctrl Pts',(33.5133741464353,33.259838157786,171.998823279157));
#31809=CARTESIAN_POINT('Ctrl Pts',(33.879273634753,31.411931894561,171.887693489937));
#31810=CARTESIAN_POINT('Ctrl Pts',(32.5252822724187,30.1022191841008,171.776563700718));
#31811=CARTESIAN_POINT('Ctrl Pts',(30.6905582708158,30.5293348957756,171.665433911498));
#31812=CARTESIAN_POINT('Ctrl Pts',(30.0542211394581,32.3023873621376,171.554304122278));
#31813=CARTESIAN_POINT('Ctrl Pts',(31.1986397201752,33.7986981939257,171.443174333059));
#31814=CARTESIAN_POINT('Ctrl Pts',(33.0764545385976,33.6488599447027,171.332044543839));
#31815=CARTESIAN_POINT('Ctrl Pts',(33.9691098369589,31.9900029552293,171.220914754619));
#31816=CARTESIAN_POINT('Ctrl Pts',(33.0596571666423,30.3402951527166,171.109784965399));
#31817=CARTESIAN_POINT('Ctrl Pts',(31.1804177489182,30.2095312276882,170.99865517618));
#31818=CARTESIAN_POINT('Ctrl Pts',(30.0512511193847,31.7173849062541,170.88752538696));
#31819=CARTESIAN_POINT('Ctrl Pts',(30.7055583320888,33.4838848537833,170.77639559774));
#31820=CARTESIAN_POINT('Ctrl Pts',(32.5445245216298,33.8923494751911,170.665265808521));
#31821=CARTESIAN_POINT('Ctrl Pts',(33.8851477740978,32.5689563785795,170.554136019301));
#31822=CARTESIAN_POINT('Ctrl Pts',(33.5005042272877,30.724860574367,170.443006230081));
#31823=CARTESIAN_POINT('Ctrl Pts',(31.7426154839547,30.0477585441825,170.331876440861));
#31824=CARTESIAN_POINT('Ctrl Pts',(30.2202822584875,31.1573267231852,170.220746651642));
#31825=CARTESIAN_POINT('Ctrl Pts',(30.3267274098173,33.0381003467177,170.109616862422));
#31826=CARTESIAN_POINT('Ctrl Pts',(31.9645334897966,33.9688157906636,169.998487073202));
#31827=CARTESIAN_POINT('Ctrl Pts',(33.6347981352959,33.0976923739124,169.887357283982));
#31828=CARTESIAN_POINT('Ctrl Pts',(33.8089132560199,31.2219728005347,169.776227494763));
#31829=CARTESIAN_POINT('Ctrl Pts',(32.3275305816819,30.058295282754,169.665097705543));
#31830=CARTESIAN_POINT('Ctrl Pts',(30.5463954709098,30.671644865286,169.553967916323));
#31831=CARTESIAN_POINT('Ctrl Pts',(30.0955834614767,32.5006906616968,169.442838127103));
#31832=CARTESIAN_POINT('Ctrl Pts',(31.3876728155618,33.8715097942865,169.331708337884));
#31833=CARTESIAN_POINT('Ctrl Pts',(33.240157368435,33.5295434588245,169.220578548664));
#31834=CARTESIAN_POINT('Ctrl Pts',(33.9576633466589,31.7877555370529,169.109448759444));
#31835=CARTESIAN_POINT('Ctrl Pts',(32.883537060004,30.2402114460784,168.998318970225));
#31836=CARTESIAN_POINT('Ctrl Pts',(31.0008072375767,30.303206755534,168.887189181005));
#31837=CARTESIAN_POINT('Ctrl Pts',(30.03252779556,31.9190888413822,168.776059391785));
#31838=CARTESIAN_POINT('Ctrl Pts',(30.8648575786276,33.6090199421243,168.664929602565));
#31839=CARTESIAN_POINT('Ctrl Pts',(32.7360573957742,33.8263934409862,168.553799813346));
#31840=CARTESIAN_POINT('Ctrl Pts',(33.9336254662211,32.3722714689531,168.442670024126));
#31841=CARTESIAN_POINT('Ctrl Pts',(33.3615604798827,30.5774506858874,168.331540234906));
#31842=CARTESIAN_POINT('Ctrl Pts',(31.5434101066319,30.0845316077095,168.220410445687));
#31843=CARTESIAN_POINT('Ctrl Pts',(30.1431258547895,31.3446284307498,168.109280656467));
#31844=CARTESIAN_POINT('Ctrl Pts',(30.4422326785732,33.2045142047563,167.998150867247));
#31845=CARTESIAN_POINT('Ctrl Pts',(32.1669912720462,33.9620416450606,167.887021078027));
#31846=CARTESIAN_POINT('Ctrl Pts',(33.7389212431062,32.9239298409573,167.775891288808));
#31847=CARTESIAN_POINT('Ctrl Pts',(33.7194093934192,31.0402474829195,167.664761499588));
#31848=CARTESIAN_POINT('Ctrl Pts',(32.1263126252782,30.0349201860045,167.553631710368));
#31849=CARTESIAN_POINT('Ctrl Pts',(30.4176160910906,30.8280126945526,167.442501921148));
#31850=CARTESIAN_POINT('Ctrl Pts',(30.1570997860257,32.693695132644,167.331372131929));
#31851=CARTESIAN_POINT('Ctrl Pts',(31.5831865126735,33.9245155987673,167.220242342709));
#31852=CARTESIAN_POINT('Ctrl Pts',(33.3907349133656,33.3940396676622,167.109112553489));
#31853=CARTESIAN_POINT('Ctrl Pts',(33.9255008766017,31.5877549553105,166.997982764269));
#31854=CARTESIAN_POINT('Ctrl Pts',(32.6980630609426,30.1587499839622,166.88685297505));
#31855=CARTESIAN_POINT('Ctrl Pts',(30.8317782439138,30.4148420550124,166.77572318583));
#31856=CARTESIAN_POINT('Ctrl Pts',(30.0346113650038,32.1216433159453,166.66459339661));
#31857=CARTESIAN_POINT('Ctrl Pts',(31.0361996772909,33.7171386430304,166.553463607391));
#31858=CARTESIAN_POINT('Ctrl Pts',(32.9197400310435,33.741085137486,166.442333818171));
#31859=CARTESIAN_POINT('Ctrl Pts',(33.961763295132,32.1716952567886,166.331204028951));
#31860=CARTESIAN_POINT('Ctrl Pts',(33.2079561086236,30.4449968915186,166.220074239731));
#31861=CARTESIAN_POINT('Ctrl Pts',(31.3495488314203,30.1417767118191,166.108944450512));
#31862=CARTESIAN_POINT('Ctrl Pts',(30.0845739128819,31.5384507908558,165.997814661292));
#31863=CARTESIAN_POINT('Ctrl Pts',(30.5763936504527,33.3590412771596,165.886684872072));
#31864=CARTESIAN_POINT('Ctrl Pts',(31.7668777668633,33.7401334029928,165.812598345926));
#31865=CARTESIAN_POINT('Ctrl Pts',(32.3110796379513,33.6366995627946,165.775555082853));
#31866=CARTESIAN_POINT('Ctrl Pts',(33.3677806246596,33.1633123698088,179.074814972382));
#31867=CARTESIAN_POINT('Ctrl Pts',(33.754581466244,32.7085259251257,179.037771709309));
#31868=CARTESIAN_POINT('Ctrl Pts',(34.0316771814958,31.3901110026558,178.963685183163));
#31869=CARTESIAN_POINT('Ctrl Pts',(32.5878798433277,29.9594996424882,178.852555393943));
#31870=CARTESIAN_POINT('Ctrl Pts',(30.6054439833786,30.4007140214203,178.741425604723));
#31871=CARTESIAN_POINT('Ctrl Pts',(29.8995925895562,32.3034512855678,178.630295815504));
#31872=CARTESIAN_POINT('Ctrl Pts',(31.1158612132413,33.9295139357165,178.519166026284));
#31873=CARTESIAN_POINT('Ctrl Pts',(33.1413578008135,33.7891953823601,178.408036237064));
#31874=CARTESIAN_POINT('Ctrl Pts',(34.1222598882652,32.0116755569721,178.296906447844));
#31875=CARTESIAN_POINT('Ctrl Pts',(33.1609105288229,30.2233471470077,178.185776658625));
#31876=CARTESIAN_POINT('Ctrl Pts',(31.1370997068695,30.0610526878912,178.074646869405));
#31877=CARTESIAN_POINT('Ctrl Pts',(29.9030101659262,31.6732320556528,177.963517080185));
#31878=CARTESIAN_POINT('Ctrl Pts',(30.5880608730512,33.5844805016589,177.852387290966));
#31879=CARTESIAN_POINT('Ctrl Pts',(32.5653039921985,34.0456224054905,177.741257501746));
#31880=CARTESIAN_POINT('Ctrl Pts',(34.0251865198973,32.6346363890432,177.630127712526));
#31881=CARTESIAN_POINT('Ctrl Pts',(33.6316405564356,30.6428363022569,177.518997923306));
#31882=CARTESIAN_POINT('Ctrl Pts',(31.7448347275366,29.8930985631831,177.407868134087));
#31883=CARTESIAN_POINT('Ctrl Pts',(30.091553449052,31.0715737535457,177.296738344867));
#31884=CARTESIAN_POINT('Ctrl Pts',(30.1848617281844,33.0997347811692,177.185608555647));
#31885=CARTESIAN_POINT('Ctrl Pts',(31.9393648838499,34.1214303625775,177.074478766427));
#31886=CARTESIAN_POINT('Ctrl Pts',(33.7493606331233,33.2016159315242,176.963348977208));
#31887=CARTESIAN_POINT('Ctrl Pts',(33.9583605054912,31.1820956066532,176.852219187988));
#31888=CARTESIAN_POINT('Ctrl Pts',(32.3750900790485,29.9111125246884,176.741089398768));
#31889=CARTESIAN_POINT('Ctrl Pts',(30.4485412807881,30.5518566012337,176.629959609548));
#31890=CARTESIAN_POINT('Ctrl Pts',(29.9418706770663,32.5179258147436,176.518829820329));
#31891=CARTESIAN_POINT('Ctrl Pts',(31.318777710414,34.0099949378598,176.407700031109));
#31892=CARTESIAN_POINT('Ctrl Pts',(33.3191319955427,33.6625384920277,176.29657024189));
#31893=CARTESIAN_POINT('Ctrl Pts',(34.1122309837906,31.7935448474304,176.18544045267));
#31894=CARTESIAN_POINT('Ctrl Pts',(32.9722390818404,30.1134967197192,176.07431066345));
#31895=CARTESIAN_POINT('Ctrl Pts',(30.9424645156955,30.1599559357627,175.96318087423));
#31896=CARTESIAN_POINT('Ctrl Pts',(29.8805349562855,31.8904035249895,175.85205108501));
#31897=CARTESIAN_POINT('Ctrl Pts',(30.7583168202445,33.7211526196019,175.740921295791));
#31898=CARTESIAN_POINT('Ctrl Pts',(32.772473664821,33.9767215018872,175.629791506571));
#31899=CARTESIAN_POINT('Ctrl Pts',(34.079670988482,32.4232163022927,175.518661717351));
#31900=CARTESIAN_POINT('Ctrl Pts',(33.4835759765767,30.4823881324319,175.407531928132));
#31901=CARTESIAN_POINT('Ctrl Pts',(31.5297283196201,29.9304618859529,175.296402138912));
#31902=CARTESIAN_POINT('Ctrl Pts',(30.0062682046631,31.2725544782441,175.185272349692));
#31903=CARTESIAN_POINT('Ctrl Pts',(30.3074498076774,33.2803973232278,175.074142560472));
#31904=CARTESIAN_POINT('Ctrl Pts',(32.1576349917629,34.1164344233243,174.963012771253));
#31905=CARTESIAN_POINT('Ctrl Pts',(33.8635543408672,33.01553369097,174.851882982033));
#31906=CARTESIAN_POINT('Ctrl Pts',(33.8639689666152,30.9852275376442,174.740753192813));
#31907=CARTESIAN_POINT('Ctrl Pts',(32.1584994080186,29.8836301371174,174.629623403593));
#31908=CARTESIAN_POINT('Ctrl Pts',(30.307972910058,30.7189114840252,174.518493614374));
#31909=CARTESIAN_POINT('Ctrl Pts',(30.0059712555425,32.7266311479268,174.407363825154));
#31910=CARTESIAN_POINT('Ctrl Pts',(31.5288830836133,34.0693458652324,174.296234035934));
#31911=CARTESIAN_POINT('Ctrl Pts',(33.482956004511,33.5182176877988,174.185104246715));
#31912=CARTESIAN_POINT('Ctrl Pts',(34.0798436720685,31.5776331468769,174.073974457495));
#31913=CARTESIAN_POINT('Ctrl Pts',(32.7732809659143,30.0235941695556,173.962844668275));
#31914=CARTESIAN_POINT('Ctrl Pts',(30.7590199056383,30.2783403750282,173.851714879056));
#31915=CARTESIAN_POINT('Ctrl Pts',(29.8804903698533,32.1087307986539,173.740585089835));
#31916=CARTESIAN_POINT('Ctrl Pts',(30.9417130624539,33.839611974488,173.629455300616));
#31917=CARTESIAN_POINT('Ctrl Pts',(32.9714684836526,33.8869002210318,173.518325511396));
#31918=CARTESIAN_POINT('Ctrl Pts',(34.1121464837495,32.2073178478682,173.407195722176));
#31919=CARTESIAN_POINT('Ctrl Pts',(33.3198109271937,30.338000428604,173.296065932957));
#31920=CARTESIAN_POINT('Ctrl Pts',(31.3195987228237,29.9897269934467,173.184936143737));
#31921=CARTESIAN_POINT('Ctrl Pts',(29.9420823886808,31.4812336133839,173.073806354517));
#31922=CARTESIAN_POINT('Ctrl Pts',(30.4479499352301,33.447509604565,172.962676565297));
#31923=CARTESIAN_POINT('Ctrl Pts',(32.3742368697747,34.0890405032362,172.851546776078));
#31924=CARTESIAN_POINT('Ctrl Pts',(33.9580262795313,32.8187041880466,172.740416986858));
#31925=CARTESIAN_POINT('Ctrl Pts',(33.7498512721717,30.7990986784339,172.629287197638));
#31926=CARTESIAN_POINT('Ctrl Pts',(31.9402313568674,29.878545035086,172.518157408419));
#31927=CARTESIAN_POINT('Ctrl Pts',(30.1853110555941,30.8995239694063,172.407027619199));
#31928=CARTESIAN_POINT('Ctrl Pts',(30.091174396759,32.9276466327604,172.295897829979));
#31929=CARTESIAN_POINT('Ctrl Pts',(31.7439742296583,34.106797157721,172.184768040759));
#31930=CARTESIAN_POINT('Ctrl Pts',(33.6310860710905,33.3578297711992,172.07363825154));
#31931=CARTESIAN_POINT('Ctrl Pts',(34.0254456286525,31.3661913031266,171.96250846232));
#31932=CARTESIAN_POINT('Ctrl Pts',(32.566139311915,29.9546076810635,171.8513786731));
#31933=CARTESIAN_POINT('Ctrl Pts',(30.588708436438,30.414944927935,171.74024888388));
#31934=CARTESIAN_POINT('Ctrl Pts',(29.9028762951132,32.325907387554,171.629119094661));
#31935=CARTESIAN_POINT('Ctrl Pts',(31.1363090261413,33.938602940402,171.517989305441));
#31936=CARTESIAN_POINT('Ctrl Pts',(33.1601823701062,33.7771101054676,171.406859516221));
#31937=CARTESIAN_POINT('Ctrl Pts',(34.1222693906039,31.9892253739659,171.295729727002));
#31938=CARTESIAN_POINT('Ctrl Pts',(33.142078479874,30.2112014633646,171.184599937782));
#31939=CARTESIAN_POINT('Ctrl Pts',(31.1166697296889,30.0702665747797,171.073470148562));
#31940=CARTESIAN_POINT('Ctrl Pts',(29.8996752635746,31.6954027898688,170.962340359342));
#31941=CARTESIAN_POINT('Ctrl Pts',(30.6048752191635,33.5993030684508,170.851210570123));
#31942=CARTESIAN_POINT('Ctrl Pts',(32.5868782446758,34.0395385225061,170.740080780903));
#31943=CARTESIAN_POINT('Ctrl Pts',(34.0317766650903,32.6132104386381,170.628950991683));
#31944=CARTESIAN_POINT('Ctrl Pts',(33.6172151153146,30.6256788113188,170.517821202463));
#31945=CARTESIAN_POINT('Ctrl Pts',(31.7225958299706,29.8959110319878,170.406691413244));
#31946=CARTESIAN_POINT('Ctrl Pts',(30.0818538327146,31.0917826582869,170.295561624024));
#31947=CARTESIAN_POINT('Ctrl Pts',(30.1965784063291,33.1188449465149,170.184431834804));
#31948=CARTESIAN_POINT('Ctrl Pts',(31.9617748651785,34.1219524730606,170.073302045585));
#31949=CARTESIAN_POINT('Ctrl Pts',(33.7619545528822,33.1830721078777,169.962172256365));
#31950=CARTESIAN_POINT('Ctrl Pts',(33.9496125413895,31.1614569794478,169.851042467145));
#31951=CARTESIAN_POINT('Ctrl Pts',(32.3530062746849,29.907267329807,169.739912677925));
#31952=CARTESIAN_POINT('Ctrl Pts',(30.433332493582,30.5683239251859,169.628782888706));
#31953=CARTESIAN_POINT('Ctrl Pts',(29.9474558245518,32.5396349383544,169.517653099486));
#31954=CARTESIAN_POINT('Ctrl Pts',(31.3400453259759,34.0170779080377,169.406523310266));
#31955=CARTESIAN_POINT('Ctrl Pts',(33.3366181881587,33.6485130505849,169.295393521047));
#31956=CARTESIAN_POINT('Ctrl Pts',(34.1099325795548,31.7712469266146,169.184263731827));
#31957=CARTESIAN_POINT('Ctrl Pts',(32.9522595554175,30.1033331346864,169.073133942607));
#31958=CARTESIAN_POINT('Ctrl Pts',(30.9230889129684,30.1712282893903,168.962004153387));
#31959=CARTESIAN_POINT('Ctrl Pts',(29.8794956187941,31.9127954814557,168.850874364168));
#31960=CARTESIAN_POINT('Ctrl Pts',(30.7765649383097,33.7341713031689,168.739744574948));
#31961=CARTESIAN_POINT('Ctrl Pts',(32.7933087588409,33.9684523545883,168.628614785728));
#31962=CARTESIAN_POINT('Ctrl Pts',(34.0840250060357,32.4012271579398,168.517484996508));
#31963=CARTESIAN_POINT('Ctrl Pts',(33.4674641686691,30.4668032177279,168.406355207289));
#31964=CARTESIAN_POINT('Ctrl Pts',(31.5078960367946,29.9355443453039,168.295225418069));
#31965=CARTESIAN_POINT('Ctrl Pts',(29.9986961181047,31.2936529010287,168.184095628849));
#31966=CARTESIAN_POINT('Ctrl Pts',(30.3210678033822,33.298202659558,168.07296583963));
#31967=CARTESIAN_POINT('Ctrl Pts',(32.1799800389545,34.1146514268768,167.96183605041));
#31968=CARTESIAN_POINT('Ctrl Pts',(33.8741764718491,32.9957941318081,167.85070626119));
#31969=CARTESIAN_POINT('Ctrl Pts',(33.8531469687877,30.9655968644692,167.73957647197));
#31970=CARTESIAN_POINT('Ctrl Pts',(32.1361373617882,29.8820740920287,167.628446682751));
#31971=CARTESIAN_POINT('Ctrl Pts',(30.2945365103406,30.7368542181635,167.517316893531));
#31972=CARTESIAN_POINT('Ctrl Pts',(30.0137569572577,32.7476515117587,167.406187104311));
#31973=CARTESIAN_POINT('Ctrl Pts',(31.5507662959473,34.0742065629572,167.295057315091));
#31974=CARTESIAN_POINT('Ctrl Pts',(33.4989078220432,33.5024696238054,167.183927525872));
#31975=CARTESIAN_POINT('Ctrl Pts',(34.0752684767976,31.5556900771347,167.072797736652));
#31976=CARTESIAN_POINT('Ctrl Pts',(32.7523591823794,30.0155355094255,166.961667947433));
#31977=CARTESIAN_POINT('Ctrl Pts',(30.740912656143,30.2915467066502,166.850538158212));
#31978=CARTESIAN_POINT('Ctrl Pts',(29.8817412505871,32.1311048683811,166.739408368993));
#31979=CARTESIAN_POINT('Ctrl Pts',(30.9612342160158,33.8506995969076,166.628278579773));
#31980=CARTESIAN_POINT('Ctrl Pts',(32.9912784338182,33.8765086763411,166.517148790554));
#31981=CARTESIAN_POINT('Ctrl Pts',(34.1143514265811,32.1850499048632,166.406019001334));
#31982=CARTESIAN_POINT('Ctrl Pts',(33.3019122785371,30.3240470198856,166.294889212114));
#31983=CARTESIAN_POINT('Ctrl Pts',(31.298956015937,29.9972420372932,166.183759422894));
#31984=CARTESIAN_POINT('Ctrl Pts',(29.9355899410197,31.5025509799206,166.072629633675));
#31985=CARTESIAN_POINT('Ctrl Pts',(30.4656639649012,33.4647490195557,165.961499844455));
#31986=CARTESIAN_POINT('Ctrl Pts',(31.7487452602343,33.8754829148802,165.887413318308));
#31987=CARTESIAN_POINT('Ctrl Pts',(32.3352757582502,33.764003875527,165.850370055235));
#31988=CARTESIAN_POINT('Ctrl Pts',(33.4664903694662,33.2472660865699,179.149629944765));
#31989=CARTESIAN_POINT('Ctrl Pts',(33.881205784247,32.7596586959787,179.112586681692));
#31990=CARTESIAN_POINT('Ctrl Pts',(34.1782988929742,31.3460966437719,179.038500155545));
#31991=CARTESIAN_POINT('Ctrl Pts',(32.6303058495641,29.8122411816384,178.927370366326));
#31992=CARTESIAN_POINT('Ctrl Pts',(30.5048019169264,30.2852970400916,178.816240577106));
#31993=CARTESIAN_POINT('Ctrl Pts',(29.7480107673423,32.3253507030764,178.705110787886));
#31994=CARTESIAN_POINT('Ctrl Pts',(31.0520548451432,34.0687627485461,178.593980998666));
#31995=CARTESIAN_POINT('Ctrl Pts',(33.2237271042091,33.9183177112026,178.482851209447));
#31996=CARTESIAN_POINT('Ctrl Pts',(34.2754187561472,32.0125181564566,178.371721420227));
#31997=CARTESIAN_POINT('Ctrl Pts',(33.244690909958,30.0951299851567,178.260591631007));
#31998=CARTESIAN_POINT('Ctrl Pts',(31.0748260745393,29.9211230888598,178.149461841787));
#31999=CARTESIAN_POINT('Ctrl Pts',(29.7516749827459,31.6496499257294,178.038332052568));
#32000=CARTESIAN_POINT('Ctrl Pts',(30.486164305436,33.6988290040063,177.927202263348));
#32001=CARTESIAN_POINT('Ctrl Pts',(32.6061007484926,34.1932505133727,177.816072474128));
#32002=CARTESIAN_POINT('Ctrl Pts',(34.1713398144831,32.6804367132165,177.704942684908));
#32003=CARTESIAN_POINT('Ctrl Pts',(33.7493924970889,30.5448927579124,177.593812895689));
#32004=CARTESIAN_POINT('Ctrl Pts',(31.7264200062909,29.7410480812482,177.482683106469));
#32005=CARTESIAN_POINT('Ctrl Pts',(29.9538250234371,31.0045712560641,177.371553317249));
#32006=CARTESIAN_POINT('Ctrl Pts',(30.0538671575865,33.1791002420091,177.26042352803));
#32007=CARTESIAN_POINT('Ctrl Pts',(31.9349889797512,34.2745293653997,177.14929373881));
#32008=CARTESIAN_POINT('Ctrl Pts',(33.8756081749856,33.2883339328014,177.03816394959));
#32009=CARTESIAN_POINT('Ctrl Pts',(34.0996911123523,31.1230692302828,176.92703416037));
#32010=CARTESIAN_POINT('Ctrl Pts',(32.4021595120518,29.7603620710703,176.815904371151));
#32011=CARTESIAN_POINT('Ctrl Pts',(30.3365758884656,30.4473472502762,176.704774581931));
#32012=CARTESIAN_POINT('Ctrl Pts',(29.7933399722275,32.5553033912937,176.593644792711));
#32013=CARTESIAN_POINT('Ctrl Pts',(31.2696153833937,34.1550518891,176.482515003491));
#32014=CARTESIAN_POINT('Ctrl Pts',(33.4143308748795,33.78252026931,176.371385214272));
#32015=CARTESIAN_POINT('Ctrl Pts',(34.2646660875078,31.7786454293097,176.260255425052));
#32016=CARTESIAN_POINT('Ctrl Pts',(33.0424034561043,29.9773518920942,176.149125635832));
#32017=CARTESIAN_POINT('Ctrl Pts',(30.8661444860815,30.0271639684406,176.037995846613));
#32018=CARTESIAN_POINT('Ctrl Pts',(29.7275777862398,31.8824941863976,175.926866057393));
#32019=CARTESIAN_POINT('Ctrl Pts',(30.6687072530417,33.8453644506448,175.815736268173));
#32020=CARTESIAN_POINT('Ctrl Pts',(32.8282214045897,34.1193771818164,175.704606478953));
#32021=CARTESIAN_POINT('Ctrl Pts',(34.2297563083451,32.4537588998731,175.593476689734));
#32022=CARTESIAN_POINT('Ctrl Pts',(33.590642419403,30.3728653935788,175.482346900514));
#32023=CARTESIAN_POINT('Ctrl Pts',(31.4957898380222,29.7811078335399,175.371217111294));
#32024=CARTESIAN_POINT('Ctrl Pts',(29.8623849289518,31.2200563213624,175.260087322075));
#32025=CARTESIAN_POINT('Ctrl Pts',(30.1853021514348,33.3728008057367,175.148957532855));
#32026=CARTESIAN_POINT('Ctrl Pts',(32.1690111653458,34.2691728801058,175.037827743635));
#32027=CARTESIAN_POINT('Ctrl Pts',(33.9980429935822,33.0888225427571,174.926697954415));
#32028=CARTESIAN_POINT('Ctrl Pts',(33.9984875419661,30.911993622066,174.815568165196));
#32029=CARTESIAN_POINT('Ctrl Pts',(32.1699379646376,29.7308963395222,174.704438375976));
#32030=CARTESIAN_POINT('Ctrl Pts',(30.1858630049732,30.6264581196432,174.593308586756));
#32031=CARTESIAN_POINT('Ctrl Pts',(29.8620665496609,32.7790705332252,174.482178797537));
#32032=CARTESIAN_POINT('Ctrl Pts',(31.494883603176,34.2186860434678,174.371049008317));
#32033=CARTESIAN_POINT('Ctrl Pts',(33.5899777053053,33.6277841473768,174.259919219097));
#32034=CARTESIAN_POINT('Ctrl Pts',(34.2299414541294,31.5471518521906,174.148789429877));
#32035=CARTESIAN_POINT('Ctrl Pts',(32.8290869668423,29.8809612709459,174.037659640658));
#32036=CARTESIAN_POINT('Ctrl Pts',(30.669461078575,30.1540919545135,173.926529851438));
#32037=CARTESIAN_POINT('Ctrl Pts',(29.727529982102,32.116577663271,173.815400062218));
#32038=CARTESIAN_POINT('Ctrl Pts',(30.8653388020982,33.9723727588352,173.704270272998));
#32039=CARTESIAN_POINT('Ctrl Pts',(33.0415772455258,34.0230736950052,173.593140483779));
#32040=CARTESIAN_POINT('Ctrl Pts',(34.2645754892831,32.2222795248272,173.482010694559));
#32041=CARTESIAN_POINT('Ctrl Pts',(33.4150588035471,30.2180575440483,173.370880905339));
#32042=CARTESIAN_POINT('Ctrl Pts',(31.2704956464786,29.8446499745953,173.259751116119));
#32043=CARTESIAN_POINT('Ctrl Pts',(29.7935669626075,31.4437953745948,173.1486213269));
#32044=CARTESIAN_POINT('Ctrl Pts',(30.3359418667882,33.5519732159772,173.03749153768));
#32045=CARTESIAN_POINT('Ctrl Pts',(32.4012447285253,34.239802000546,172.92636174846));
#32046=CARTESIAN_POINT('Ctrl Pts',(34.0993327660339,32.8777882838563,172.81523195924));
#32047=CARTESIAN_POINT('Ctrl Pts',(33.8761342223841,30.7124322489989,172.704102170021));
#32048=CARTESIAN_POINT('Ctrl Pts',(31.9359179842369,29.7254442567669,172.592972380801));
#32049=CARTESIAN_POINT('Ctrl Pts',(30.0543489119754,30.8201050142119,172.481842591581));
#32050=CARTESIAN_POINT('Ctrl Pts',(29.9534186157667,32.9945928672219,172.370712802362));
#32051=CARTESIAN_POINT('Ctrl Pts',(31.7254974081573,34.2588401140609,172.259583013142));
#32052=CARTESIAN_POINT('Ctrl Pts',(33.7487979957457,33.4558213846124,172.148453223922));
#32053=CARTESIAN_POINT('Ctrl Pts',(34.1716176225522,31.3204507116921,172.037323434703));
#32054=CARTESIAN_POINT('Ctrl Pts',(32.6069963514114,29.8069961780261,171.926193645483));
#32055=CARTESIAN_POINT('Ctrl Pts',(30.4868586020602,30.3005549600944,171.815063856263));
#32056=CARTESIAN_POINT('Ctrl Pts',(29.7515314507684,32.3494274129703,171.703934067043));
#32057=CARTESIAN_POINT('Ctrl Pts',(31.0739783321073,34.0785076868783,171.592804277824));
#32058=CARTESIAN_POINT('Ctrl Pts',(33.2439102016148,33.9053602662325,171.481674488604));
#32059=CARTESIAN_POINT('Ctrl Pts',(34.2754289442489,31.9884477927025,171.370544699384));
#32060=CARTESIAN_POINT('Ctrl Pts',(33.2244997931058,30.0821077740126,171.259414910164));
#32061=CARTESIAN_POINT('Ctrl Pts',(31.0529217104596,29.9310019218713,171.148285120945));
#32062=CARTESIAN_POINT('Ctrl Pts',(29.7480994077644,31.6734206734835,171.037155331725));
#32063=CARTESIAN_POINT('Ctrl Pts',(30.5041921062382,33.7147212831184,170.926025542505));
#32064=CARTESIAN_POINT('Ctrl Pts',(32.6292319677217,34.1867275698212,170.814895753286));
#32065=CARTESIAN_POINT('Ctrl Pts',(34.1784055560829,32.6574644986967,170.703765964066));
#32066=CARTESIAN_POINT('Ctrl Pts',(33.7339260033414,30.5264970482706,170.592636174846));
#32067=CARTESIAN_POINT('Ctrl Pts',(31.7025761759865,29.7440635197931,170.481506385626));
#32068=CARTESIAN_POINT('Ctrl Pts',(29.9434254069416,31.0262385933886,170.370376596407));
#32069=CARTESIAN_POINT('Ctrl Pts',(30.0664294028411,33.1995895463121,170.259246807187));
#32070=CARTESIAN_POINT('Ctrl Pts',(31.9590162405603,34.2750891554577,170.148117017967));
#32071=CARTESIAN_POINT('Ctrl Pts',(33.8891109704685,33.2684518418429,170.036987228747));
#32072=CARTESIAN_POINT('Ctrl Pts',(34.0903118267592,31.1009411583609,169.925857439528));
#32073=CARTESIAN_POINT('Ctrl Pts',(32.3784819676879,29.7562393768599,169.814727650308));
#32074=CARTESIAN_POINT('Ctrl Pts',(30.3202695162544,30.4650029850859,169.703597861088));
#32075=CARTESIAN_POINT('Ctrl Pts',(29.7993281876268,32.578579215012,169.592468071868));
#32076=CARTESIAN_POINT('Ctrl Pts',(31.29241783639,34.162646021789,169.481338282649));
#32077=CARTESIAN_POINT('Ctrl Pts',(33.4330790078824,33.7674826423452,169.370208493429));
#32078=CARTESIAN_POINT('Ctrl Pts',(34.2622018124507,31.7547383161762,169.259078704209));
#32079=CARTESIAN_POINT('Ctrl Pts',(33.020982050831,29.9664548232945,169.14794891499));
#32080=CARTESIAN_POINT('Ctrl Pts',(30.8453705883601,30.0392498232466,169.03681912577));
#32081=CARTESIAN_POINT('Ctrl Pts',(29.7264634420282,31.9065021215292,168.92568933655));
#32082=CARTESIAN_POINT('Ctrl Pts',(30.6882722979918,33.8593226642135,168.81455954733));
#32083=CARTESIAN_POINT('Ctrl Pts',(32.8505601219075,34.1105112681904,168.703429758111));
#32084=CARTESIAN_POINT('Ctrl Pts',(34.2344245458504,32.4301828469265,168.592299968891));
#32085=CARTESIAN_POINT('Ctrl Pts',(33.5733678574555,30.3561557495683,168.481170179671));
#32086=CARTESIAN_POINT('Ctrl Pts',(31.4723819669573,29.7865570828984,168.370040390452));
#32087=CARTESIAN_POINT('Ctrl Pts',(29.8542663814199,31.2426773713076,168.258910601232));
#32088=CARTESIAN_POINT('Ctrl Pts',(30.1999029281912,33.3918911143597,168.147780812012));
#32089=CARTESIAN_POINT('Ctrl Pts',(32.1929688058628,34.267261208693,168.036651022792));
#32090=CARTESIAN_POINT('Ctrl Pts',(34.0094317005922,33.0676584226589,167.925521233573));
#32091=CARTESIAN_POINT('Ctrl Pts',(33.9868845441562,30.8909462460187,167.814391444353));
#32092=CARTESIAN_POINT('Ctrl Pts',(32.1459620982981,29.729227998053,167.703261655133));
#32093=CARTESIAN_POINT('Ctrl Pts',(30.1714569295906,30.6456957417745,167.592131865913));
#32094=CARTESIAN_POINT('Ctrl Pts',(29.8704141284897,32.8016078908734,167.481002076694));
#32095=CARTESIAN_POINT('Ctrl Pts',(31.5183460792209,34.2238975271471,167.369872287474));
#32096=CARTESIAN_POINT('Ctrl Pts',(33.6070807307209,33.6108995799486,167.258742498254));
#32097=CARTESIAN_POINT('Ctrl Pts',(34.2250360769934,31.5236251989588,167.147612709034));
#32098=CARTESIAN_POINT('Ctrl Pts',(32.8066553038163,29.8723210348887,167.036482919815));
#32099=CARTESIAN_POINT('Ctrl Pts',(30.6500470683722,30.1682513582881,166.925353130595));
#32100=CARTESIAN_POINT('Ctrl Pts',(29.7288711361704,32.1405664208168,166.814223341375));
#32101=CARTESIAN_POINT('Ctrl Pts',(30.8862687547407,33.9842605507847,166.703093552155));
#32102=CARTESIAN_POINT('Ctrl Pts',(33.0628168365929,34.0119322151961,166.591963762936));
#32103=CARTESIAN_POINT('Ctrl Pts',(34.2669395580302,32.1984045529377,166.480833973716));
#32104=CARTESIAN_POINT('Ctrl Pts',(33.3958684484506,30.2030971482525,166.369704184496));
#32105=CARTESIAN_POINT('Ctrl Pts',(31.2483632004537,29.8527073627674,166.258574395277));
#32106=CARTESIAN_POINT('Ctrl Pts',(29.7866059691575,31.4666511689852,166.147444606057));
#32107=CARTESIAN_POINT('Ctrl Pts',(30.3549342793497,33.5704567619518,166.036314816837));
#32108=CARTESIAN_POINT('Ctrl Pts',(31.7306127536053,34.0108324267677,165.962228290691));
#32109=CARTESIAN_POINT('Ctrl Pts',(32.359471878549,33.8913081882594,165.925185027618));
#32110=CARTESIAN_POINT('Ctrl Pts',(33.5652001142727,33.3312198033311,179.224444917147));
#32111=CARTESIAN_POINT('Ctrl Pts',(34.0078301022499,32.8107914668318,179.187401654074));
#32112=CARTESIAN_POINT('Ctrl Pts',(34.3249206044526,31.3020822848881,179.113315127928));
#32113=CARTESIAN_POINT('Ctrl Pts',(32.6727318558004,29.6649827207885,179.002185338708));
#32114=CARTESIAN_POINT('Ctrl Pts',(30.4041598504741,30.1698800587628,178.891055549488));
#32115=CARTESIAN_POINT('Ctrl Pts',(29.5964289451286,32.347250120585,178.779925760269));
#32116=CARTESIAN_POINT('Ctrl Pts',(30.9882484770451,34.2080115613757,178.668795971049));
#32117=CARTESIAN_POINT('Ctrl Pts',(33.3060964076047,34.0474400400451,178.557666181829));
#32118=CARTESIAN_POINT('Ctrl Pts',(34.4285776240291,32.013360755941,178.446536392609));
#32119=CARTESIAN_POINT('Ctrl Pts',(33.3284712910932,29.9669128233058,178.33540660339));
#32120=CARTESIAN_POINT('Ctrl Pts',(31.0125524422092,29.7811934898284,178.22427681417));
#32121=CARTESIAN_POINT('Ctrl Pts',(29.6003397995657,31.626067795806,178.11314702495));
#32122=CARTESIAN_POINT('Ctrl Pts',(30.3842677378208,33.8131775063538,178.002017235731));
#32123=CARTESIAN_POINT('Ctrl Pts',(32.6468975047867,34.3408786212549,177.890887446511));
#32124=CARTESIAN_POINT('Ctrl Pts',(34.3174931090689,32.7262370373898,177.779757657291));
#32125=CARTESIAN_POINT('Ctrl Pts',(33.8671444377423,30.4469492135679,177.668627868071));
#32126=CARTESIAN_POINT('Ctrl Pts',(31.7080052850452,29.5889975993134,177.557498078852));
#32127=CARTESIAN_POINT('Ctrl Pts',(29.8160965978222,30.9375687585825,177.446368289632));
#32128=CARTESIAN_POINT('Ctrl Pts',(29.9228725869886,33.2584657028491,177.335238500412));
#32129=CARTESIAN_POINT('Ctrl Pts',(31.9306130756526,34.4276283682218,177.224108711192));
#32130=CARTESIAN_POINT('Ctrl Pts',(34.0018557168478,33.3750519340786,177.112978921973));
#32131=CARTESIAN_POINT('Ctrl Pts',(34.2410217192136,31.0640428539123,177.001849132753));
#32132=CARTESIAN_POINT('Ctrl Pts',(32.429228945055,29.6096116174522,176.890719343533));
#32133=CARTESIAN_POINT('Ctrl Pts',(30.224610496143,30.3428378993186,176.779589554313));
#32134=CARTESIAN_POINT('Ctrl Pts',(29.6448092673887,32.5926809678439,176.668459765094));
#32135=CARTESIAN_POINT('Ctrl Pts',(31.2204530563734,34.3001088403402,176.557329975874));
#32136=CARTESIAN_POINT('Ctrl Pts',(33.5095297542162,33.9025020465923,176.446200186654));
#32137=CARTESIAN_POINT('Ctrl Pts',(34.417101191225,31.7637460111891,176.335070397435));
#32138=CARTESIAN_POINT('Ctrl Pts',(33.112567830368,29.8412070644691,176.223940608215));
#32139=CARTESIAN_POINT('Ctrl Pts',(30.7898244564675,29.8943720011186,176.112810818995));
#32140=CARTESIAN_POINT('Ctrl Pts',(29.574620616194,31.8745848478056,176.001681029775));
#32141=CARTESIAN_POINT('Ctrl Pts',(30.5790976858388,33.9695762816876,175.890551240556));
#32142=CARTESIAN_POINT('Ctrl Pts',(32.8839691443584,34.2620328617456,175.779421451336));
#32143=CARTESIAN_POINT('Ctrl Pts',(34.3798416282082,32.4843014974535,175.668291662116));
#32144=CARTESIAN_POINT('Ctrl Pts',(33.6977088622292,30.2633426547257,175.557161872896));
#32145=CARTESIAN_POINT('Ctrl Pts',(31.4618513564243,29.6317537811269,175.446032083677));
#32146=CARTESIAN_POINT('Ctrl Pts',(29.7185016532407,31.1675581644807,175.334902294457));
#32147=CARTESIAN_POINT('Ctrl Pts',(30.063154495192,33.4652042882456,175.223772505237));
#32148=CARTESIAN_POINT('Ctrl Pts',(32.1803873389287,34.4219113368872,175.112642716017));
#32149=CARTESIAN_POINT('Ctrl Pts',(34.1325316462971,33.1621113945443,175.001512926798));
#32150=CARTESIAN_POINT('Ctrl Pts',(34.1330061173171,30.8387597064878,174.890383137578));
#32151=CARTESIAN_POINT('Ctrl Pts',(32.1813765212566,29.578162541927,174.779253348358));
#32152=CARTESIAN_POINT('Ctrl Pts',(30.0637530998886,30.5340047552611,174.668123559139));
#32153=CARTESIAN_POINT('Ctrl Pts',(29.7181618437792,32.8315099185237,174.556993769919));
#32154=CARTESIAN_POINT('Ctrl Pts',(31.4608841227388,34.3680262217031,174.445863980699));
#32155=CARTESIAN_POINT('Ctrl Pts',(33.6969994060995,33.7373506069548,174.33473419148));
#32156=CARTESIAN_POINT('Ctrl Pts',(34.3800392361903,31.5166705575043,174.22360440226));
#32157=CARTESIAN_POINT('Ctrl Pts',(32.8848929677704,29.7383283723363,174.11247461304));
#32158=CARTESIAN_POINT('Ctrl Pts',(30.5799022515117,30.0298435339987,174.00134482382));
#32159=CARTESIAN_POINT('Ctrl Pts',(29.5745695943507,32.1244245278882,173.890215034601));
#32160=CARTESIAN_POINT('Ctrl Pts',(30.7889645417425,34.1051335431823,173.779085245381));
#32161=CARTESIAN_POINT('Ctrl Pts',(33.1116860073988,34.1592471689786,173.667955456161));
#32162=CARTESIAN_POINT('Ctrl Pts',(34.4170044948166,32.2372412017861,173.556825666941));
#32163=CARTESIAN_POINT('Ctrl Pts',(33.5103066799004,30.0981146594927,173.445695877722));
#32164=CARTESIAN_POINT('Ctrl Pts',(31.2213925701334,29.6995729557439,173.334566088502));
#32165=CARTESIAN_POINT('Ctrl Pts',(29.6450515365342,31.4063571358058,173.223436299282));
#32166=CARTESIAN_POINT('Ctrl Pts',(30.2239337983464,33.6564368273894,173.112306510062));
#32167=CARTESIAN_POINT('Ctrl Pts',(32.4282525872759,34.3905634978557,173.001176720843));
#32168=CARTESIAN_POINT('Ctrl Pts',(34.2406392525365,32.936872379666,172.890046931623));
#32169=CARTESIAN_POINT('Ctrl Pts',(34.0024171725965,30.6257658195639,172.778917142403));
#32170=CARTESIAN_POINT('Ctrl Pts',(31.9316046116063,29.5723434784478,172.667787353184));
#32171=CARTESIAN_POINT('Ctrl Pts',(29.9233867683568,30.7406860590175,172.556657563964));
#32172=CARTESIAN_POINT('Ctrl Pts',(29.8156628347745,33.0615391016834,172.445527774744));
#32173=CARTESIAN_POINT('Ctrl Pts',(31.7070205866564,34.4108830704008,172.334397985525));
#32174=CARTESIAN_POINT('Ctrl Pts',(33.8665099204009,33.5538129980256,172.223268196305));
#32175=CARTESIAN_POINT('Ctrl Pts',(34.3177896164518,31.2747101202577,172.112138407085));
#32176=CARTESIAN_POINT('Ctrl Pts',(32.6478533909077,29.6593846749887,172.001008617865));
#32177=CARTESIAN_POINT('Ctrl Pts',(30.3850087676824,30.1861649922538,171.889878828646));
#32178=CARTESIAN_POINT('Ctrl Pts',(29.6001866064235,32.3729474383867,171.778749039426));
#32179=CARTESIAN_POINT('Ctrl Pts',(31.0116476380733,34.2184124333546,171.667619250206));
#32180=CARTESIAN_POINT('Ctrl Pts',(33.3276380331233,34.0336104269975,171.556489460986));
#32181=CARTESIAN_POINT('Ctrl Pts',(34.4285884978939,31.987670211439,171.445359671767));
#32182=CARTESIAN_POINT('Ctrl Pts',(33.3069211063375,29.9530140846606,171.334229882547));
#32183=CARTESIAN_POINT('Ctrl Pts',(30.9891736912303,29.7917372689629,171.223100093327));
#32184=CARTESIAN_POINT('Ctrl Pts',(29.5965235519542,31.6514385570982,171.111970304107));
#32185=CARTESIAN_POINT('Ctrl Pts',(30.403508993313,33.8301394977859,171.000840514888));
#32186=CARTESIAN_POINT('Ctrl Pts',(32.6715856907677,34.3339166171362,170.889710725668));
#32187=CARTESIAN_POINT('Ctrl Pts',(34.3250344470753,32.7017185587553,170.778580936448));
#32188=CARTESIAN_POINT('Ctrl Pts',(33.8506368913683,30.4273152852224,170.667451147229));
#32189=CARTESIAN_POINT('Ctrl Pts',(31.6825565220024,29.5922160075984,170.556321358009));
#32190=CARTESIAN_POINT('Ctrl Pts',(29.8049969811687,30.9606945284903,170.445191568789));
#32191=CARTESIAN_POINT('Ctrl Pts',(29.9362803993529,33.2803341461093,170.334061779569));
#32192=CARTESIAN_POINT('Ctrl Pts',(31.9562576159421,34.4282258378547,170.22293199035));
#32193=CARTESIAN_POINT('Ctrl Pts',(34.0162673880548,33.3538315758082,170.11180220113));
#32194=CARTESIAN_POINT('Ctrl Pts',(34.2310111121289,31.0404253372741,170.00067241191));
#32195=CARTESIAN_POINT('Ctrl Pts',(32.4039576606909,29.6052114239129,169.88954262269));
#32196=CARTESIAN_POINT('Ctrl Pts',(30.2072065389267,30.3616820449858,169.778412833471));
#32197=CARTESIAN_POINT('Ctrl Pts',(29.6512005507019,32.6175234916696,169.667283044251));
#32198=CARTESIAN_POINT('Ctrl Pts',(31.2447903468041,34.3082141355403,169.556153255031));
#32199=CARTESIAN_POINT('Ctrl Pts',(33.5295398276061,33.8864522341055,169.445023465811));
#32200=CARTESIAN_POINT('Ctrl Pts',(34.4144710453466,31.738229705738,169.333893676592));
#32201=CARTESIAN_POINT('Ctrl Pts',(33.0897045462445,29.8295765119025,169.222763887372));
#32202=CARTESIAN_POINT('Ctrl Pts',(30.7676522637518,29.9072713571029,169.111634098153));
#32203=CARTESIAN_POINT('Ctrl Pts',(29.5734312652623,31.9002087616026,169.000504308933));
#32204=CARTESIAN_POINT('Ctrl Pts',(30.599979657674,33.9844740252581,168.889374519713));
#32205=CARTESIAN_POINT('Ctrl Pts',(32.9078114849742,34.2525701817925,168.778244730493));
#32206=CARTESIAN_POINT('Ctrl Pts',(34.384824085665,32.4591385359132,168.667114941273));
#32207=CARTESIAN_POINT('Ctrl Pts',(33.6792715462419,30.2455082814088,168.555985152054));
#32208=CARTESIAN_POINT('Ctrl Pts',(31.43686789712,29.6375698204928,168.444855362834));
#32209=CARTESIAN_POINT('Ctrl Pts',(29.7098366447351,31.1917018415865,168.333725573614));
#32210=CARTESIAN_POINT('Ctrl Pts',(30.0787380530001,33.4855795691615,168.222595784395));
#32211=CARTESIAN_POINT('Ctrl Pts',(32.2059575727712,34.4198709905092,168.111465995175));
#32212=CARTESIAN_POINT('Ctrl Pts',(34.1446869293352,33.1395227135096,168.000336205955));
#32213=CARTESIAN_POINT('Ctrl Pts',(34.1206221195246,30.8162956275684,167.889206416735));
#32214=CARTESIAN_POINT('Ctrl Pts',(32.1557868348082,29.5763819040772,167.778076627516));
#32215=CARTESIAN_POINT('Ctrl Pts',(30.0483773488405,30.5545372653854,167.666946838296));
#32216=CARTESIAN_POINT('Ctrl Pts',(29.7270712997217,32.8555642699881,167.555817049076));
#32217=CARTESIAN_POINT('Ctrl Pts',(31.4859258624946,34.3735884913369,167.444687259856));
#32218=CARTESIAN_POINT('Ctrl Pts',(33.7152536393985,33.7193295360918,167.333557470637));
#32219=CARTESIAN_POINT('Ctrl Pts',(34.3748036771893,31.4915603207829,167.222427681417));
#32220=CARTESIAN_POINT('Ctrl Pts',(32.8609514252531,29.7291065603519,167.111297892197));
#32221=CARTESIAN_POINT('Ctrl Pts',(30.5591814806014,30.044956009926,167.000168102977));
#32222=CARTESIAN_POINT('Ctrl Pts',(29.5760010217537,32.1500279732525,166.889038313758));
#32223=CARTESIAN_POINT('Ctrl Pts',(30.8113032934655,34.1178215046619,166.777908524538));
#32224=CARTESIAN_POINT('Ctrl Pts',(33.1343552393677,34.1473557540512,166.666778735318));
#32225=CARTESIAN_POINT('Ctrl Pts',(34.4195276894793,32.2117592010123,166.555648946099));
#32226=CARTESIAN_POINT('Ctrl Pts',(33.4898246183641,30.0821472766194,166.444519156879));
#32227=CARTESIAN_POINT('Ctrl Pts',(31.1977703849704,29.7081726882415,166.333389367659));
#32228=CARTESIAN_POINT('Ctrl Pts',(29.6376219972954,31.4307513580499,166.222259578439));
#32229=CARTESIAN_POINT('Ctrl Pts',(30.2442045937981,33.6761645043479,166.11112978922));
#32230=CARTESIAN_POINT('Ctrl Pts',(31.7124802469762,34.1461819386551,166.037043263073));
#32231=CARTESIAN_POINT('Ctrl Pts',(32.3836679988478,34.0186125009917,166.));
#32232=CARTESIAN_POINT('Ctrl Pts',(33.2690708798531,33.0793586530476,179.));
#32233=CARTESIAN_POINT('Ctrl Pts',(33.3143937781624,33.0370771991883,179.));
#32234=CARTESIAN_POINT('Ctrl Pts',(33.3569863179444,32.9922261551744,179.));
#32235=CARTESIAN_POINT('Ctrl Pts',(33.3968502279411,32.9451506656108,179.));
#32236=CARTESIAN_POINT('Ctrl Pts',(33.4393503990047,32.8949620022427,179.));
#32237=CARTESIAN_POINT('Ctrl Pts',(33.4787498348177,32.8422447205077,179.));
#32238=CARTESIAN_POINT('Ctrl Pts',(33.515021779277,32.787362334173,179.));
#32239=CARTESIAN_POINT('Ctrl Pts',(33.5467597306789,32.7393402461302,179.));
#32240=CARTESIAN_POINT('Ctrl Pts',(33.5761029525123,32.6896592737051,179.));
#32241=CARTESIAN_POINT('Ctrl Pts',(33.6030106200597,32.6385353790539,179.));
#32242=CARTESIAN_POINT('Ctrl Pts',(33.6165047704786,32.6128968311118,179.));
#32243=CARTESIAN_POINT('Ctrl Pts',(33.6293860170028,32.586895031717,179.));
#32244=CARTESIAN_POINT('Ctrl Pts',(33.641646871455,32.5605553798914,179.));
#32245=CARTESIAN_POINT('Ctrl Pts',(33.6472617019107,32.5484931961473,179.));
#32246=CARTESIAN_POINT('Ctrl Pts',(33.6527470163596,32.5363584469774,179.));
#32247=CARTESIAN_POINT('Ctrl Pts',(33.6580935559345,32.5241735966087,179.));
#32248=CARTESIAN_POINT('Ctrl Pts',(33.6850051176496,32.4628417111726,179.));
#32249=CARTESIAN_POINT('Ctrl Pts',(33.708455881982,32.4001342696333,179.));
#32250=CARTESIAN_POINT('Ctrl Pts',(33.7284226243158,32.3364092263026,179.));
#32251=CARTESIAN_POINT('Ctrl Pts',(33.7487446483798,32.2715502802415,179.));
#32252=CARTESIAN_POINT('Ctrl Pts',(33.7654581172737,32.2056363549699,179.));
#32253=CARTESIAN_POINT('Ctrl Pts',(33.778499226047,32.1390083355841,179.));
#32254=CARTESIAN_POINT('Ctrl Pts',(33.789406899287,32.0832802010578,179.));
#32255=CARTESIAN_POINT('Ctrl Pts',(33.7977449205042,32.0270515616279,179.));
#32256=CARTESIAN_POINT('Ctrl Pts',(33.8034511333226,31.9705095923301,179.));
#32257=CARTESIAN_POINT('Ctrl Pts',(33.8060782739115,31.9444776676104,179.));
#32258=CARTESIAN_POINT('Ctrl Pts',(33.8081472199985,31.9183792139312,179.));
#32259=CARTESIAN_POINT('Ctrl Pts',(33.809650107142,31.8922320972929,179.));
#32260=CARTESIAN_POINT('Ctrl Pts',(33.8103080275562,31.8807856477814,179.));
#32261=CARTESIAN_POINT('Ctrl Pts',(33.8108573512992,31.8693300330975,179.));
#32262=CARTESIAN_POINT('Ctrl Pts',(33.8112970804587,31.857880967774,179.));
#32263=CARTESIAN_POINT('Ctrl Pts',(33.8139906687424,31.7877490068823,179.));
#32264=CARTESIAN_POINT('Ctrl Pts',(33.8125841486909,31.7177313799782,179.));
#32265=CARTESIAN_POINT('Ctrl Pts',(33.8070231799885,31.6481892005974,179.));
#32266=CARTESIAN_POINT('Ctrl Pts',(33.8020529941113,31.5860350011532,179.));
#32267=CARTESIAN_POINT('Ctrl Pts',(33.7937638352136,31.5242596307283,179.));
#32268=CARTESIAN_POINT('Ctrl Pts',(33.7820838097155,31.4631087786356,179.));
#32269=CARTESIAN_POINT('Ctrl Pts',(33.769354070438,31.3964621429871,179.));
#32270=CARTESIAN_POINT('Ctrl Pts',(33.7525976732535,31.3305564900439,179.));
#32271=CARTESIAN_POINT('Ctrl Pts',(33.7320596705581,31.265605227867,179.));
#32272=CARTESIAN_POINT('Ctrl Pts',(33.7241289063575,31.2405242522486,179.));
#32273=CARTESIAN_POINT('Ctrl Pts',(33.7156337035593,31.2155856354338,179.));
#32274=CARTESIAN_POINT('Ctrl Pts',(33.706586160513,31.1908019867147,179.));
#32275=CARTESIAN_POINT('Ctrl Pts',(33.702618487712,31.1799334660092,179.));
#32276=CARTESIAN_POINT('Ctrl Pts',(33.6985446903967,31.1690953061603,179.));
#32277=CARTESIAN_POINT('Ctrl Pts',(33.6943708791898,31.1583011218621,179.));
#32278=CARTESIAN_POINT('Ctrl Pts',(33.6691493675868,31.0930740114287,179.));
#32279=CARTESIAN_POINT('Ctrl Pts',(33.6402374396347,31.0293334091269,179.));
#32280=CARTESIAN_POINT('Ctrl Pts',(33.607947561365,30.9672979393099,179.));
#32281=CARTESIAN_POINT('Ctrl Pts',(33.5749108621329,30.9038276734593,179.));
#32282=CARTESIAN_POINT('Ctrl Pts',(33.5383378486612,30.8421415079131,179.));
#32283=CARTESIAN_POINT('Ctrl Pts',(33.498507043831,30.7824773207679,179.));
#32284=CARTESIAN_POINT('Ctrl Pts',(33.4680142575527,30.736800932484,179.));
#32285=CARTESIAN_POINT('Ctrl Pts',(33.4356109333393,30.6923095509569,179.));
#32286=CARTESIAN_POINT('Ctrl Pts',(33.4014024846335,30.6491160175195,179.));
#32287=CARTESIAN_POINT('Ctrl Pts',(33.3801001770704,30.6222185121127,179.));
#32288=CARTESIAN_POINT('Ctrl Pts',(33.358097552623,30.5958244105247,179.));
#32289=CARTESIAN_POINT('Ctrl Pts',(33.3354171550448,30.5699626540177,179.));
#32290=CARTESIAN_POINT('Ctrl Pts',(33.3227587779473,30.5555286977725,179.));
#32291=CARTESIAN_POINT('Ctrl Pts',(33.3098848307075,30.5412560553495,179.));
#32292=CARTESIAN_POINT('Ctrl Pts',(33.2968228468101,30.5271750883558,179.));
#32293=CARTESIAN_POINT('Ctrl Pts',(33.2459583837086,30.4723426194361,179.));
#32294=CARTESIAN_POINT('Ctrl Pts',(33.1921974074919,30.4203552297909,179.));
#32295=CARTESIAN_POINT('Ctrl Pts',(33.1358245952464,30.3714766007923,179.));
#32296=CARTESIAN_POINT('Ctrl Pts',(33.0936773153233,30.3349323664957,179.));
#32297=CARTESIAN_POINT('Ctrl Pts',(33.0500689035381,30.3001260799766,179.));
#32298=CARTESIAN_POINT('Ctrl Pts',(33.0051019564734,30.2671776805756,179.));
#32299=CARTESIAN_POINT('Ctrl Pts',(32.9910181102745,30.2568580965266,179.));
#32300=CARTESIAN_POINT('Ctrl Pts',(32.9768009030306,30.2467208427216,179.));
#32301=CARTESIAN_POINT('Ctrl Pts',(32.9624532443534,30.2367698321705,179.));
#32302=CARTESIAN_POINT('Ctrl Pts',(32.9486742469643,30.2272132242606,179.));
#32303=CARTESIAN_POINT('Ctrl Pts',(32.9347819948037,30.2178333484506,179.));
#32304=CARTESIAN_POINT('Ctrl Pts',(32.9207843887783,30.2086363784296,179.));
#32305=CARTESIAN_POINT('Ctrl Pts',(32.857836207379,30.1672769819617,179.));
#32306=CARTESIAN_POINT('Ctrl Pts',(32.79273001494,30.1295928505755,179.));
#32307=CARTESIAN_POINT('Ctrl Pts',(32.725726822945,30.0958629167136,179.));
#32308=CARTESIAN_POINT('Ctrl Pts',(32.6745421351153,30.0700961422685,179.));
#32309=CARTESIAN_POINT('Ctrl Pts',(32.6222494513403,30.0466373077193,179.));
#32310=CARTESIAN_POINT('Ctrl Pts',(32.5689512962096,30.0256259714062,179.));
#32311=CARTESIAN_POINT('Ctrl Pts',(32.5564668873308,30.0207043355076,179.));
#32312=CARTESIAN_POINT('Ctrl Pts',(32.5439272667614,30.0159170540829,179.));
#32313=CARTESIAN_POINT('Ctrl Pts',(32.5313343916942,30.0112635340338,179.));
#32314=CARTESIAN_POINT('Ctrl Pts',(30.3326674383851,31.998696643609,177.87148036339));
#32315=CARTESIAN_POINT('Ctrl Pts',(30.3319312160462,31.9130454971719,177.877220944861));
#32316=CARTESIAN_POINT('Ctrl Pts',(30.3379613622294,31.8274983352525,177.882961526332));
#32317=CARTESIAN_POINT('Ctrl Pts',(30.3511186960486,31.7430618380899,177.888702107803));
#32318=CARTESIAN_POINT('Ctrl Pts',(30.4360213458042,31.1982035526917,177.925745370876));
#32319=CARTESIAN_POINT('Ctrl Pts',(30.8176973425019,30.6995929198072,177.962788633949));
#32320=CARTESIAN_POINT('Ctrl Pts',(31.3214948089321,30.4753846070209,177.999831897022));
#32321=CARTESIAN_POINT('Ctrl Pts',(31.8252922753623,30.2511762942346,178.036875160096));
#32322=CARTESIAN_POINT('Ctrl Pts',(32.451211211525,30.3013703015467,178.073918423169));
#32323=CARTESIAN_POINT('Ctrl Pts',(32.9128324917223,30.6030120799742,178.110961686242));
#32324=CARTESIAN_POINT('Ctrl Pts',(33.3744537719195,30.9046538584017,178.148004949315));
#32325=CARTESIAN_POINT('Ctrl Pts',(33.6717773961514,31.4577434079447,178.185048212389));
#32326=CARTESIAN_POINT('Ctrl Pts',(33.6687537877731,32.0091615320545,178.222091475462));
#32327=CARTESIAN_POINT('Ctrl Pts',(33.6657301793948,32.5605796561643,178.259134738535));
#32328=CARTESIAN_POINT('Ctrl Pts',(33.3623593384064,33.1103263548409,178.296178001608));
#32329=CARTESIAN_POINT('Ctrl Pts',(32.8974537652324,33.4068983824074,178.333221264682));
#32330=CARTESIAN_POINT('Ctrl Pts',(32.4325481920584,33.703470409974,178.370264527755));
#32331=CARTESIAN_POINT('Ctrl Pts',(31.8061078866989,33.7468677664304,178.407307790828));
#32332=CARTESIAN_POINT('Ctrl Pts',(31.3048055390909,33.5171142355207,178.444351053901));
#32333=CARTESIAN_POINT('Ctrl Pts',(30.8035031914829,33.287360704611,178.481394316975));
#32334=CARTESIAN_POINT('Ctrl Pts',(30.4273388016264,32.7844562863351,178.518437580048));
#32335=CARTESIAN_POINT('Ctrl Pts',(30.348408546375,32.2387672663122,178.555480843121));
#32336=CARTESIAN_POINT('Ctrl Pts',(30.337044840679,32.1602036102679,178.560814016544));
#32337=CARTESIAN_POINT('Ctrl Pts',(30.3318421408634,32.0807531241047,178.566147189967));
#32338=CARTESIAN_POINT('Ctrl Pts',(30.3325025488117,32.0012179414303,178.57148036339));
#32339=CARTESIAN_POINT('Ctrl Pts',(31.4698297828098,30.0148256743287,179.));
#32340=CARTESIAN_POINT('Ctrl Pts',(30.8097602092458,30.191107033931,178.962956736927));
#32341=CARTESIAN_POINT('Ctrl Pts',(29.6908221960836,31.2516371458941,178.88887021078));
#32342=CARTESIAN_POINT('Ctrl Pts',(30.1185589391069,33.5378733053769,178.777740421561));
#32343=CARTESIAN_POINT('Ctrl Pts',(32.2716026719728,34.4129388487757,178.666610632341));
#32344=CARTESIAN_POINT('Ctrl Pts',(34.1744105218922,33.0815150675564,178.555480843121));
#32345=CARTESIAN_POINT('Ctrl Pts',(34.0880401159474,30.7594177996359,178.444351053901));
#32346=CARTESIAN_POINT('Ctrl Pts',(32.0903159869838,29.5731212764253,178.333221264682));
#32347=CARTESIAN_POINT('Ctrl Pts',(30.0101331232206,30.6076649966109,178.222091475462));
#32348=CARTESIAN_POINT('Ctrl Pts',(29.7509578494046,32.9165631575214,178.110961686242));
#32349=CARTESIAN_POINT('Ctrl Pts',(31.5501292046485,34.3865813061288,177.999831897022));
#32350=CARTESIAN_POINT('Ctrl Pts',(33.7609940320372,33.6724513469602,177.888702107803));
#32351=CARTESIAN_POINT('Ctrl Pts',(34.3602277126424,31.4276996634035,177.777572318583));
#32352=CARTESIAN_POINT('Ctrl Pts',(32.7994009405473,29.7067171266042,177.666442529363));
#32353=CARTESIAN_POINT('Ctrl Pts',(30.5069738698555,30.0845192170702,177.555312740143));
#32354=CARTESIAN_POINT('Ctrl Pts',(29.580946760212,32.2153500156115,177.444182950924));
#32355=CARTESIAN_POINT('Ctrl Pts',(30.8688116111015,34.1490940941566,177.333053161704));
#32356=CARTESIAN_POINT('Ctrl Pts',(33.1919274796751,34.1160109178655,177.221923372484));
#32357=CARTESIAN_POINT('Ctrl Pts',(34.4242044061711,32.1463773227603,177.110793583265));
#32358=CARTESIAN_POINT('Ctrl Pts',(33.4378756702622,30.0427808747097,176.999663794045));
#32359=CARTESIAN_POINT('Ctrl Pts',(31.135618752982,29.7304101029964,176.888534004825));
#32360=CARTESIAN_POINT('Ctrl Pts',(29.6244341600216,31.4951434129585,176.777404215606));
#32361=CARTESIAN_POINT('Ctrl Pts',(30.2873416712654,33.7219159863135,176.666274426386));
#32362=CARTESIAN_POINT('Ctrl Pts',(32.5176555073463,34.3728097273692,176.555144637166));
#32363=CARTESIAN_POINT('Ctrl Pts',(34.2742166391108,32.8521337355438,176.444014847946));
#32364=CARTESIAN_POINT('Ctrl Pts',(33.9494393645001,30.5515941911541,176.332885058726));
#32365=CARTESIAN_POINT('Ctrl Pts',(31.8405563248355,29.5766199351239,176.221755269507));
#32366=CARTESIAN_POINT('Ctrl Pts',(29.8775944073181,30.8194968342953,176.110625480287));
#32367=CARTESIAN_POINT('Ctrl Pts',(29.857035071825,33.1427574285537,175.999495691067));
#32368=CARTESIAN_POINT('Ctrl Pts',(31.7976939990458,34.4201788169579,175.888365901848));
#32369=CARTESIAN_POINT('Ctrl Pts',(33.9235011844546,33.4826787977943,175.777236112628));
#32370=CARTESIAN_POINT('Ctrl Pts',(34.2889409453366,31.1882472218883,175.666106323408));
#32371=CARTESIAN_POINT('Ctrl Pts',(32.5595667755852,29.6367229854095,175.554976534189));
#32372=CARTESIAN_POINT('Ctrl Pts',(30.3180831610634,30.248044244016,175.443846744969));
#32373=CARTESIAN_POINT('Ctrl Pts',(29.6158715979096,32.462736411328,175.332716955749));
#32374=CARTESIAN_POINT('Ctrl Pts',(31.0955884935522,34.2539372331611,175.221587166529));
#32375=CARTESIAN_POINT('Ctrl Pts',(33.4030129919618,33.982359142136,175.11045737731));
#32376=CARTESIAN_POINT('Ctrl Pts',(34.4264152151701,31.8965474620181,174.99932758809));
#32377=CARTESIAN_POINT('Ctrl Pts',(33.2291885468321,29.905414422765,174.88819779887));
#32378=CARTESIAN_POINT('Ctrl Pts',(30.9070218504281,29.8312233889627,174.77706800965));
#32379=CARTESIAN_POINT('Ctrl Pts',(29.5851369036578,31.7418731901787,174.665938220431));
#32380=CARTESIAN_POINT('Ctrl Pts',(30.4733084745601,33.8887578484745,174.554808431211));
#32381=CARTESIAN_POINT('Ctrl Pts',(32.7586915732648,34.3070718065724,174.443678641991));
#32382=CARTESIAN_POINT('Ctrl Pts',(34.3497283717851,32.6139786664471,174.332548852772));
#32383=CARTESIAN_POINT('Ctrl Pts',(33.7903192461908,30.3589789091108,174.221419063552));
#32384=CARTESIAN_POINT('Ctrl Pts',(31.5924293616864,29.6058238580236,174.110289274332));
#32385=CARTESIAN_POINT('Ctrl Pts',(29.7675437054471,31.0437928483141,173.999159485112));
#32386=CARTESIAN_POINT('Ctrl Pts',(29.9857778400022,33.3568722541927,173.888029695893));
#32387=CARTESIAN_POINT('Ctrl Pts',(32.0474062520575,34.428156887701,173.776899906673));
#32388=CARTESIAN_POINT('Ctrl Pts',(34.0656489763292,33.2772186698503,173.665770117453));
#32389=CARTESIAN_POINT('Ctrl Pts',(34.1934321584947,30.9573837762123,173.554640328233));
#32390=CARTESIAN_POINT('Ctrl Pts',(32.3138100159872,29.5917399438827,173.443510539014));
#32391=CARTESIAN_POINT('Ctrl Pts',(30.146992349976,30.4301095984188,173.332380749794));
#32392=CARTESIAN_POINT('Ctrl Pts',(29.6760271902357,32.7052259237296,173.221250960574));
#32393=CARTESIAN_POINT('Ctrl Pts',(31.3319367435559,34.3349271314997,173.110121171355));
#32394=CARTESIAN_POINT('Ctrl Pts',(33.5992505443295,33.8277283497517,172.998991382135));
#32395=CARTESIAN_POINT('Ctrl Pts',(34.4029475900826,31.6478124031995,172.887861592915));
#32396=CARTESIAN_POINT('Ctrl Pts',(33.0074930602737,29.7902147259237,172.776731803695));
#32397=CARTESIAN_POINT('Ctrl Pts',(30.6899918075095,29.9549885673591,172.665602014476));
#32398=CARTESIAN_POINT('Ctrl Pts',(29.5713958460653,31.9913346947219,172.554472225256));
#32399=CARTESIAN_POINT('Ctrl Pts',(30.6754320691868,34.035611215504,172.443342436036));
#32400=CARTESIAN_POINT('Ctrl Pts',(32.9916984982474,34.2169184271411,172.332212646816));
#32401=CARTESIAN_POINT('Ctrl Pts',(34.4003732162344,32.369325935738,172.221082857597));
#32402=CARTESIAN_POINT('Ctrl Pts',(33.6122523976872,30.1837303531204,172.109953068377));
#32403=CARTESIAN_POINT('Ctrl Pts',(31.3486156689259,29.6603650547029,171.998823279157));
#32404=CARTESIAN_POINT('Ctrl Pts',(29.6811188159947,31.2782082859368,171.887693489937));
#32405=CARTESIAN_POINT('Ctrl Pts',(30.1358368754459,33.5566274663761,171.776563700718));
#32406=CARTESIAN_POINT('Ctrl Pts',(32.2966168104817,34.41043807051,171.665433911498));
#32407=CARTESIAN_POINT('Ctrl Pts',(34.1859362572401,33.0582418926255,171.554304122278));
#32408=CARTESIAN_POINT('Ctrl Pts',(34.0747105468639,30.7375542107656,171.443174333058));
#32409=CARTESIAN_POINT('Ctrl Pts',(32.064732243297,29.5722432245585,171.332044543839));
#32410=CARTESIAN_POINT('Ctrl Pts',(29.9955116926565,30.6287889113096,171.220914754619));
#32411=CARTESIAN_POINT('Ctrl Pts',(29.7607771031263,32.9402521162651,171.1097849654));
#32412=CARTESIAN_POINT('Ctrl Pts',(31.5753550254538,34.3912067810244,170.99865517618));
#32413=CARTESIAN_POINT('Ctrl Pts',(33.7785634234029,33.6537549313479,170.88752538696));
#32414=CARTESIAN_POINT('Ctrl Pts',(34.3540498639709,31.4028045027273,170.77639559774));
#32415=CARTESIAN_POINT('Ctrl Pts',(32.7751353976405,29.6984009168952,170.66526580852));
#32416=CARTESIAN_POINT('Ctrl Pts',(30.4868254213828,30.1003958521179,170.554136019301));
#32417=CARTESIAN_POINT('Ctrl Pts',(29.5833564097807,32.2408879031331,170.443006230081));
#32418=CARTESIAN_POINT('Ctrl Pts',(30.8915734045388,34.1609219575215,170.331876440861));
#32419=CARTESIAN_POINT('Ctrl Pts',(33.2142103990771,34.1033036706089,170.220746651642));
#32420=CARTESIAN_POINT('Ctrl Pts',(34.4256152039436,32.1207646737337,170.109616862422));
#32421=CARTESIAN_POINT('Ctrl Pts',(33.4171232788624,30.0277031570956,169.998487073202));
#32422=CARTESIAN_POINT('Ctrl Pts',(31.1116954970284,29.7396663224151,169.887357283982));
#32423=CARTESIAN_POINT('Ctrl Pts',(29.6192343630528,31.5202623571622,169.776227494763));
#32424=CARTESIAN_POINT('Ctrl Pts',(30.305624121683,33.7399090800963,169.665097705543));
#32425=CARTESIAN_POINT('Ctrl Pts',(32.5426883094078,34.3672098814547,169.553967916323));
#32426=CARTESIAN_POINT('Ctrl Pts',(34.2830900415719,32.8280658706275,169.442838127104));
#32427=CARTESIAN_POINT('Ctrl Pts',(33.9340325267706,30.5310849550035,169.331708337884));
#32428=CARTESIAN_POINT('Ctrl Pts',(31.8149694171768,29.5784391588377,169.220578548664));
#32429=CARTESIAN_POINT('Ctrl Pts',(29.8652442904127,30.8419795837744,169.109448759444));
#32430=CARTESIAN_POINT('Ctrl Pts',(29.869224438595,33.165327735423,168.998318970225));
#32431=CARTESIAN_POINT('Ctrl Pts',(31.8232672732892,34.4221805810845,168.887189181005));
#32432=CARTESIAN_POINT('Ctrl Pts',(33.9390539828564,33.4622800263533,168.776059391785));
#32433=CARTESIAN_POINT('Ctrl Pts',(34.2802395155314,31.1641166493491,168.664929602565));
#32434=CARTESIAN_POINT('Ctrl Pts',(32.5345745716517,29.6309446499222,168.553799813346));
#32435=CARTESIAN_POINT('Ctrl Pts',(30.2996727772365,30.2659064158787,168.442670024126));
#32436=CARTESIAN_POINT('Ctrl Pts',(29.620892017365,32.4878918238939,168.331540234906));
#32437=CARTESIAN_POINT('Ctrl Pts',(31.1194450837624,34.2633639270065,168.220410445687));
#32438=CARTESIAN_POINT('Ctrl Pts',(33.4238724584211,33.9674299065165,168.109280656467));
#32439=CARTESIAN_POINT('Ctrl Pts',(34.4251872041711,31.8709253771026,167.998150867247));
#32440=CARTESIAN_POINT('Ctrl Pts',(33.206996913019,29.8925485313441,167.887021078027));
#32441=CARTESIAN_POINT('Ctrl Pts',(30.8841761520946,29.8428884386802,167.775891288808));
#32442=CARTESIAN_POINT('Ctrl Pts',(29.5825452442318,31.7673934065167,167.664761499588));
#32443=CARTESIAN_POINT('Ctrl Pts',(30.493342777661,33.9047775029395,167.553631710368));
#32444=CARTESIAN_POINT('Ctrl Pts',(32.7830165295865,34.2989296881618,167.442501921148));
#32445=CARTESIAN_POINT('Ctrl Pts',(34.3560823145915,32.5891267546308,167.331372131929));
#32446=CARTESIAN_POINT('Ctrl Pts',(33.7728865672594,30.3401605876776,167.220242342709));
#32447=CARTESIAN_POINT('Ctrl Pts',(31.5671653767747,29.6102631127892,167.109112553489));
#32448=CARTESIAN_POINT('Ctrl Pts',(29.7575674653531,31.0674235375315,166.99798276427));
#32449=CARTESIAN_POINT('Ctrl Pts',(30.0002241215838,33.3780747167424,166.88685297505));
#32450=CARTESIAN_POINT('Ctrl Pts',(32.073044548561,34.4275128335807,166.77572318583));
#32451=CARTESIAN_POINT('Ctrl Pts',(34.0790345884103,33.255346086573,166.66459339661));
#32452=CARTESIAN_POINT('Ctrl Pts',(34.1822756467128,30.9342420768624,166.553463607391));
#32453=CARTESIAN_POINT('Ctrl Pts',(32.2884012470789,29.5886265247524,166.442333818171));
#32454=CARTESIAN_POINT('Ctrl Pts',(30.1304232002167,30.4496328462658,166.331204028951));
#32455=CARTESIAN_POINT('Ctrl Pts',(29.6837912905188,32.7300090226775,166.220074239731));
#32456=CARTESIAN_POINT('Ctrl Pts',(31.356257105939,34.3412895988536,166.108944450512));
#32457=CARTESIAN_POINT('Ctrl Pts',(33.619236151672,33.8118910160724,165.997814661292));
#32458=CARTESIAN_POINT('Ctrl Pts',(34.3974968060795,31.6200550614307,165.886684872072));
#32459=CARTESIAN_POINT('Ctrl Pts',(33.4572031808889,30.3983372977448,165.812598345926));
#32460=CARTESIAN_POINT('Ctrl Pts',(32.8326019491379,30.1214975228146,165.775555082853));
#32461=CARTESIAN_POINT('Ctrl Pts',(31.5032651029109,30.1400211999976,179.074814972382));
#32462=CARTESIAN_POINT('Ctrl Pts',(30.8848229855212,30.3051853306515,179.037771709309));
#32463=CARTESIAN_POINT('Ctrl Pts',(29.8364510838271,31.2988328403474,178.963685183163));
#32464=CARTESIAN_POINT('Ctrl Pts',(30.2372124999491,33.44088693275,178.852555393943));
#32465=CARTESIAN_POINT('Ctrl Pts',(32.254473980124,34.2607662442478,178.741425604723));
#32466=CARTESIAN_POINT('Ctrl Pts',(34.0372807671961,33.0133090437071,178.630295815504));
#32467=CARTESIAN_POINT('Ctrl Pts',(33.9563573329528,30.8376554328259,178.519166026284));
#32468=CARTESIAN_POINT('Ctrl Pts',(32.0846201862067,29.7261730027164,178.408036237064));
#32469=CARTESIAN_POINT('Ctrl Pts',(30.1356245858232,30.6954729590666,178.296906447844));
#32470=CARTESIAN_POINT('Ctrl Pts',(29.8927942668186,32.8587598679912,178.185776658625));
#32471=CARTESIAN_POINT('Ctrl Pts',(31.5785004212106,34.236070946757,178.074646869405));
#32472=CARTESIAN_POINT('Ctrl Pts',(33.6499364938202,33.5669777757827,177.963517080185));
#32473=CARTESIAN_POINT('Ctrl Pts',(34.2113793493719,31.4637919302408,177.852387290966));
#32474=CARTESIAN_POINT('Ctrl Pts',(32.7489865161425,29.8513435964963,177.741257501746));
#32475=CARTESIAN_POINT('Ctrl Pts',(30.6011319439267,30.2053195016732,177.630127712526));
#32476=CARTESIAN_POINT('Ctrl Pts',(29.7335049703702,32.2017689118975,177.518997923306));
#32477=CARTESIAN_POINT('Ctrl Pts',(30.9401502956429,34.0135609264389,177.407868134087));
#32478=CARTESIAN_POINT('Ctrl Pts',(33.116758268867,33.9825641491069,177.296738344867));
#32479=CARTESIAN_POINT('Ctrl Pts',(34.2713213363899,32.1371459995299,177.185608555647));
#32480=CARTESIAN_POINT('Ctrl Pts',(33.3471956740235,30.1662133985295,177.074478766427));
#32481=CARTESIAN_POINT('Ctrl Pts',(31.1901311770041,29.8735423692835,176.963348977208));
#32482=CARTESIAN_POINT('Ctrl Pts',(29.7742498262084,31.5269823225115,176.852219187988));
#32483=CARTESIAN_POINT('Ctrl Pts',(30.3953509060134,33.6133229150267,176.741089398768));
#32484=CARTESIAN_POINT('Ctrl Pts',(32.4850094306167,34.2231678761279,176.629959609548));
#32485=CARTESIAN_POINT('Ctrl Pts',(34.1307925861515,32.7983937039596,176.518829820329));
#32486=CARTESIAN_POINT('Ctrl Pts',(33.8264974732807,30.6429382732709,176.407700031109));
#32487=CARTESIAN_POINT('Ctrl Pts',(31.8506116809161,29.7294510176109,176.29657024189));
#32488=CARTESIAN_POINT('Ctrl Pts',(30.0114444578766,30.8939455678262,176.185440452669));
#32489=CARTESIAN_POINT('Ctrl Pts',(29.9921817021251,33.0706891395728,176.07431066345));
#32490=CARTESIAN_POINT('Ctrl Pts',(31.8104524786453,34.2675496219881,175.96318087423));
#32491=CARTESIAN_POINT('Ctrl Pts',(33.8021950911818,33.3891732808794,175.85205108501));
#32492=CARTESIAN_POINT('Ctrl Pts',(34.1445883002461,31.2394406180825,175.740921295791));
#32493=CARTESIAN_POINT('Ctrl Pts',(32.5242775540239,29.7857636536858,175.629791506571));
#32494=CARTESIAN_POINT('Ctrl Pts',(30.4241536759089,30.3585317810463,175.518661717351));
#32495=CARTESIAN_POINT('Ctrl Pts',(29.766227264262,32.4335538214098,175.407531928132));
#32496=CARTESIAN_POINT('Ctrl Pts',(31.1526254361051,34.1117921061154,175.296402138912));
#32497=CARTESIAN_POINT('Ctrl Pts',(33.3145316194307,33.8573411567355,175.185272349692));
#32498=CARTESIAN_POINT('Ctrl Pts',(34.2733927201549,31.9030717227376,175.074142560472));
#32499=CARTESIAN_POINT('Ctrl Pts',(33.1516694573109,30.0375099969467,174.963012771253));
#32500=CARTESIAN_POINT('Ctrl Pts',(30.9759507964711,29.9679978396324,174.851882982033));
#32501=CARTESIAN_POINT('Ctrl Pts',(29.7374308613498,31.7581520233406,174.740753192813));
#32502=CARTESIAN_POINT('Ctrl Pts',(30.5695896653805,33.7696428525554,174.629623403593));
#32503=CARTESIAN_POINT('Ctrl Pts',(32.7108444955008,34.1615757340891,174.518493614374));
#32504=CARTESIAN_POINT('Ctrl Pts',(34.2015421521264,32.5752579450972,174.407363825154));
#32505=CARTESIAN_POINT('Ctrl Pts',(33.6774123058563,30.462470323165,174.296234035934));
#32506=CARTESIAN_POINT('Ctrl Pts',(31.6181329080456,29.7568131876572,174.185104246715));
#32507=CARTESIAN_POINT('Ctrl Pts',(29.9083341316153,31.1040962964574,174.073974457495));
#32508=CARTESIAN_POINT('Ctrl Pts',(30.1128052747589,33.2713007590689,173.962844668275));
#32509=CARTESIAN_POINT('Ctrl Pts',(32.0444165646686,34.275024553663,173.851714879055));
#32510=CARTESIAN_POINT('Ctrl Pts',(33.9353782962711,33.1966705483588,173.740585089836));
#32511=CARTESIAN_POINT('Ctrl Pts',(34.05510279943,31.0231366345483,173.629455300616));
#32512=CARTESIAN_POINT('Ctrl Pts',(32.2940195072124,29.7436174791571,173.518325511396));
#32513=CARTESIAN_POINT('Ctrl Pts',(30.2638527505027,30.5291151373919,173.407195722177));
#32514=CARTESIAN_POINT('Ctrl Pts',(29.8225891288001,32.6607506708034,173.296065932957));
#32515=CARTESIAN_POINT('Ctrl Pts',(31.374068323382,34.1876743558384,173.184936143737));
#32516=CARTESIAN_POINT('Ctrl Pts',(33.4983934004583,33.7124621947505,173.073806354517));
#32517=CARTESIAN_POINT('Ctrl Pts',(34.2514050868349,31.6700232039062,172.962676565298));
#32518=CARTESIAN_POINT('Ctrl Pts',(32.9439552532118,29.9295753983976,172.851546776078));
#32519=CARTESIAN_POINT('Ctrl Pts',(30.7726078086176,30.0839577354556,172.740416986858));
#32520=CARTESIAN_POINT('Ctrl Pts',(29.7245563870626,31.9918811744116,172.629287197638));
#32521=CARTESIAN_POINT('Ctrl Pts',(30.7589662839094,33.9072348745011,172.518157408419));
#32522=CARTESIAN_POINT('Ctrl Pts',(32.9291567792721,34.0771079005481,172.407027619199));
#32523=CARTESIAN_POINT('Ctrl Pts',(34.2489930665307,32.3460343013108,172.295897829979));
#32524=CARTESIAN_POINT('Ctrl Pts',(33.5105752886146,30.2982738620995,172.184768040759));
#32525=CARTESIAN_POINT('Ctrl Pts',(31.3896953880653,29.8079147298433,172.07363825154));
#32526=CARTESIAN_POINT('Ctrl Pts',(29.8273596498807,31.3237282646596,171.96250846232));
#32527=CARTESIAN_POINT('Ctrl Pts',(30.2534007988218,33.4584583577978,171.8513786731));
#32528=CARTESIAN_POINT('Ctrl Pts',(32.2779105956015,34.2584231782018,171.74024888388));
#32529=CARTESIAN_POINT('Ctrl Pts',(34.0480796291017,32.991503597495,171.629119094661));
#32530=CARTESIAN_POINT('Ctrl Pts',(33.9438683965466,30.8171706767696,171.517989305441));
#32531=CARTESIAN_POINT('Ctrl Pts',(32.0606498878471,29.7253503254147,171.406859516221));
#32532=CARTESIAN_POINT('Ctrl Pts',(30.1219252595105,30.7152646886918,171.295729727001));
#32533=CARTESIAN_POINT('Ctrl Pts',(29.9019942667975,32.8809548765038,171.184599937782));
#32534=CARTESIAN_POINT('Ctrl Pts',(31.6021353691866,34.2404047148974,171.073470148562));
#32535=CARTESIAN_POINT('Ctrl Pts',(33.6663978670339,33.5494604543942,170.962340359343));
#32536=CARTESIAN_POINT('Ctrl Pts',(34.2055911083041,31.4404667892284,170.851210570123));
#32537=CARTESIAN_POINT('Ctrl Pts',(32.7262512858941,29.8435518506758,170.740080780903));
#32538=CARTESIAN_POINT('Ctrl Pts',(30.5822541625009,30.2201948726783,170.628950991683));
#32539=CARTESIAN_POINT('Ctrl Pts',(29.7357626547736,32.2256962460227,170.517821202463));
#32540=CARTESIAN_POINT('Ctrl Pts',(30.9614766107659,34.0246428625811,170.406691413244));
#32541=CARTESIAN_POINT('Ctrl Pts',(33.1376359102681,33.9706582876428,170.295561624024));
#32542=CARTESIAN_POINT('Ctrl Pts',(34.2726431618406,32.1131486187531,170.184431834804));
#32543=CARTESIAN_POINT('Ctrl Pts',(33.3277520374855,30.1520865610262,170.073302045585));
#32544=CARTESIAN_POINT('Ctrl Pts',(31.1677166472949,29.8822148428614,169.962172256365));
#32545=CARTESIAN_POINT('Ctrl Pts',(29.7693779557629,31.5505171340862,169.851042467145));
#32546=CARTESIAN_POINT('Ctrl Pts',(30.4124803690279,33.6301812697564,169.739912677925));
#32547=CARTESIAN_POINT('Ctrl Pts',(32.5084635326252,34.2179211859256,169.628782888706));
#32548=CARTESIAN_POINT('Ctrl Pts',(34.139106385221,32.7758436850889,169.517653099486));
#32549=CARTESIAN_POINT('Ctrl Pts',(33.812062271706,30.6237224573342,169.406523310266));
#32550=CARTESIAN_POINT('Ctrl Pts',(31.8266384181214,29.7311555115167,169.295393521046));
#32551=CARTESIAN_POINT('Ctrl Pts',(29.9998732042468,30.9150104369695,169.184263731827));
#32552=CARTESIAN_POINT('Ctrl Pts',(30.0036023433679,33.0918360442771,169.073133942607));
#32553=CARTESIAN_POINT('Ctrl Pts',(31.8344129678195,34.2694251443491,168.962004153387));
#32554=CARTESIAN_POINT('Ctrl Pts',(33.8167670483817,33.3700609631672,168.850874364168));
#32555=CARTESIAN_POINT('Ctrl Pts',(34.136435628333,31.2168318462613,168.739744574948));
#32556=CARTESIAN_POINT('Ctrl Pts',(32.5008614898121,29.7803497304012,168.628614785728));
#32557=CARTESIAN_POINT('Ctrl Pts',(30.4069043476383,30.3752674704802,168.517484996508));
#32558=CARTESIAN_POINT('Ctrl Pts',(29.7709310696827,32.4571228014599,168.406355207289));
#32559=CARTESIAN_POINT('Ctrl Pts',(31.174977504363,34.1206243031067,168.295225418069));
#32560=CARTESIAN_POINT('Ctrl Pts',(33.3340755783122,33.8433534371718,168.184095628849));
#32561=CARTESIAN_POINT('Ctrl Pts',(34.2722421539831,31.8790655011488,168.072965839629));
#32562=CARTESIAN_POINT('Ctrl Pts',(33.1308773445499,30.0254554962531,167.96183605041));
#32563=CARTESIAN_POINT('Ctrl Pts',(30.9545458679356,29.9789272300114,167.85070626119));
#32564=CARTESIAN_POINT('Ctrl Pts',(29.7350026455872,31.7820628007198,167.73957647197));
#32565=CARTESIAN_POINT('Ctrl Pts',(30.5883605000415,33.7846522234216,167.628446682751));
#32566=CARTESIAN_POINT('Ctrl Pts',(32.7336353922418,34.1539471004548,167.517316893531));
#32567=CARTESIAN_POINT('Ctrl Pts',(34.2074953819074,32.5519733254443,167.406187104311));
#32568=CARTESIAN_POINT('Ctrl Pts',(33.6610790232724,30.4448387839772,167.295057315091));
#32569=CARTESIAN_POINT('Ctrl Pts',(31.5944622027923,29.7609724796875,167.183927525872));
#32570=CARTESIAN_POINT('Ctrl Pts',(29.8989870456498,31.1262367102264,167.072797736652));
#32571=CARTESIAN_POINT('Ctrl Pts',(30.1263404979045,33.2911660829048,166.961667947432));
#32572=CARTESIAN_POINT('Ctrl Pts',(32.0684379754575,34.2744211169802,166.850538158213));
#32573=CARTESIAN_POINT('Ctrl Pts',(33.9479197413089,33.17617736513,166.739408368993));
#32574=CARTESIAN_POINT('Ctrl Pts',(34.0446498759119,31.0014543723761,166.628278579773));
#32575=CARTESIAN_POINT('Ctrl Pts',(32.2702131488022,29.7407004085991,166.517148790554));
#32576=CARTESIAN_POINT('Ctrl Pts',(30.2483285384032,30.5474071466291,166.406019001334));
#32577=CARTESIAN_POINT('Ctrl Pts',(29.8298635841167,32.6839708172891,166.294889212114));
#32578=CARTESIAN_POINT('Ctrl Pts',(31.3968549159023,34.1936355725642,166.183759422894));
#32579=CARTESIAN_POINT('Ctrl Pts',(33.5171186103713,33.697623646563,166.072629633675));
#32580=CARTESIAN_POINT('Ctrl Pts',(34.2462980579166,31.6440163859826,165.961499844455));
#32581=CARTESIAN_POINT('Ctrl Pts',(33.3653042902582,30.4993465649714,165.887413318308));
#32582=CARTESIAN_POINT('Ctrl Pts',(32.78009369465,30.2399657611251,165.850370055235));
#32583=CARTESIAN_POINT('Ctrl Pts',(31.5367004230119,30.2652167256666,179.149629944765));
#32584=CARTESIAN_POINT('Ctrl Pts',(30.9598857617967,30.419263627372,179.112586681692));
#32585=CARTESIAN_POINT('Ctrl Pts',(29.9820799715705,31.3460285348007,179.038500155545));
#32586=CARTESIAN_POINT('Ctrl Pts',(30.3558660607915,33.3439005601231,178.927370366326));
#32587=CARTESIAN_POINT('Ctrl Pts',(32.237345288275,34.1085936397198,178.816240577106));
#32588=CARTESIAN_POINT('Ctrl Pts',(33.9001510125,32.9451030198579,178.705110787886));
#32589=CARTESIAN_POINT('Ctrl Pts',(33.8246745499582,30.9158930660159,178.593980998666));
#32590=CARTESIAN_POINT('Ctrl Pts',(32.0789243854297,29.8792247290074,178.482851209447));
#32591=CARTESIAN_POINT('Ctrl Pts',(30.2611160484258,30.7832809215223,178.371721420227));
#32592=CARTESIAN_POINT('Ctrl Pts',(30.0346306842325,32.8009565784611,178.260591631007));
#32593=CARTESIAN_POINT('Ctrl Pts',(31.6068716377727,34.0855605873852,178.149461841787));
#32594=CARTESIAN_POINT('Ctrl Pts',(33.5388789556032,33.4615042046052,178.038332052568));
#32595=CARTESIAN_POINT('Ctrl Pts',(34.0625309861015,31.4998841970782,177.927202263348));
#32596=CARTESIAN_POINT('Ctrl Pts',(32.6985720917375,29.9959700663885,177.816072474128));
#32597=CARTESIAN_POINT('Ctrl Pts',(30.695290017998,30.3261197862762,177.704942684909));
#32598=CARTESIAN_POINT('Ctrl Pts',(29.8860631805284,32.1881878081835,177.593812895689));
#32599=CARTESIAN_POINT('Ctrl Pts',(31.0114889801843,33.8780277587213,177.482683106469));
#32600=CARTESIAN_POINT('Ctrl Pts',(33.041589058059,33.8491173803483,177.371553317249));
#32601=CARTESIAN_POINT('Ctrl Pts',(34.1184382666087,32.1279146762995,177.26042352803));
#32602=CARTESIAN_POINT('Ctrl Pts',(33.2565156777848,30.2896459223494,177.14929373881));
#32603=CARTESIAN_POINT('Ctrl Pts',(31.2446436010262,30.0166746355706,177.03816394959));
#32604=CARTESIAN_POINT('Ctrl Pts',(29.9240654923951,31.5588212320646,176.92703416037));
#32605=CARTESIAN_POINT('Ctrl Pts',(30.5033601407615,33.50472984374,176.815904371151));
#32606=CARTESIAN_POINT('Ctrl Pts',(32.452363353887,34.0735260248864,176.704774581931));
#32607=CARTESIAN_POINT('Ctrl Pts',(33.9873685331922,32.7446536723755,176.593644792711));
#32608=CARTESIAN_POINT('Ctrl Pts',(33.7035555820612,30.7342823553878,176.482515003492));
#32609=CARTESIAN_POINT('Ctrl Pts',(31.8606670369967,29.8822821000979,176.371385214272));
#32610=CARTESIAN_POINT('Ctrl Pts',(30.1452945084351,30.9683943013571,176.260255425052));
#32611=CARTESIAN_POINT('Ctrl Pts',(30.1273283324253,32.998620850592,176.149125635832));
#32612=CARTESIAN_POINT('Ctrl Pts',(31.8232109582448,34.1149204270184,176.037995846613));
#32613=CARTESIAN_POINT('Ctrl Pts',(33.680888997909,33.2956677639645,175.926866057393));
#32614=CARTESIAN_POINT('Ctrl Pts',(34.0002356551555,31.2906340142769,175.815736268173));
#32615=CARTESIAN_POINT('Ctrl Pts',(32.4889883324627,29.934804321962,175.704606478953));
#32616=CARTESIAN_POINT('Ctrl Pts',(30.5302241907544,30.4690193180765,175.593476689734));
#32617=CARTESIAN_POINT('Ctrl Pts',(29.9165829306144,32.4043712314915,175.482346900514));
#32618=CARTESIAN_POINT('Ctrl Pts',(31.2096623786579,33.9696469790697,175.371217111294));
#32619=CARTESIAN_POINT('Ctrl Pts',(33.2260502468995,33.7323231713349,175.260087322075));
#32620=CARTESIAN_POINT('Ctrl Pts',(34.1203702251398,31.9095959834572,175.148957532855));
#32621=CARTESIAN_POINT('Ctrl Pts',(33.0741503677897,30.1696055711286,175.037827743635));
#32622=CARTESIAN_POINT('Ctrl Pts',(31.0448797425142,30.1047722903021,174.926697954415));
#32623=CARTESIAN_POINT('Ctrl Pts',(29.8897248190418,31.7744308565025,174.815568165196));
#32624=CARTESIAN_POINT('Ctrl Pts',(30.6658708562009,33.6505278566363,174.704438375976));
#32625=CARTESIAN_POINT('Ctrl Pts',(32.6629974177368,34.0160796616058,174.593308586756));
#32626=CARTESIAN_POINT('Ctrl Pts',(34.0533559324676,32.5365372237472,174.482178797536));
#32627=CARTESIAN_POINT('Ctrl Pts',(33.5645053655219,30.5659617372191,174.371049008317));
#32628=CARTESIAN_POINT('Ctrl Pts',(31.6438364544047,29.9078025172906,174.259919219097));
#32629=CARTESIAN_POINT('Ctrl Pts',(30.0491245577835,31.1643997446009,174.148789429877));
#32630=CARTESIAN_POINT('Ctrl Pts',(30.2398327095156,33.1857292639449,174.037659640658));
#32631=CARTESIAN_POINT('Ctrl Pts',(32.0414268772797,34.1218922196251,173.926529851438));
#32632=CARTESIAN_POINT('Ctrl Pts',(33.805107616213,33.1161224268672,173.815400062218));
#32633=CARTESIAN_POINT('Ctrl Pts',(33.9167734403653,31.0888894928842,173.704270272998));
#32634=CARTESIAN_POINT('Ctrl Pts',(32.2742289984375,29.8954950144316,173.593140483778));
#32635=CARTESIAN_POINT('Ctrl Pts',(30.3807131510295,30.6281206763649,173.482010694559));
#32636=CARTESIAN_POINT('Ctrl Pts',(29.9691510673645,32.6162754178773,173.370880905339));
#32637=CARTESIAN_POINT('Ctrl Pts',(31.416199903208,34.040421580177,173.25975111612));
#32638=CARTESIAN_POINT('Ctrl Pts',(33.3975362565871,33.5971960397494,173.1486213269));
#32639=CARTESIAN_POINT('Ctrl Pts',(34.0998625835872,31.6922340046129,173.03749153768));
#32640=CARTESIAN_POINT('Ctrl Pts',(32.8804174461499,30.0689360708715,172.92636174846));
#32641=CARTESIAN_POINT('Ctrl Pts',(30.8552238097257,30.2129269035522,172.815231959241));
#32642=CARTESIAN_POINT('Ctrl Pts',(29.8777169280598,31.9924276541012,172.704102170021));
#32643=CARTESIAN_POINT('Ctrl Pts',(30.8425004986319,33.7788585334981,172.592972380801));
#32644=CARTESIAN_POINT('Ctrl Pts',(32.8666150602968,33.9372973739551,172.481842591581));
#32645=CARTESIAN_POINT('Ctrl Pts',(34.097612916827,32.3227426668835,172.370712802362));
#32646=CARTESIAN_POINT('Ctrl Pts',(33.408898179542,30.4128173710787,172.259583013142));
#32647=CARTESIAN_POINT('Ctrl Pts',(31.4307751072047,29.9554644049837,172.148453223922));
#32648=CARTESIAN_POINT('Ctrl Pts',(29.9736004837668,31.3692482433824,172.037323434702));
#32649=CARTESIAN_POINT('Ctrl Pts',(30.3709647221978,33.3602892492196,171.926193645483));
#32650=CARTESIAN_POINT('Ctrl Pts',(32.2592043807214,34.1064082858936,171.815063856263));
#32651=CARTESIAN_POINT('Ctrl Pts',(33.9102230009633,32.9247653023644,171.703934067043));
#32652=CARTESIAN_POINT('Ctrl Pts',(33.8130262462293,30.8967871427735,171.592804277824));
#32653=CARTESIAN_POINT('Ctrl Pts',(32.0565675323973,29.8784574262709,171.481674488604));
#32654=CARTESIAN_POINT('Ctrl Pts',(30.2483388263645,30.8017404660741,171.370544699384));
#32655=CARTESIAN_POINT('Ctrl Pts',(30.0432114304686,32.8216576367426,171.259414910164));
#32656=CARTESIAN_POINT('Ctrl Pts',(31.6289157129194,34.0896026487704,171.148285120945));
#32657=CARTESIAN_POINT('Ctrl Pts',(33.5542323106648,33.4451659774406,171.037155331725));
#32658=CARTESIAN_POINT('Ctrl Pts',(34.0571323526374,31.4781290757296,170.926025542505));
#32659=CARTESIAN_POINT('Ctrl Pts',(32.6773671741476,29.9887027844564,170.814895753285));
#32660=CARTESIAN_POINT('Ctrl Pts',(30.6776829036191,30.3399938932386,170.703765964066));
#32661=CARTESIAN_POINT('Ctrl Pts',(29.8881688997665,32.2105045889123,170.592636174846));
#32662=CARTESIAN_POINT('Ctrl Pts',(31.031379816993,33.8883637676406,170.481506385626));
#32663=CARTESIAN_POINT('Ctrl Pts',(33.061061421459,33.8380129046766,170.370376596406));
#32664=CARTESIAN_POINT('Ctrl Pts',(34.1196711197376,32.1055325637725,170.259246807187));
#32665=CARTESIAN_POINT('Ctrl Pts',(33.2383807961085,30.2764699649568,170.148117017967));
#32666=CARTESIAN_POINT('Ctrl Pts',(31.2237377975614,30.0247633633077,170.036987228747));
#32667=CARTESIAN_POINT('Ctrl Pts',(29.919521548473,31.5807719110101,169.925857439528));
#32668=CARTESIAN_POINT('Ctrl Pts',(30.5193366163728,33.5204534594166,169.814727650308));
#32669=CARTESIAN_POINT('Ctrl Pts',(32.4742387558426,34.0686324903965,169.703597861088));
#32670=CARTESIAN_POINT('Ctrl Pts',(33.9951227288701,32.7236214995502,169.592468071869));
#32671=CARTESIAN_POINT('Ctrl Pts',(33.6900920166414,30.716359959665,169.481338282649));
#32672=CARTESIAN_POINT('Ctrl Pts',(31.8383074190659,29.8838718641958,169.370208493429));
#32673=CARTESIAN_POINT('Ctrl Pts',(30.134502118081,30.9880412901646,169.259078704209));
#32674=CARTESIAN_POINT('Ctrl Pts',(30.1379802481407,33.0183443531313,169.14794891499));
#32675=CARTESIAN_POINT('Ctrl Pts',(31.8455586623499,34.1166697076136,169.03681912577));
#32676=CARTESIAN_POINT('Ctrl Pts',(33.6944801139071,33.2778418999811,168.92568933655));
#32677=CARTESIAN_POINT('Ctrl Pts',(33.9926317411346,31.2695470431734,168.81455954733));
#32678=CARTESIAN_POINT('Ctrl Pts',(32.4671484079726,29.9297548108802,168.703429758111));
#32679=CARTESIAN_POINT('Ctrl Pts',(30.5141359180401,30.4846285250817,168.592299968891));
#32680=CARTESIAN_POINT('Ctrl Pts',(29.9209701220004,32.4263537790259,168.481170179671));
#32681=CARTESIAN_POINT('Ctrl Pts',(31.2305099249636,33.977884679207,168.370040390452));
#32682=CARTESIAN_POINT('Ctrl Pts',(33.2442786982033,33.719276967827,168.258910601232));
#32683=CARTESIAN_POINT('Ctrl Pts',(34.1192971037951,31.8872056251949,168.147780812012));
#32684=CARTESIAN_POINT('Ctrl Pts',(33.0547577760807,30.158362461162,168.036651022792));
#32685=CARTESIAN_POINT('Ctrl Pts',(31.0249155837767,30.1149660213425,167.925521233573));
#32686=CARTESIAN_POINT('Ctrl Pts',(29.8874600469425,31.796732194923,167.814391444353));
#32687=CARTESIAN_POINT('Ctrl Pts',(30.6833782224221,33.6645269439038,167.703261655133));
#32688=CARTESIAN_POINT('Ctrl Pts',(32.6842542548971,34.0089645127478,167.592131865913));
#32689=CARTESIAN_POINT('Ctrl Pts',(34.0589084492235,32.5148198962578,167.481002076694));
#32690=CARTESIAN_POINT('Ctrl Pts',(33.5492714792853,30.5495169802769,167.369872287474));
#32691=CARTESIAN_POINT('Ctrl Pts',(31.6217590288099,29.9116818465859,167.258742498254));
#32692=CARTESIAN_POINT('Ctrl Pts',(30.0404066259465,31.1850498829213,167.147612709034));
#32693=CARTESIAN_POINT('Ctrl Pts',(30.2524568742251,33.2042574490671,167.036482919815));
#32694=CARTESIAN_POINT('Ctrl Pts',(32.063831402354,34.1213294003798,166.925353130595));
#32695=CARTESIAN_POINT('Ctrl Pts',(33.8168048942076,33.0970086436869,166.814223341375));
#32696=CARTESIAN_POINT('Ctrl Pts',(33.9070241051109,31.0686666678897,166.703093552156));
#32697=CARTESIAN_POINT('Ctrl Pts',(32.2520250505256,29.8927742924459,166.591963762936));
#32698=CARTESIAN_POINT('Ctrl Pts',(30.3662338765896,30.6451814469923,166.480833973716));
#32699=CARTESIAN_POINT('Ctrl Pts',(29.9759358777146,32.6379326119006,166.369704184496));
#32700=CARTESIAN_POINT('Ctrl Pts',(31.4374527258656,34.0459815462748,166.258574395277));
#32701=CARTESIAN_POINT('Ctrl Pts',(33.4150010690707,33.5833562770537,166.147444606057));
#32702=CARTESIAN_POINT('Ctrl Pts',(34.0950993097536,31.6679777105344,166.036314816837));
#32703=CARTESIAN_POINT('Ctrl Pts',(33.2734053996274,30.600355832198,165.962228290691));
#32704=CARTESIAN_POINT('Ctrl Pts',(32.727585440162,30.3584339994357,165.925185027618));
#32705=CARTESIAN_POINT('Ctrl Pts',(31.5701357431129,30.3904122513355,179.224444917147));
#32706=CARTESIAN_POINT('Ctrl Pts',(31.0349485380721,30.5333419240925,179.187401654074));
#32707=CARTESIAN_POINT('Ctrl Pts',(30.1277088593139,31.393224229254,179.113315127928));
#32708=CARTESIAN_POINT('Ctrl Pts',(30.4745196216338,33.2469141874962,179.002185338708));
#32709=CARTESIAN_POINT('Ctrl Pts',(32.2202165964262,33.9564210351918,178.891055549488));
#32710=CARTESIAN_POINT('Ctrl Pts',(33.7630212578038,32.8768969960087,178.779925760269));
#32711=CARTESIAN_POINT('Ctrl Pts',(33.6929917669636,30.9941306992059,178.668795971049));
#32712=CARTESIAN_POINT('Ctrl Pts',(32.0732285846526,30.0322764552985,178.557666181829));
#32713=CARTESIAN_POINT('Ctrl Pts',(30.3866075110284,30.871088883978,178.446536392609));
#32714=CARTESIAN_POINT('Ctrl Pts',(30.1764671016465,32.7431532889309,178.33540660339));
#32715=CARTESIAN_POINT('Ctrl Pts',(31.6352428543348,33.9350502280134,178.22427681417));
#32716=CARTESIAN_POINT('Ctrl Pts',(33.4278214173861,33.3560306334278,178.11314702495));
#32717=CARTESIAN_POINT('Ctrl Pts',(33.9136826228311,31.5359764639154,178.002017235731));
#32718=CARTESIAN_POINT('Ctrl Pts',(32.6481576673327,30.1405965362806,177.890887446511));
#32719=CARTESIAN_POINT('Ctrl Pts',(30.7894480920692,30.4469200708791,177.779757657291));
#32720=CARTESIAN_POINT('Ctrl Pts',(30.0386213906866,32.1746067044695,177.668627868071));
#32721=CARTESIAN_POINT('Ctrl Pts',(31.0828276647257,33.7424945910037,177.557498078852));
#32722=CARTESIAN_POINT('Ctrl Pts',(32.9664198472509,33.7156706115897,177.446368289632));
#32723=CARTESIAN_POINT('Ctrl Pts',(33.9655551968274,32.1186833530691,177.335238500412));
#32724=CARTESIAN_POINT('Ctrl Pts',(33.1658356815461,30.4130784461693,177.224108711192));
#32725=CARTESIAN_POINT('Ctrl Pts',(31.2991560250483,30.1598069018577,177.112978921973));
#32726=CARTESIAN_POINT('Ctrl Pts',(30.0738811585818,31.5906601416176,177.001849132753));
#32727=CARTESIAN_POINT('Ctrl Pts',(30.6113693755095,33.3961367724532,176.890719343533));
#32728=CARTESIAN_POINT('Ctrl Pts',(32.4197172771573,33.923884173645,176.779589554314));
#32729=CARTESIAN_POINT('Ctrl Pts',(33.8439444802329,32.6909136407913,176.668459765094));
#32730=CARTESIAN_POINT('Ctrl Pts',(33.5806136908418,30.8256264375046,176.557329975874));
#32731=CARTESIAN_POINT('Ctrl Pts',(31.8707223930774,30.035113182585,176.446200186654));
#32732=CARTESIAN_POINT('Ctrl Pts',(30.2791445589935,31.0428430348879,176.335070397435));
#32733=CARTESIAN_POINT('Ctrl Pts',(30.2624749627256,32.9265525616111,176.223940608215));
#32734=CARTESIAN_POINT('Ctrl Pts',(31.8359694378442,33.9622912320486,176.112810818995));
#32735=CARTESIAN_POINT('Ctrl Pts',(33.5595829046363,33.2021622470496,176.001681029775));
#32736=CARTESIAN_POINT('Ctrl Pts',(33.8558830100649,31.3418274104712,175.890551240556));
#32737=CARTESIAN_POINT('Ctrl Pts',(32.4536991109015,30.0838449902383,175.779421451336));
#32738=CARTESIAN_POINT('Ctrl Pts',(30.6362947056,30.5795068551068,175.668291662116));
#32739=CARTESIAN_POINT('Ctrl Pts',(30.0669385969668,32.3751886415732,175.557161872896));
#32740=CARTESIAN_POINT('Ctrl Pts',(31.2666993212108,33.827501852024,175.446032083677));
#32741=CARTESIAN_POINT('Ctrl Pts',(33.1375688743684,33.6073051859344,175.334902294457));
#32742=CARTESIAN_POINT('Ctrl Pts',(33.9673477301245,31.9161202441767,175.223772505237));
#32743=CARTESIAN_POINT('Ctrl Pts',(32.9966312782686,30.3017011453104,175.112642716018));
#32744=CARTESIAN_POINT('Ctrl Pts',(31.1138086885573,30.2415467409718,175.001512926798));
#32745=CARTESIAN_POINT('Ctrl Pts',(30.0420187767338,31.7907096896643,174.890383137578));
#32746=CARTESIAN_POINT('Ctrl Pts',(30.7621520470214,33.5314128607172,174.779253348358));
#32747=CARTESIAN_POINT('Ctrl Pts',(32.6151503399728,33.8705835891225,174.668123559139));
#32748=CARTESIAN_POINT('Ctrl Pts',(33.9051697128089,32.4978165023973,174.556993769919));
#32749=CARTESIAN_POINT('Ctrl Pts',(33.4515984251874,30.6694531512732,174.445863980699));
#32750=CARTESIAN_POINT('Ctrl Pts',(31.6695400007639,30.0587918469241,174.334734191479));
#32751=CARTESIAN_POINT('Ctrl Pts',(30.1899149839517,31.2247031927443,174.22360440226));
#32752=CARTESIAN_POINT('Ctrl Pts',(30.3668601442724,33.100157768821,174.11247461304));
#32753=CARTESIAN_POINT('Ctrl Pts',(32.0384371898907,33.968759885587,174.00134482382));
#32754=CARTESIAN_POINT('Ctrl Pts',(33.674836936155,33.0355743053757,173.890215034601));
#32755=CARTESIAN_POINT('Ctrl Pts',(33.7784440813005,31.1546423512202,173.779085245381));
#32756=CARTESIAN_POINT('Ctrl Pts',(32.2544384896628,30.047372549706,173.667955456161));
#32757=CARTESIAN_POINT('Ctrl Pts',(30.4975735515562,30.727126215338,173.556825666941));
#32758=CARTESIAN_POINT('Ctrl Pts',(30.115713005929,32.5718001649512,173.445695877722));
#32759=CARTESIAN_POINT('Ctrl Pts',(31.458331483034,33.8931688045157,173.334566088502));
#32760=CARTESIAN_POINT('Ctrl Pts',(33.2966791127159,33.4819298847482,173.223436299282));
#32761=CARTESIAN_POINT('Ctrl Pts',(33.9483200803396,31.7144448053196,173.112306510062));
#32762=CARTESIAN_POINT('Ctrl Pts',(32.8168796390879,30.2082967433453,173.001176720843));
#32763=CARTESIAN_POINT('Ctrl Pts',(30.9378398108339,30.3418960716488,172.890046931623));
#32764=CARTESIAN_POINT('Ctrl Pts',(30.030877469057,31.9929741337908,172.778917142403));
#32765=CARTESIAN_POINT('Ctrl Pts',(30.9260347133546,33.6504821924952,172.667787353184));
#32766=CARTESIAN_POINT('Ctrl Pts',(32.8040733413214,33.797486847362,172.556657563964));
#32767=CARTESIAN_POINT('Ctrl Pts',(33.9462327671232,32.2994510324562,172.445527774744));
#32768=CARTESIAN_POINT('Ctrl Pts',(33.3072210704694,30.5273608800578,172.334397985524));
#32769=CARTESIAN_POINT('Ctrl Pts',(31.4718548263441,30.1030140801241,172.223268196305));
#32770=CARTESIAN_POINT('Ctrl Pts',(30.1198413176528,31.4147682221052,172.112138407085));
#32771=CARTESIAN_POINT('Ctrl Pts',(30.4885286455738,33.2621201406413,172.001008617865));
#32772=CARTESIAN_POINT('Ctrl Pts',(32.2404981658413,33.9543933935854,171.889878828646));
#32773=CARTESIAN_POINT('Ctrl Pts',(33.7723663728249,32.858027007234,171.778749039426));
#32774=CARTESIAN_POINT('Ctrl Pts',(33.6821840959121,30.9764036087774,171.667619250206));
#32775=CARTESIAN_POINT('Ctrl Pts',(32.0524851769474,30.0315645271271,171.556489460986));
#32776=CARTESIAN_POINT('Ctrl Pts',(30.3747523932185,30.8882162434563,171.445359671767));
#32777=CARTESIAN_POINT('Ctrl Pts',(30.1844285941397,32.7623603969814,171.334229882547));
#32778=CARTESIAN_POINT('Ctrl Pts',(31.6556960566522,33.9388005826434,171.223100093327));
#32779=CARTESIAN_POINT('Ctrl Pts',(33.4420667542958,33.340871500487,171.111970304107));
#32780=CARTESIAN_POINT('Ctrl Pts',(33.9086735969707,31.5157913622307,171.000840514888));
#32781=CARTESIAN_POINT('Ctrl Pts',(32.6284830624013,30.133853718237,170.889710725668));
#32782=CARTESIAN_POINT('Ctrl Pts',(30.7731116447372,30.4597929137989,170.778580936448));
#32783=CARTESIAN_POINT('Ctrl Pts',(30.0405751447595,32.1953129318018,170.667451147229));
#32784=CARTESIAN_POINT('Ctrl Pts',(31.1012830232201,33.7520846727002,170.556321358009));
#32785=CARTESIAN_POINT('Ctrl Pts',(32.98448693265,33.7053675217104,170.445191568789));
#32786=CARTESIAN_POINT('Ctrl Pts',(33.9666990776347,32.0979165087919,170.334061779569));
#32787=CARTESIAN_POINT('Ctrl Pts',(33.1490095547316,30.4008533688874,170.22293199035));
#32788=CARTESIAN_POINT('Ctrl Pts',(31.2797589478278,30.167311883754,170.11180220113));
#32789=CARTESIAN_POINT('Ctrl Pts',(30.0696651411831,31.611026687934,170.00067241191));
#32790=CARTESIAN_POINT('Ctrl Pts',(30.6261928637177,33.4107256490767,169.88954262269));
#32791=CARTESIAN_POINT('Ctrl Pts',(32.4400139790599,33.9193437948674,169.778412833471));
#32792=CARTESIAN_POINT('Ctrl Pts',(33.8511390725192,32.6713993140116,169.667283044251));
#32793=CARTESIAN_POINT('Ctrl Pts',(33.5681217615767,30.8089974619958,169.556153255031));
#32794=CARTESIAN_POINT('Ctrl Pts',(31.8499764200105,30.0365882168748,169.445023465812));
#32795=CARTESIAN_POINT('Ctrl Pts',(30.2691310319151,31.0610721433597,169.333893676592));
#32796=CARTESIAN_POINT('Ctrl Pts',(30.2723581529136,32.9448526619855,169.222763887372));
#32797=CARTESIAN_POINT('Ctrl Pts',(31.8567043568802,33.9639142708781,169.111634098152));
#32798=CARTESIAN_POINT('Ctrl Pts',(33.5721931794324,33.1856228367951,169.000504308933));
#32799=CARTESIAN_POINT('Ctrl Pts',(33.8488278539362,31.3222622400855,168.889374519713));
#32800=CARTESIAN_POINT('Ctrl Pts',(32.433435326133,30.0791598913592,168.778244730493));
#32801=CARTESIAN_POINT('Ctrl Pts',(30.6213674884419,30.5939895796832,168.667114941273));
#32802=CARTESIAN_POINT('Ctrl Pts',(30.0710091743181,32.3955847565919,168.555985152054));
#32803=CARTESIAN_POINT('Ctrl Pts',(31.2860423455642,33.8351450553073,168.444855362834));
#32804=CARTESIAN_POINT('Ctrl Pts',(33.1544818180945,33.5952004984823,168.333725573614));
#32805=CARTESIAN_POINT('Ctrl Pts',(33.966352053607,31.895345749241,168.222595784395));
#32806=CARTESIAN_POINT('Ctrl Pts',(32.9786382076115,30.291269426071,168.111465995175));
#32807=CARTESIAN_POINT('Ctrl Pts',(31.0952852996177,30.2510048126737,168.000336205955));
#32808=CARTESIAN_POINT('Ctrl Pts',(30.039917448298,31.8114015891261,167.889206416735));
#32809=CARTESIAN_POINT('Ctrl Pts',(30.7783959448026,33.544401664386,167.778076627515));
#32810=CARTESIAN_POINT('Ctrl Pts',(32.6348731175525,33.8639819250408,167.666946838296));
#32811=CARTESIAN_POINT('Ctrl Pts',(33.9103215165394,32.4776664670713,167.555817049076));
#32812=CARTESIAN_POINT('Ctrl Pts',(33.4374639352983,30.6541951765766,167.444687259857));
#32813=CARTESIAN_POINT('Ctrl Pts',(31.6490558548275,30.0623912134843,167.333557470637));
#32814=CARTESIAN_POINT('Ctrl Pts',(30.1818262062432,31.2438630556162,167.222427681417));
#32815=CARTESIAN_POINT('Ctrl Pts',(30.3785732505457,33.1173488152295,167.111297892197));
#32816=CARTESIAN_POINT('Ctrl Pts',(32.0592248292506,33.9682376837793,167.000168102978));
#32817=CARTESIAN_POINT('Ctrl Pts',(33.6856900471062,33.0178399222439,166.889038313758));
#32818=CARTESIAN_POINT('Ctrl Pts',(33.76939833431,31.1358789634033,166.777908524538));
#32819=CARTESIAN_POINT('Ctrl Pts',(32.2338369522489,30.0448481762927,166.666778735318));
#32820=CARTESIAN_POINT('Ctrl Pts',(30.484139214776,30.7429557473555,166.555648946099));
#32821=CARTESIAN_POINT('Ctrl Pts',(30.1220081713125,32.5918944065121,166.444519156879));
#32822=CARTESIAN_POINT('Ctrl Pts',(31.4780505358289,33.8983275199854,166.333389367659));
#32823=CARTESIAN_POINT('Ctrl Pts',(33.3128835277701,33.4690889075443,166.222259578439));
#32824=CARTESIAN_POINT('Ctrl Pts',(33.9439005615907,31.6919390350863,166.11112978922));
#32825=CARTESIAN_POINT('Ctrl Pts',(33.1815065089967,30.7013650994246,166.037043263073));
#32826=CARTESIAN_POINT('Ctrl Pts',(32.6750771856741,30.4769022377462,166.));
#32827=CARTESIAN_POINT('Ctrl Pts',(30.3361333853116,32.0009462961084,178.37851963661));
#32828=CARTESIAN_POINT('Ctrl Pts',(30.3350134449002,32.216507009066,178.364148625537));
#32829=CARTESIAN_POINT('Ctrl Pts',(30.373884681584,32.431680346969,178.349777614463));
#32830=CARTESIAN_POINT('Ctrl Pts',(30.4546197953249,32.6297920446191,178.33540660339));
#32831=CARTESIAN_POINT('Ctrl Pts',(30.6627256858759,33.140452268625,178.298363340316));
#32832=CARTESIAN_POINT('Ctrl Pts',(31.1489842701054,33.5377512483192,178.261320077243));
#32833=CARTESIAN_POINT('Ctrl Pts',(31.690876656062,33.639897472402,178.22427681417));
#32834=CARTESIAN_POINT('Ctrl Pts',(32.2327690420186,33.7420436964848,178.187233551097));
#32835=CARTESIAN_POINT('Ctrl Pts',(32.8302952297023,33.5490371649563,178.150190288023));
#32836=CARTESIAN_POINT('Ctrl Pts',(33.2100351911184,33.1491915376066,178.11314702495));
#32837=CARTESIAN_POINT('Ctrl Pts',(33.5897751525344,32.749345910257,178.076103761877));
#32838=CARTESIAN_POINT('Ctrl Pts',(33.7517288876827,32.1426611870862,178.039060498804));
#32839=CARTESIAN_POINT('Ctrl Pts',(33.6217849293405,31.6067555042284,178.002017235731));
#32840=CARTESIAN_POINT('Ctrl Pts',(33.4918409709983,31.0708498213705,177.964973972657));
#32841=CARTESIAN_POINT('Ctrl Pts',(33.0699993191655,30.6057231788256,177.927930709584));
#32842=CARTESIAN_POINT('Ctrl Pts',(32.5492935640385,30.4242137799862,177.890887446511));
#32843=CARTESIAN_POINT('Ctrl Pts',(32.0285878089115,30.2427043811468,177.853844183437));
#32844=CARTESIAN_POINT('Ctrl Pts',(31.4090179504904,30.344812226013,177.816800920364));
#32845=CARTESIAN_POINT('Ctrl Pts',(30.974095237716,30.6838139207111,177.779757657291));
#32846=CARTESIAN_POINT('Ctrl Pts',(30.5778854104528,30.9926407512105,177.746011650397));
#32847=CARTESIAN_POINT('Ctrl Pts',(30.3349144418051,31.4980660345814,177.712265643504));
#32848=CARTESIAN_POINT('Ctrl Pts',(30.3317667672262,32.0008552724323,177.67851963661));
#32849=CARTESIAN_POINT('Ctrl Pts',(31.4698297828098,30.0148256743287,179.));
#32850=CARTESIAN_POINT('Ctrl Pts',(31.4011717602422,30.0402471946251,179.));
#32851=CARTESIAN_POINT('Ctrl Pts',(31.3342170200572,30.0695594652625,179.));
#32852=CARTESIAN_POINT('Ctrl Pts',(31.2691543791405,30.1024681435714,179.));
#32853=CARTESIAN_POINT('Ctrl Pts',(31.2022750866749,30.1362956840811,179.));
#32854=CARTESIAN_POINT('Ctrl Pts',(31.1373942576578,30.173923959486,179.));
#32855=CARTESIAN_POINT('Ctrl Pts',(31.0747481851605,30.215077936283,179.));
#32856=CARTESIAN_POINT('Ctrl Pts',(31.0218169218836,30.2498499801463,179.));
#32857=CARTESIAN_POINT('Ctrl Pts',(30.9704813835458,30.287140070486,179.));
#32858=CARTESIAN_POINT('Ctrl Pts',(30.920906837578,30.3268003233183,179.));
#32859=CARTESIAN_POINT('Ctrl Pts',(30.8988714689694,30.3444288920366,179.));
#32860=CARTESIAN_POINT('Ctrl Pts',(30.8771843246632,30.3625259150697,179.));
#32861=CARTESIAN_POINT('Ctrl Pts',(30.8558614729043,30.381079129876,179.));
#32862=CARTESIAN_POINT('Ctrl Pts',(30.8441499657732,30.391269422899,179.));
#32863=CARTESIAN_POINT('Ctrl Pts',(30.8325483731912,30.401597342812,179.));
#32864=CARTESIAN_POINT('Ctrl Pts',(30.8210594917678,30.412060899429,179.));
#32865=CARTESIAN_POINT('Ctrl Pts',(30.8104646293746,30.4217102237116,179.));
#32866=CARTESIAN_POINT('Ctrl Pts',(30.7999641824858,30.4314764150215,179.));
#32867=CARTESIAN_POINT('Ctrl Pts',(30.7895762380615,30.4413424485534,179.));
#32868=CARTESIAN_POINT('Ctrl Pts',(30.7364925281002,30.4917591278393,179.));
#32869=CARTESIAN_POINT('Ctrl Pts',(30.6862488525372,30.5448645642236,179.));
#32870=CARTESIAN_POINT('Ctrl Pts',(30.6390638156957,30.6003988925952,179.));
#32871=CARTESIAN_POINT('Ctrl Pts',(30.5922436254276,30.6555038155712,179.));
#32872=CARTESIAN_POINT('Ctrl Pts',(30.5484344479305,30.7130010983928,179.));
#32873=CARTESIAN_POINT('Ctrl Pts',(30.5078946509714,30.7726610952581,179.));
#32874=CARTESIAN_POINT('Ctrl Pts',(30.4742099869881,30.8222328025285,179.));
#32875=CARTESIAN_POINT('Ctrl Pts',(30.4427831503197,30.8732983012023,179.));
#32876=CARTESIAN_POINT('Ctrl Pts',(30.4137899491081,30.9257323179221,179.));
#32877=CARTESIAN_POINT('Ctrl Pts',(30.4016832698065,30.9476271690731,179.));
#32878=CARTESIAN_POINT('Ctrl Pts',(30.3900012514895,30.9697606799659,179.));
#32879=CARTESIAN_POINT('Ctrl Pts',(30.3787581361903,30.9921238118577,179.));
#32880=CARTESIAN_POINT('Ctrl Pts',(30.3735598930403,31.0024633835934,179.));
#32881=CARTESIAN_POINT('Ctrl Pts',(30.3684554850874,31.0128520405776,179.));
#32882=CARTESIAN_POINT('Ctrl Pts',(30.3634463850541,31.0232888874584,179.));
#32883=CARTESIAN_POINT('Ctrl Pts',(30.3582116938596,31.0341957709509,179.));
#32884=CARTESIAN_POINT('Ctrl Pts',(30.3530846911292,31.0451478442412,179.));
#32885=CARTESIAN_POINT('Ctrl Pts',(30.348068454379,31.056139759175,179.));
#32886=CARTESIAN_POINT('Ctrl Pts',(30.3195275799257,31.118680440517,179.));
#32887=CARTESIAN_POINT('Ctrl Pts',(30.2945477318953,31.1825532780501,179.));
#32888=CARTESIAN_POINT('Ctrl Pts',(30.2733523356296,31.2475534440222,179.));
#32889=CARTESIAN_POINT('Ctrl Pts',(30.2541560446554,31.3064229307604,179.));
#32890=CARTESIAN_POINT('Ctrl Pts',(30.2380643124207,31.3662177179318,179.));
#32891=CARTESIAN_POINT('Ctrl Pts',(30.2252797771608,31.4267904453086,179.));
#32892=CARTESIAN_POINT('Ctrl Pts',(30.2101450523644,31.4984982970514,179.));
#32893=CARTESIAN_POINT('Ctrl Pts',(30.1996446092358,31.5712979137807,179.));
#32894=CARTESIAN_POINT('Ctrl Pts',(30.1937033974617,31.6447666213231,179.));
#32895=CARTESIAN_POINT('Ctrl Pts',(30.1923961005744,31.660932584822,179.));
#32896=CARTESIAN_POINT('Ctrl Pts',(30.1913097719617,31.6771308619873,179.));
#32897=CARTESIAN_POINT('Ctrl Pts',(30.1904439810637,31.6933567855583,179.));
#32898=CARTESIAN_POINT('Ctrl Pts',(30.1895460489563,31.7101850725971,179.));
#32899=CARTESIAN_POINT('Ctrl Pts',(30.1888853223853,31.7270493233257,179.));
#32900=CARTESIAN_POINT('Ctrl Pts',(30.1884618847505,31.7439099359327,179.));
#32901=CARTESIAN_POINT('Ctrl Pts',(30.1867401602096,31.8124662665857,179.));
#32902=CARTESIAN_POINT('Ctrl Pts',(30.1889297506264,31.881048937226,179.));
#32903=CARTESIAN_POINT('Ctrl Pts',(30.1949101630748,31.9493199653033,179.));
#32904=CARTESIAN_POINT('Ctrl Pts',(30.200889360023,32.017577117506,179.));
#32905=CARTESIAN_POINT('Ctrl Pts',(30.2106582916318,32.0855238245582,179.));
#32906=CARTESIAN_POINT('Ctrl Pts',(30.2241461415959,32.1528072679591,179.));
#32907=CARTESIAN_POINT('Ctrl Pts',(30.23390407838,32.2014842319721,179.));
#32908=CARTESIAN_POINT('Ctrl Pts',(30.2456095327489,32.2498137804381,179.));
#32909=CARTESIAN_POINT('Ctrl Pts',(30.2592498872082,32.2976526714744,179.));
#32910=CARTESIAN_POINT('Ctrl Pts',(30.2694853722893,32.3335501444441,179.));
#32911=CARTESIAN_POINT('Ctrl Pts',(30.2808105985582,32.3691711861731,179.));
#32912=CARTESIAN_POINT('Ctrl Pts',(30.293224150216,32.404451098837,179.));
#32913=CARTESIAN_POINT('Ctrl Pts',(30.2973533131521,32.4161863790998,179.));
#32914=CARTESIAN_POINT('Ctrl Pts',(30.3015996987641,32.4278747200823,179.));
#32915=CARTESIAN_POINT('Ctrl Pts',(30.3059626641326,32.4395135673061,179.));
#32916=CARTESIAN_POINT('Ctrl Pts',(30.3290856800155,32.5011975887183,179.));
#32917=CARTESIAN_POINT('Ctrl Pts',(30.3554815681533,32.561497971648,179.));
#32918=CARTESIAN_POINT('Ctrl Pts',(30.3851004076594,32.6200808955868,179.));
#32919=CARTESIAN_POINT('Ctrl Pts',(30.4059270031276,32.6612736930956,179.));
#32920=CARTESIAN_POINT('Ctrl Pts',(30.4283479615027,32.7016168064163,179.));
#32921=CARTESIAN_POINT('Ctrl Pts',(30.4523563217739,32.7409828457338,179.));
#32922=CARTESIAN_POINT('Ctrl Pts',(30.4600693931975,32.7536298182672,179.));
#32923=CARTESIAN_POINT('Ctrl Pts',(30.4679474569151,32.7661775460074,179.));
#32924=CARTESIAN_POINT('Ctrl Pts',(30.4759869702196,32.7786161898381,179.));
#32925=CARTESIAN_POINT('Ctrl Pts',(30.5102319100181,32.8315995724167,179.));
#32926=CARTESIAN_POINT('Ctrl Pts',(30.5473331969222,32.8824994972081,179.));
#32927=CARTESIAN_POINT('Ctrl Pts',(30.5872566572931,32.9310009671585,179.));
#32928=CARTESIAN_POINT('Ctrl Pts',(30.6240225851301,32.9756664727941,179.));
#32929=CARTESIAN_POINT('Ctrl Pts',(30.6631825179533,33.0182979966642,179.));
#32930=CARTESIAN_POINT('Ctrl Pts',(30.704731170499,33.0586167056725,179.));
#32931=CARTESIAN_POINT('Ctrl Pts',(30.7125728682978,33.066226269697,179.));
#32932=CARTESIAN_POINT('Ctrl Pts',(30.7204997080418,33.0737533451809,179.));
#32933=CARTESIAN_POINT('Ctrl Pts',(30.728510082833,33.081197258918,179.));
#32934=CARTESIAN_POINT('Origin',(32.,32.,172.));
#32935=CARTESIAN_POINT('Origin',(-32.,-32.,166.));
#32936=CARTESIAN_POINT('Ctrl Pts',(-31.3249228143252,-33.5230977622534,
166.));
#32937=CARTESIAN_POINT('Ctrl Pts',(-31.2652496657111,-33.5045147077491,
166.));
#32938=CARTESIAN_POINT('Ctrl Pts',(-31.2068892780268,-33.4823562231994,
166.));
#32939=CARTESIAN_POINT('Ctrl Pts',(-31.1499979698121,-33.4569214879221,
166.));
#32940=CARTESIAN_POINT('Ctrl Pts',(-31.1139308831639,-33.440796761142,166.));
#32941=CARTESIAN_POINT('Ctrl Pts',(-31.0784541858883,-33.4233541702623,
166.));
#32942=CARTESIAN_POINT('Ctrl Pts',(-31.0436086065906,-33.4046595162816,
166.));
#32943=CARTESIAN_POINT('Ctrl Pts',(-31.020037064781,-33.3920133836358,166.));
#32944=CARTESIAN_POINT('Ctrl Pts',(-30.9967543373406,-33.3787941494722,
166.));
#32945=CARTESIAN_POINT('Ctrl Pts',(-30.9737734827442,-33.3650202765066,
166.));
#32946=CARTESIAN_POINT('Ctrl Pts',(-30.9613024215807,-33.3575455844106,
166.));
#32947=CARTESIAN_POINT('Ctrl Pts',(-30.9489201683257,-33.3499073220363,
166.));
#32948=CARTESIAN_POINT('Ctrl Pts',(-30.9366413906613,-33.3421166398709,
166.));
#32949=CARTESIAN_POINT('Ctrl Pts',(-30.8809436659781,-33.3067773510422,
166.));
#32950=CARTESIAN_POINT('Ctrl Pts',(-30.82730918088,-33.2682678880975,166.));
#32951=CARTESIAN_POINT('Ctrl Pts',(-30.7759194947972,-33.2268911757215,
166.));
#32952=CARTESIAN_POINT('Ctrl Pts',(-30.738836022715,-33.1970331969088,166.));
#32953=CARTESIAN_POINT('Ctrl Pts',(-30.7029215593492,-33.1656809490029,
166.));
#32954=CARTESIAN_POINT('Ctrl Pts',(-30.6682496155875,-33.1329323650887,
166.));
#32955=CARTESIAN_POINT('Ctrl Pts',(-30.6588709943895,-33.124074004986,166.));
#32956=CARTESIAN_POINT('Ctrl Pts',(-30.6495833196648,-33.1151134090585,
166.));
#32957=CARTESIAN_POINT('Ctrl Pts',(-30.640388127734,-33.1060523678756,166.));
#32958=CARTESIAN_POINT('Ctrl Pts',(-30.6306794907576,-33.0964853724138,
166.));
#32959=CARTESIAN_POINT('Ctrl Pts',(-30.6210793827335,-33.0868116833964,
166.));
#32960=CARTESIAN_POINT('Ctrl Pts',(-30.6115938499237,-33.0770385931226,
166.));
#32961=CARTESIAN_POINT('Ctrl Pts',(-30.564337834939,-33.0283499944233,166.));
#32962=CARTESIAN_POINT('Ctrl Pts',(-30.5198880169309,-32.9771627809512,
166.));
#32963=CARTESIAN_POINT('Ctrl Pts',(-30.4784278661767,-32.9237844624066,
166.));
#32964=CARTESIAN_POINT('Ctrl Pts',(-30.4363632851573,-32.8696279635937,
166.));
#32965=CARTESIAN_POINT('Ctrl Pts',(-30.3973752864255,-32.8132154260561,
166.));
#32966=CARTESIAN_POINT('Ctrl Pts',(-30.361679837689,-32.7548210768249,166.));
#32967=CARTESIAN_POINT('Ctrl Pts',(-30.3395645388112,-32.7186425573852,
166.));
#32968=CARTESIAN_POINT('Ctrl Pts',(-30.3187136102408,-32.6817024296689,
166.));
#32969=CARTESIAN_POINT('Ctrl Pts',(-30.2991853292908,-32.6440586298174,
166.));
#32970=CARTESIAN_POINT('Ctrl Pts',(-30.2832062943298,-32.6132565538216,
166.));
#32971=CARTESIAN_POINT('Ctrl Pts',(-30.2681128991308,-32.5819832290257,
166.));
#32972=CARTESIAN_POINT('Ctrl Pts',(-30.2539403906387,-32.5502681863268,
166.));
#32973=CARTESIAN_POINT('Ctrl Pts',(-30.2481177635283,-32.5372383922343,
166.));
#32974=CARTESIAN_POINT('Ctrl Pts',(-30.2424496988302,-32.5241314966566,
166.));
#32975=CARTESIAN_POINT('Ctrl Pts',(-30.2369478542267,-32.5109721386666,
166.));
#32976=CARTESIAN_POINT('Ctrl Pts',(-30.2097573184397,-32.4459375875024,
166.));
#32977=CARTESIAN_POINT('Ctrl Pts',(-30.1865718984384,-32.379512851388,166.));
#32978=CARTESIAN_POINT('Ctrl Pts',(-30.167602992408,-32.3119935916337,166.));
#32979=CARTESIAN_POINT('Ctrl Pts',(-30.1654998512031,-32.3045075227436,
166.));
#32980=CARTESIAN_POINT('Ctrl Pts',(-30.1634485787457,-32.297007960316,166.));
#32981=CARTESIAN_POINT('Ctrl Pts',(-30.1614494913157,-32.2894952795695,
166.));
#32982=CARTESIAN_POINT('Ctrl Pts',(-30.144109446168,-32.2243304341649,166.));
#32983=CARTESIAN_POINT('Ctrl Pts',(-30.130691802039,-32.1581806460084,166.));
#32984=CARTESIAN_POINT('Ctrl Pts',(-30.1210426074296,-32.0913500757851,
166.));
#32985=CARTESIAN_POINT('Ctrl Pts',(-30.1106636454464,-32.0194651179478,
166.));
#32986=CARTESIAN_POINT('Ctrl Pts',(-30.1046440842174,-31.9467917171052,
166.));
#32987=CARTESIAN_POINT('Ctrl Pts',(-30.102852468024,-31.873685883042,166.));
#32988=CARTESIAN_POINT('Ctrl Pts',(-30.1025311821446,-31.8605760036622,
166.));
#32989=CARTESIAN_POINT('Ctrl Pts',(-30.1023460194269,-31.8474521833933,
166.));
#32990=CARTESIAN_POINT('Ctrl Pts',(-30.1022964301738,-31.8343164404446,
166.));
#32991=CARTESIAN_POINT('Ctrl Pts',(-30.102251899601,-31.8225206959586,166.));
#32992=CARTESIAN_POINT('Ctrl Pts',(-30.102316746396,-31.8107240263089,166.));
#32993=CARTESIAN_POINT('Ctrl Pts',(-30.1024900270227,-31.7989311721439,
166.));
#32994=CARTESIAN_POINT('Ctrl Pts',(-30.1035341466453,-31.7278721583389,
166.));
#32995=CARTESIAN_POINT('Ctrl Pts',(-30.1085110510928,-31.6569165693418,
166.));
#32996=CARTESIAN_POINT('Ctrl Pts',(-30.1172407253237,-31.5863996593262,
166.));
#32997=CARTESIAN_POINT('Ctrl Pts',(-30.1261541825071,-31.51439818006,166.));
#32998=CARTESIAN_POINT('Ctrl Pts',(-30.1389800306763,-31.442853110017,166.));
#32999=CARTESIAN_POINT('Ctrl Pts',(-30.1555793421879,-31.372105161476,166.));
#33000=CARTESIAN_POINT('Ctrl Pts',(-30.1722789678255,-31.3009296639604,
166.));
#33001=CARTESIAN_POINT('Ctrl Pts',(-30.1927978814359,-31.230559881898,166.));
#33002=CARTESIAN_POINT('Ctrl Pts',(-30.2170470200302,-31.1613418292143,
166.));
#33003=CARTESIAN_POINT('Ctrl Pts',(-30.2230312117698,-31.1442602286663,
166.));
#33004=CARTESIAN_POINT('Ctrl Pts',(-30.2292428199321,-31.1272488082428,
166.));
#33005=CARTESIAN_POINT('Ctrl Pts',(-30.2356809841796,-31.1103128783636,
166.));
#33006=CARTESIAN_POINT('Ctrl Pts',(-30.2407433191753,-31.0969961397381,
166.));
#33007=CARTESIAN_POINT('Ctrl Pts',(-30.2459464874926,-31.083724508723,166.));
#33008=CARTESIAN_POINT('Ctrl Pts',(-30.2512816614537,-31.0705206906996,
166.));
#33009=CARTESIAN_POINT('Ctrl Pts',(-30.2795038863081,-31.0006745856034,
166.));
#33010=CARTESIAN_POINT('Ctrl Pts',(-30.3114625623906,-30.932599286949,166.));
#33011=CARTESIAN_POINT('Ctrl Pts',(-30.3469997430835,-30.8666517028784,
166.));
#33012=CARTESIAN_POINT('Ctrl Pts',(-30.3825752356235,-30.8006330221788,
166.));
#33013=CARTESIAN_POINT('Ctrl Pts',(-30.4217371239017,-30.7367455318663,
166.));
#33014=CARTESIAN_POINT('Ctrl Pts',(-30.4643787139105,-30.6753517285781,
166.));
#33015=CARTESIAN_POINT('Ctrl Pts',(-30.5060510273331,-30.6153534543042,
166.));
#33016=CARTESIAN_POINT('Ctrl Pts',(-30.5510469857941,-30.5577358065873,
166.));
#33017=CARTESIAN_POINT('Ctrl Pts',(-30.5993123466261,-30.5028567349083,
166.));
#33018=CARTESIAN_POINT('Ctrl Pts',(-30.6096397636154,-30.4911141715577,
166.));
#33019=CARTESIAN_POINT('Ctrl Pts',(-30.620117024632,-30.479497094178,166.));
#33020=CARTESIAN_POINT('Ctrl Pts',(-30.6307438541099,-30.4680091959517,
166.));
#33021=CARTESIAN_POINT('Ctrl Pts',(-30.6398545489831,-30.4581602814009,
166.));
#33022=CARTESIAN_POINT('Ctrl Pts',(-30.649075180594,-30.4484063167597,166.));
#33023=CARTESIAN_POINT('Ctrl Pts',(-30.6584038878141,-30.4387477190139,
166.));
#33024=CARTESIAN_POINT('Ctrl Pts',(-31.6163320011535,-29.981387499008,166.));
#33025=CARTESIAN_POINT('Ctrl Pts',(-31.6906427498098,-29.9743675630937,
166.));
#33026=CARTESIAN_POINT('Ctrl Pts',(-31.7652022960126,-29.9717511873187,
166.));
#33027=CARTESIAN_POINT('Ctrl Pts',(-31.8396884569134,-29.9733742829586,
166.));
#33028=CARTESIAN_POINT('Ctrl Pts',(-31.9122243289139,-29.9749548806987,
166.));
#33029=CARTESIAN_POINT('Ctrl Pts',(-31.9846913912953,-29.9805565001925,
166.));
#33030=CARTESIAN_POINT('Ctrl Pts',(-32.0567789152228,-29.9900714754047,
166.));
#33031=CARTESIAN_POINT('Ctrl Pts',(-32.0728687041251,-29.9921951985434,
166.));
#33032=CARTESIAN_POINT('Ctrl Pts',(-32.088941631761,-29.9945143667354,166.));
#33033=CARTESIAN_POINT('Ctrl Pts',(-32.1049872983986,-29.9970269692978,
166.));
#33034=CARTESIAN_POINT('Ctrl Pts',(-32.1786235674407,-30.0085577260099,
166.));
#33035=CARTESIAN_POINT('Ctrl Pts',(-32.2515406107965,-30.0241342606475,
166.));
#33036=CARTESIAN_POINT('Ctrl Pts',(-32.3234063396469,-30.0436165375461,
166.));
#33037=CARTESIAN_POINT('Ctrl Pts',(-32.3738567729472,-30.0572932834295,
166.));
#33038=CARTESIAN_POINT('Ctrl Pts',(-32.423788826305,-30.0728959391103,166.));
#33039=CARTESIAN_POINT('Ctrl Pts',(-32.4730796706315,-30.090389199647,166.));
#33040=CARTESIAN_POINT('Ctrl Pts',(-32.4918010193241,-30.0970333834656,
166.));
#33041=CARTESIAN_POINT('Ctrl Pts',(-32.5104297849499,-30.1039504059982,
166.));
#33042=CARTESIAN_POINT('Ctrl Pts',(-32.5289589042585,-30.1111386947073,
166.));
#33043=CARTESIAN_POINT('Ctrl Pts',(-32.546660933288,-30.1180061174533,166.));
#33044=CARTESIAN_POINT('Ctrl Pts',(-32.5642774893601,-30.1251235901428,
166.));
#33045=CARTESIAN_POINT('Ctrl Pts',(-32.5817714522529,-30.1324764898979,
166.));
#33046=CARTESIAN_POINT('Ctrl Pts',(-32.6487029901528,-30.1606085313138,
166.));
#33047=CARTESIAN_POINT('Ctrl Pts',(-32.7139143733596,-30.192208709252,166.));
#33048=CARTESIAN_POINT('Ctrl Pts',(-32.7770972324966,-30.2271493585151,
166.));
#33049=CARTESIAN_POINT('Ctrl Pts',(-32.8389246041363,-30.2613404118613,
166.));
#33050=CARTESIAN_POINT('Ctrl Pts',(-32.89881025273,-30.2987307725668,166.));
#33051=CARTESIAN_POINT('Ctrl Pts',(-32.9564328602487,-30.3392376279317,
166.));
#33052=CARTESIAN_POINT('Ctrl Pts',(-33.0127911310432,-30.3788556949021,
166.));
#33053=CARTESIAN_POINT('Ctrl Pts',(-33.0669851431482,-30.4214555217774,
166.));
#33054=CARTESIAN_POINT('Ctrl Pts',(-33.1186738211267,-30.4669868293286,
166.));
#33055=CARTESIAN_POINT('Ctrl Pts',(-33.1354927563908,-30.4818022230307,
166.));
#33056=CARTESIAN_POINT('Ctrl Pts',(-33.1520460717911,-30.4969281821769,
166.));
#33057=CARTESIAN_POINT('Ctrl Pts',(-33.1683209144445,-30.5123634761981,
166.));
#33058=CARTESIAN_POINT('Ctrl Pts',(-33.1774555438763,-30.5210268896673,
166.));
#33059=CARTESIAN_POINT('Ctrl Pts',(-33.1865032709774,-30.5297887184969,
166.));
#33060=CARTESIAN_POINT('Ctrl Pts',(-33.1954493554731,-30.538636114803,166.));
#33061=CARTESIAN_POINT('Ctrl Pts',(-33.2440184737772,-30.5866694458182,
166.));
#33062=CARTESIAN_POINT('Ctrl Pts',(-33.2896825812191,-30.6373038648715,
166.));
#33063=CARTESIAN_POINT('Ctrl Pts',(-33.3321491427106,-30.6904579124732,
166.));
#33064=CARTESIAN_POINT('Ctrl Pts',(-33.3382530454572,-30.698097973871,166.));
#33065=CARTESIAN_POINT('Ctrl Pts',(-33.3442908157837,-30.7057901395772,
166.));
#33066=CARTESIAN_POINT('Ctrl Pts',(-33.3502615092167,-30.7135342161227,
166.));
#33067=CARTESIAN_POINT('Ctrl Pts',(-33.3926204742275,-30.7684744121174,
166.));
#33068=CARTESIAN_POINT('Ctrl Pts',(-33.4316074125864,-30.8260259901118,
166.));
#33069=CARTESIAN_POINT('Ctrl Pts',(-33.4671552055421,-30.8858271868844,
166.));
#33070=CARTESIAN_POINT('Ctrl Pts',(-33.5003164101228,-30.9416134834574,
166.));
#33071=CARTESIAN_POINT('Ctrl Pts',(-33.5304843566103,-30.999358447659,166.));
#33072=CARTESIAN_POINT('Ctrl Pts',(-33.557564843168,-31.0587738345715,166.));
#33073=CARTESIAN_POINT('Ctrl Pts',(-33.5634601879376,-31.0717083950244,
166.));
#33074=CARTESIAN_POINT('Ctrl Pts',(-33.569209065161,-31.0847221124707,166.));
#33075=CARTESIAN_POINT('Ctrl Pts',(-33.5748102571412,-31.097811985643,166.));
#33076=CARTESIAN_POINT('Ctrl Pts',(-33.5793367581237,-31.1083903275362,
166.));
#33077=CARTESIAN_POINT('Ctrl Pts',(-33.5837665821197,-31.1190180990339,
166.));
#33078=CARTESIAN_POINT('Ctrl Pts',(-33.588094067069,-31.1296806929919,166.));
#33079=CARTESIAN_POINT('Ctrl Pts',(-33.6138045316752,-31.1930293233811,
166.));
#33080=CARTESIAN_POINT('Ctrl Pts',(-33.6359574101316,-31.2577224771475,
166.));
#33081=CARTESIAN_POINT('Ctrl Pts',(-33.6545065508599,-31.3234105339755,
166.));
#33082=CARTESIAN_POINT('Ctrl Pts',(-33.6729704001367,-31.3887965482564,
166.));
#33083=CARTESIAN_POINT('Ctrl Pts',(-33.6878635838304,-31.455169472032,166.));
#33084=CARTESIAN_POINT('Ctrl Pts',(-33.699089518876,-31.5221871118774,166.));
#33085=CARTESIAN_POINT('Ctrl Pts',(-33.7100754114707,-31.5877717237873,
166.));
#33086=CARTESIAN_POINT('Ctrl Pts',(-33.7175490812715,-31.6539747381941,
166.));
#33087=CARTESIAN_POINT('Ctrl Pts',(-33.7213721137454,-31.7204625720356,
166.));
#33088=CARTESIAN_POINT('Ctrl Pts',(-33.7221759623023,-31.7344426126579,
166.));
#33089=CARTESIAN_POINT('Ctrl Pts',(-33.722818243567,-31.7484351706062,166.));
#33090=CARTESIAN_POINT('Ctrl Pts',(-33.7232974015415,-31.7624370101449,
166.));
#33091=CARTESIAN_POINT('Ctrl Pts',(-33.7237537916425,-31.7757735323356,
166.));
#33092=CARTESIAN_POINT('Ctrl Pts',(-33.7240620939902,-31.7891203356115,
166.));
#33093=CARTESIAN_POINT('Ctrl Pts',(-33.7242209861537,-31.8024529385825,
166.));
#33094=CARTESIAN_POINT('Ctrl Pts',(-33.7249995905293,-31.8677854432606,
166.));
#33095=CARTESIAN_POINT('Ctrl Pts',(-33.7221998286388,-31.9328937570084,
166.));
#33096=CARTESIAN_POINT('Ctrl Pts',(-33.7157435098322,-31.9974682783476,
166.));
#33097=CARTESIAN_POINT('Ctrl Pts',(-33.7094097670054,-32.0608168247216,
166.));
#33098=CARTESIAN_POINT('Ctrl Pts',(-33.6995568373319,-32.1236525228668,
166.));
#33099=CARTESIAN_POINT('Ctrl Pts',(-33.6860642400599,-32.1856659078437,
166.));
#33100=CARTESIAN_POINT('Ctrl Pts',(-33.6730092582277,-32.2456679665956,
166.));
#33101=CARTESIAN_POINT('Ctrl Pts',(-33.6565466410315,-32.304900812395,166.));
#33102=CARTESIAN_POINT('Ctrl Pts',(-33.6365261352111,-32.3630572331293,
166.));
#33103=CARTESIAN_POINT('Ctrl Pts',(-33.6332193402308,-32.3726629524795,
166.));
#33104=CARTESIAN_POINT('Ctrl Pts',(-33.6298153922485,-32.3822392325952,
166.));
#33105=CARTESIAN_POINT('Ctrl Pts',(-33.6263135082516,-32.3917845978604,
166.));
#33106=CARTESIAN_POINT('Ctrl Pts',(-33.6225506586299,-32.4020412979991,
166.));
#33107=CARTESIAN_POINT('Ctrl Pts',(-33.6186747312615,-32.4122623041161,
166.));
#33108=CARTESIAN_POINT('Ctrl Pts',(-33.6146867820778,-32.422446252051,166.));
#33109=CARTESIAN_POINT('Origin',(-32.,-32.,180.545925280538));
#33110=CARTESIAN_POINT('Ctrl Pts',(-34.0565967959177,-31.9984978779484,
178.795925280538));
#33111=CARTESIAN_POINT('Ctrl Pts',(-34.0574113092882,-31.9004036992395,
178.790592107115));
#33112=CARTESIAN_POINT('Ctrl Pts',(-34.0064252722628,-31.1217950158479,
178.748215670618));
#33113=CARTESIAN_POINT('Ctrl Pts',(-33.0117514577367,-29.791988463957,178.668795971049));
#33114=CARTESIAN_POINT('Ctrl Pts',(-30.6939036549736,-29.9525600728975,
178.557666181829));
#33115=CARTESIAN_POINT('Ctrl Pts',(-29.5714224639719,-31.9866392256298,
178.446536392609));
#33116=CARTESIAN_POINT('Ctrl Pts',(-30.6715287627672,-34.0330871086906,
178.33540660339));
#33117=CARTESIAN_POINT('Ctrl Pts',(-32.9874475184943,-34.2188064189366,
178.22427681417));
#33118=CARTESIAN_POINT('Ctrl Pts',(-34.0018726081791,-32.893590431192,178.144449706553));
#33119=CARTESIAN_POINT('Ctrl Pts',(-34.0573014417229,-32.1072447535499,
178.101665862009));
#33120=CARTESIAN_POINT('Ctrl Pts',(-34.0563934268478,-32.0016074868405,
178.095925280538));
#33121=CARTESIAN_POINT('Ctrl Pts',(-34.0526600126176,-32.0021813586275,
178.854074719462));
#33122=CARTESIAN_POINT('Ctrl Pts',(-34.0491237063947,-31.5321172985515,
178.828629953495));
#33123=CARTESIAN_POINT('Ctrl Pts',(-33.6567303178001,-30.3707973172003,
178.766141924455));
#33124=CARTESIAN_POINT('Ctrl Pts',(-31.7283973144122,-29.5870608054774,
178.666610632341));
#33125=CARTESIAN_POINT('Ctrl Pts',(-29.8255893685038,-30.9184850177167,
178.555480843121));
#33126=CARTESIAN_POINT('Ctrl Pts',(-29.9119598065434,-33.2405821817579,
178.444351053901));
#33127=CARTESIAN_POINT('Ctrl Pts',(-31.909683998457,-34.4268788699842,178.333221264681));
#33128=CARTESIAN_POINT('Ctrl Pts',(-33.720863198688,-33.5261195206734,178.236462486535));
#33129=CARTESIAN_POINT('Ctrl Pts',(-34.0499397495798,-32.4182643041283,
178.176746971462));
#33130=CARTESIAN_POINT('Ctrl Pts',(-34.0521188940875,-31.9988328896354,
178.154074719462));
#33131=CARTESIAN_POINT('Ctrl Pts',(-30.7309291201476,-30.9206413469516,
179.));
#33132=CARTESIAN_POINT('Ctrl Pts',(-30.3720428517593,-31.3426068457263,
178.962956736927));
#33133=CARTESIAN_POINT('Ctrl Pts',(-30.1149439884831,-32.5658740604652,
178.88887021078));
#33134=CARTESIAN_POINT('Ctrl Pts',(-31.4545463871115,-33.8932420431011,
178.777740421561));
#33135=CARTESIAN_POINT('Ctrl Pts',(-33.2939138023212,-33.4838688004809,
178.666610632341));
#33136=CARTESIAN_POINT('Ctrl Pts',(-33.9488255585344,-31.7184482261547,
178.555480843121));
#33137=CARTESIAN_POINT('Ctrl Pts',(-32.8203323657814,-30.2097348976529,
178.444351053901));
#33138=CARTESIAN_POINT('Ctrl Pts',(-30.9410115533208,-30.3399270380568,
178.333221264682));
#33139=CARTESIAN_POINT('Ctrl Pts',(-30.0308990509683,-31.9891670275699,
178.222091475462));
#33140=CARTESIAN_POINT('Ctrl Pts',(-30.9228698959826,-33.6484356360037,
178.110961686242));
#33141=CARTESIAN_POINT('Ctrl Pts',(-32.8006266289385,-33.7990176391037,
177.999831897022));
#33142=CARTESIAN_POINT('Ctrl Pts',(-33.9456545763016,-32.3031858052012,
177.888702107803));
#33143=CARTESIAN_POINT('Ctrl Pts',(-33.3100425086012,-30.5298680560717,
177.777572318583));
#33144=CARTESIAN_POINT('Ctrl Pts',(-31.4754927844203,-30.1020057762959,
177.666442529363));
#33145=CARTESIAN_POINT('Ctrl Pts',(-30.1209668471194,-31.4111639574702,
177.555312740144));
#33146=CARTESIAN_POINT('Ctrl Pts',(-30.4861114426254,-33.2592201050247,
177.444182950924));
#33147=CARTESIAN_POINT('Ctrl Pts',(-32.2367505420768,-33.9548508793836,
177.333053161704));
#33148=CARTESIAN_POINT('Ctrl Pts',(-33.770718057041,-32.8614237158023,177.221923372484));
#33149=CARTESIAN_POINT('Ctrl Pts',(-33.6841436362607,-30.9796307189992,
177.110793583265));
#33150=CARTESIAN_POINT('Ctrl Pts',(-32.0562592098835,-30.0316687161759,
176.999663794045));
#33151=CARTESIAN_POINT('Ctrl Pts',(-30.3768869713417,-30.8851021127453,
176.888534004825));
#33152=CARTESIAN_POINT('Ctrl Pts',(-30.1829701714511,-32.7588779877096,
176.777404215605));
#33153=CARTESIAN_POINT('Ctrl Pts',(-31.6519793673763,-33.9381369469389,
176.666274426386));
#33154=CARTESIAN_POINT('Ctrl Pts',(-33.4394932713683,-33.3436339959878,
176.555144637166));
#33155=CARTESIAN_POINT('Ctrl Pts',(-33.9095985444435,-31.5194517803416,
176.444014847946));
#33156=CARTESIAN_POINT('Ctrl Pts',(-32.6320599381888,-30.1350620853103,
176.332885058727));
#33157=CARTESIAN_POINT('Ctrl Pts',(-30.7760669310012,-30.457443344749,176.221755269507));
#33158=CARTESIAN_POINT('Ctrl Pts',(-30.0402041955143,-32.1915557270597,
176.110625480287));
#33159=CARTESIAN_POINT('Ctrl Pts',(-31.0979253272145,-33.7503583851451,
175.999495691067));
#33160=CARTESIAN_POINT('Ctrl Pts',(-32.9812154168446,-33.7072520310685,
175.888365901848));
#33161=CARTESIAN_POINT('Ctrl Pts',(-33.966507797822,-32.1016871324977,175.777236112628));
#33162=CARTESIAN_POINT('Ctrl Pts',(-33.1520735681191,-30.4030592730345,
175.666106323408));
#33163=CARTESIAN_POINT('Ctrl Pts',(-31.2832741025925,-30.1659342487801,
175.554976534188));
#33164=CARTESIAN_POINT('Ctrl Pts',(-30.0704144058039,-31.6073263104316,
175.443846744969));
#33165=CARTESIAN_POINT('Ctrl Pts',(-30.6234905193395,-33.4080890744052,
175.332716955749));
#33166=CARTESIAN_POINT('Ctrl Pts',(-32.4363331819517,-33.9201839875743,
175.221587166529));
#33167=CARTESIAN_POINT('Ctrl Pts',(-33.8498484482781,-32.6749473388432,
175.11045737731));
#33168=CARTESIAN_POINT('Ctrl Pts',(-33.5704024755114,-30.8120062051021,
174.99932758809));
#33169=CARTESIAN_POINT('Ctrl Pts',(-31.8537411874624,-30.0363041091952,
174.88819779887));
#33170=CARTESIAN_POINT('Ctrl Pts',(-30.270934378537,-31.0577551971577,174.77706800965));
#33171=CARTESIAN_POINT('Ctrl Pts',(-30.2705496754386,-32.9415385104621,
174.665938220431));
#33172=CARTESIAN_POINT('Ctrl Pts',(-31.8529391542711,-33.9636359895515,
174.554808431211));
#33173=CARTESIAN_POINT('Ctrl Pts',(-33.5699171243061,-33.188635105749,174.443678641991));
#33174=CARTESIAN_POINT('Ctrl Pts',(-33.8501239672185,-31.3258082633759,
174.332548852771));
#33175=CARTESIAN_POINT('Ctrl Pts',(-32.4371174190915,-30.0799943870563,
174.221419063552));
#33176=CARTESIAN_POINT('Ctrl Pts',(-30.6240657493529,-30.5913488261089,
174.110289274332));
#33177=CARTESIAN_POINT('Ctrl Pts',(-30.070254184421,-32.3918855433208,173.999159485112));
#33178=CARTESIAN_POINT('Ctrl Pts',(-31.2825250626851,-33.8337728611072,
173.888029695892));
#33179=CARTESIAN_POINT('Ctrl Pts',(-33.151421222888,-33.5974111428469,173.776899906673));
#33180=CARTESIAN_POINT('Ctrl Pts',(-33.9665491665471,-31.8991160698556,
173.665770117453));
#33181=CARTESIAN_POINT('Ctrl Pts',(-32.98191263932,-30.2931488756918,173.554640328233));
#33182=CARTESIAN_POINT('Ctrl Pts',(-31.0986403129863,-30.2492733204651,
173.443510539014));
#33183=CARTESIAN_POINT('Ctrl Pts',(-30.0402825973689,-31.8076438365085,
173.332380749794));
#33184=CARTESIAN_POINT('Ctrl Pts',(-30.7754369963891,-33.5420566273636,
173.221250960574));
#33185=CARTESIAN_POINT('Ctrl Pts',(-32.6312981764812,-33.8651959157632,
173.110121171355));
#33186=CARTESIAN_POINT('Ctrl Pts',(-33.9094021116014,-32.4813281292638,
172.998991382135));
#33187=CARTESIAN_POINT('Ctrl Pts',(-33.4400419407876,-30.6569540586483,
172.887861592915));
#33188=CARTESIAN_POINT('Ctrl Pts',(-31.6527710023696,-30.0617210688312,
172.776731803695));
#33189=CARTESIAN_POINT('Ctrl Pts',(-30.1832802770412,-31.24037993706,172.665602014476));
#33190=CARTESIAN_POINT('Ctrl Pts',(-30.3764317406597,-33.1142348491549,
172.554472225256));
#33191=CARTESIAN_POINT('Ctrl Pts',(-32.0554552683619,-33.968354110677,172.443342436036));
#33192=CARTESIAN_POINT('Ctrl Pts',(-33.6837267358465,-33.021057036019,172.332212646816));
#33193=CARTESIAN_POINT('Ctrl Pts',(-33.7710697539406,-31.1392996348988,
172.221082857597));
#33194=CARTESIAN_POINT('Ctrl Pts',(-32.2375489396799,-30.0452458740124,
172.109953068377));
#33195=CARTESIAN_POINT('Ctrl Pts',(-30.4866259119352,-30.7401618908041,
171.998823279157));
#33196=CARTESIAN_POINT('Ctrl Pts',(-30.1207264377287,-32.5880680827564,
171.887693489937));
#33197=CARTESIAN_POINT('Ctrl Pts',(-31.4747177478399,-33.8977807427029,
171.776563700718));
#33198=CARTESIAN_POINT('Ctrl Pts',(-33.3094416786791,-33.4706650475028,
171.665433911498));
#33199=CARTESIAN_POINT('Ctrl Pts',(-33.9457787854949,-31.6976126495265,
171.554304122278));
#33200=CARTESIAN_POINT('Ctrl Pts',(-32.8013602489181,-30.2013018754492,
171.443174333058));
#33201=CARTESIAN_POINT('Ctrl Pts',(-30.9235455029214,-30.3511401188919,
171.332044543839));
#33202=CARTESIAN_POINT('Ctrl Pts',(-30.0308902389882,-32.0099970443839,
171.220914754619));
#33203=CARTESIAN_POINT('Ctrl Pts',(-30.9403428742268,-33.6597047832692,
171.109784965399));
#33204=CARTESIAN_POINT('Ctrl Pts',(-32.81958221947,-33.7904687032553,170.99865517618));
#33205=CARTESIAN_POINT('Ctrl Pts',(-33.9487488054533,-32.2826150828469,
170.88752538696));
#33206=CARTESIAN_POINT('Ctrl Pts',(-33.2944416179866,-30.5161152034498,
170.77639559774));
#33207=CARTESIAN_POINT('Ctrl Pts',(-31.4554754993733,-30.107650597795,170.66526580852));
#33208=CARTESIAN_POINT('Ctrl Pts',(-30.1148522986113,-31.4310436433634,
170.554136019301));
#33209=CARTESIAN_POINT('Ctrl Pts',(-30.4994958305847,-33.2751393764509,
170.443006230081));
#33210=CARTESIAN_POINT('Ctrl Pts',(-32.2573845061169,-33.9522413805212,
170.331876440861));
#33211=CARTESIAN_POINT('Ctrl Pts',(-33.7797176728697,-32.8426732443147,
170.220746651642));
#33212=CARTESIAN_POINT('Ctrl Pts',(-33.6732725256466,-30.9618996933222,
170.109616862422));
#33213=CARTESIAN_POINT('Ctrl Pts',(-32.0354665088367,-30.0311842852721,
169.998487073202));
#33214=CARTESIAN_POINT('Ctrl Pts',(-30.3652019277577,-30.9023076684237,
169.887357283982));
#33215=CARTESIAN_POINT('Ctrl Pts',(-30.191086813748,-32.7780271694562,169.776227494763));
#33216=CARTESIAN_POINT('Ctrl Pts',(-31.6724694309494,-33.9417046423557,
169.665097705543));
#33217=CARTESIAN_POINT('Ctrl Pts',(-33.453604473025,-33.3283550834814,169.553967916323));
#33218=CARTESIAN_POINT('Ctrl Pts',(-33.9044164650717,-31.4993093576157,
169.442838127103));
#33219=CARTESIAN_POINT('Ctrl Pts',(-32.6123271608224,-30.1284902778966,
169.331708337884));
#33220=CARTESIAN_POINT('Ctrl Pts',(-30.759842679398,-30.4704566001679,169.220578548664));
#33221=CARTESIAN_POINT('Ctrl Pts',(-30.0423367288465,-32.2122444547597,
169.109448759444));
#33222=CARTESIAN_POINT('Ctrl Pts',(-31.1164629740721,-33.7597884860473,
168.998318970225));
#33223=CARTESIAN_POINT('Ctrl Pts',(-32.9991927238842,-33.6967931790227,
168.887189181005));
#33224=CARTESIAN_POINT('Ctrl Pts',(-33.9674721285561,-32.0809111554984,
168.776059391785));
#33225=CARTESIAN_POINT('Ctrl Pts',(-33.135142377592,-30.3909801199351,168.664929602566));
#33226=CARTESIAN_POINT('Ctrl Pts',(-31.263942632616,-30.1736066294559,168.553799813346));
#33227=CARTESIAN_POINT('Ctrl Pts',(-30.0663746083578,-31.627728545404,168.442670024126));
#33228=CARTESIAN_POINT('Ctrl Pts',(-30.6384395726302,-33.4225492592449,
168.331540234906));
#33229=CARTESIAN_POINT('Ctrl Pts',(-32.4565898757574,-33.9154683184132,
168.220410445686));
#33230=CARTESIAN_POINT('Ctrl Pts',(-33.8568740735902,-32.6553715439732,
168.109280656467));
#33231=CARTESIAN_POINT('Ctrl Pts',(-33.557767261349,-30.7954858417039,167.998150867247));
#33232=CARTESIAN_POINT('Ctrl Pts',(-31.8330087343896,-30.0379584306098,
167.887021078027));
#33233=CARTESIAN_POINT('Ctrl Pts',(-30.2610788239753,-31.0760701946845,
167.775891288807));
#33234=CARTESIAN_POINT('Ctrl Pts',(-30.2805906728734,-32.9597524800475,
167.664761499588));
#33235=CARTESIAN_POINT('Ctrl Pts',(-31.8736873796365,-33.9650797382332,
167.553631710368));
#33236=CARTESIAN_POINT('Ctrl Pts',(-33.5823838477932,-33.1719872601882,
167.442501921148));
#33237=CARTESIAN_POINT('Ctrl Pts',(-33.8429001430549,-31.3063048942249,
167.331372131929));
#33238=CARTESIAN_POINT('Ctrl Pts',(-32.4168134709511,-30.0754844752405,
167.220242342709));
#33239=CARTESIAN_POINT('Ctrl Pts',(-30.6092651408375,-30.6059603865314,
167.109112553489));
#33240=CARTESIAN_POINT('Ctrl Pts',(-30.0744991966179,-32.4122450279571,
166.99798276427));
#33241=CARTESIAN_POINT('Ctrl Pts',(-31.3019369679044,-33.8412499466342,
166.88685297505));
#33242=CARTESIAN_POINT('Ctrl Pts',(-33.1682217075247,-33.5851578807299,
166.77572318583));
#33243=CARTESIAN_POINT('Ctrl Pts',(-33.9653885654801,-31.8783566947692,
166.66459339661));
#33244=CARTESIAN_POINT('Ctrl Pts',(-32.9638002744564,-30.2828614116132,
166.553463607391));
#33245=CARTESIAN_POINT('Ctrl Pts',(-31.0802600234891,-30.2589149518813,
166.442333818171));
#33246=CARTESIAN_POINT('Ctrl Pts',(-30.0382367488593,-31.8283047073915,
166.331204028951));
#33247=CARTESIAN_POINT('Ctrl Pts',(-30.7920439879536,-33.5550031292294,
166.220074239731));
#33248=CARTESIAN_POINT('Ctrl Pts',(-32.6504510705939,-33.8582230624016,
166.108944450512));
#33249=CARTESIAN_POINT('Ctrl Pts',(-33.9154261036092,-32.461549476428,165.997814661292));
#33250=CARTESIAN_POINT('Ctrl Pts',(-33.423606114718,-30.6409579664333,165.886684872072));
#33251=CARTESIAN_POINT('Ctrl Pts',(-32.2331222331378,-30.2598665970074,
165.812598345926));
#33252=CARTESIAN_POINT('Ctrl Pts',(-31.6889203620497,-30.3633004372052,
165.775555082853));
#33253=CARTESIAN_POINT('Ctrl Pts',(-30.6322193753411,-30.8366876301903,
179.074814972382));
#33254=CARTESIAN_POINT('Ctrl Pts',(-30.2454185337564,-31.2914740748732,
179.037771709309));
#33255=CARTESIAN_POINT('Ctrl Pts',(-29.9683222348862,-32.6098883743919,
178.963685183163));
#33256=CARTESIAN_POINT('Ctrl Pts',(-31.4121203983139,-34.0405005153411,
178.852555393943));
#33257=CARTESIAN_POINT('Ctrl Pts',(-33.3945558572736,-33.5992857665047,
178.741425604723));
#33258=CARTESIAN_POINT('Ctrl Pts',(-34.1004073784384,-31.6965488159742,
178.630295815504));
#33259=CARTESIAN_POINT('Ctrl Pts',(-32.8841387297665,-30.0704860864209,
178.519166026284));
#33260=CARTESIAN_POINT('Ctrl Pts',(-30.8586422538717,-30.2108047163371,
178.408036237064));
#33261=CARTESIAN_POINT('Ctrl Pts',(-29.8777401886362,-31.9883244269232,
178.296906447844));
#33262=CARTESIAN_POINT('Ctrl Pts',(-30.8390895182441,-33.776652793566,178.185776658625));
#33263=CARTESIAN_POINT('Ctrl Pts',(-32.8629002587904,-33.9389472323813,
178.074646869405));
#33264=CARTESIAN_POINT('Ctrl Pts',(-34.09698975368,-32.3267679344073,177.963517080185));
#33265=CARTESIAN_POINT('Ctrl Pts',(-33.4119390722704,-30.415519558032,177.852387290965));
#33266=CARTESIAN_POINT('Ctrl Pts',(-31.4346960297071,-29.954377674162,177.741257501746));
#33267=CARTESIAN_POINT('Ctrl Pts',(-29.9748135581674,-31.3653636350345,
177.630127712526));
#33268=CARTESIAN_POINT('Ctrl Pts',(-30.3683595065151,-33.3571636456066,
177.518997923306));
#33269=CARTESIAN_POINT('Ctrl Pts',(-32.2551652626115,-34.1069013554461,
177.407868134087));
#33270=CARTESIAN_POINT('Ctrl Pts',(-33.9084464773441,-32.9284262107039,
177.296738344867));
#33271=CARTESIAN_POINT('Ctrl Pts',(-33.8151382018061,-30.9002652612182,
177.185608555647));
#33272=CARTESIAN_POINT('Ctrl Pts',(-32.0606351138136,-29.8785697192598,
177.074478766427));
#33273=CARTESIAN_POINT('Ctrl Pts',(-30.2506394343487,-30.7983841148121,
176.963348977208));
#33274=CARTESIAN_POINT('Ctrl Pts',(-30.0416395700409,-32.8179043618037,
176.852219187988));
#33275=CARTESIAN_POINT('Ctrl Pts',(-31.624909935417,-34.0888873947425,176.741089398768));
#33276=CARTESIAN_POINT('Ctrl Pts',(-33.5514586593724,-33.4481433429146,
176.629959609548));
#33277=CARTESIAN_POINT('Ctrl Pts',(-34.0581292435536,-31.4820742052332,
176.518829820329));
#33278=CARTESIAN_POINT('Ctrl Pts',(-32.681222263313,-29.9900051396649,176.407700031109));
#33279=CARTESIAN_POINT('Ctrl Pts',(-30.6808680553363,-30.3374615720942,
176.296570241889));
#33280=CARTESIAN_POINT('Ctrl Pts',(-29.8877690976764,-32.2064551446055,
176.18544045267));
#33281=CARTESIAN_POINT('Ctrl Pts',(-31.0277609556569,-33.8865032075191,
176.07431066345));
#33282=CARTESIAN_POINT('Ctrl Pts',(-33.0575354435149,-33.8400439932689,
175.96318087423));
#33283=CARTESIAN_POINT('Ctrl Pts',(-34.1194649619683,-32.1095964707848,
175.85205108501));
#33284=CARTESIAN_POINT('Ctrl Pts',(-33.2416831318658,-30.2788474467825,
175.740921295791));
#33285=CARTESIAN_POINT('Ctrl Pts',(-31.227526364974,-30.0232785743529,175.629791506571));
#33286=CARTESIAN_POINT('Ctrl Pts',(-29.9203290917295,-31.5767837140291,
175.518661717351));
#33287=CARTESIAN_POINT('Ctrl Pts',(-30.5164240806426,-33.517611809034,175.407531928132));
#33288=CARTESIAN_POINT('Ctrl Pts',(-32.4702716622405,-34.0695380342269,
175.296402138912));
#33289=CARTESIAN_POINT('Ctrl Pts',(-33.9937317184398,-32.7274454937002,
175.185272349692));
#33290=CARTESIAN_POINT('Ctrl Pts',(-33.692550127043,-30.7196027261572,175.074142560472));
#33291=CARTESIAN_POINT('Ctrl Pts',(-31.8423650143184,-29.8835656583048,
174.963012771252));
#33292=CARTESIAN_POINT('Ctrl Pts',(-30.1364457310092,-30.9844663481972,
174.851882982033));
#33293=CARTESIAN_POINT('Ctrl Pts',(-30.136031105276,-33.0147724232156,174.740753192813));
#33294=CARTESIAN_POINT('Ctrl Pts',(-31.8415005980932,-34.1163697812558,
174.629623403593));
#33295=CARTESIAN_POINT('Ctrl Pts',(-33.692027024681,-33.2810884665653,174.518493614374));
#33296=CARTESIAN_POINT('Ctrl Pts',(-33.9940286675499,-31.2733688801001,
174.407363825154));
#33297=CARTESIAN_POINT('Ctrl Pts',(-32.4711168982175,-29.930654214581,174.296234035934));
#33298=CARTESIAN_POINT('Ctrl Pts',(-30.5170440526865,-30.4817823707567,
174.185104246715));
#33299=CARTESIAN_POINT('Ctrl Pts',(-29.9201564081492,-32.4223668368314,
174.073974457495));
#33300=CARTESIAN_POINT('Ctrl Pts',(-31.2267190639093,-33.9764057542155,
173.962844668275));
#33301=CARTESIAN_POINT('Ctrl Pts',(-33.240980046497,-33.7216595585696,173.851714879055));
#33302=CARTESIAN_POINT('Ctrl Pts',(-34.1195095483989,-31.8912692055412,
173.740585089835));
#33303=CARTESIAN_POINT('Ctrl Pts',(-33.05828689673,-30.1603880964652,173.629455300616));
#33304=CARTESIAN_POINT('Ctrl Pts',(-31.0285315538174,-30.1130998517438,
173.518325511396));
#33305=CARTESIAN_POINT('Ctrl Pts',(-29.8878535977144,-31.7926821601266,
173.407195722177));
#33306=CARTESIAN_POINT('Ctrl Pts',(-30.6801891237093,-33.661999507293,173.296065932957));
#33307=CARTESIAN_POINT('Ctrl Pts',(-32.6804012509324,-34.0102729290192,
173.184936143737));
#33308=CARTESIAN_POINT('Ctrl Pts',(-34.0579175319466,-32.518766366609,173.073806354517));
#33309=CARTESIAN_POINT('Ctrl Pts',(-33.5520500049095,-30.5524904512653,
172.962676565297));
#33310=CARTESIAN_POINT('Ctrl Pts',(-31.6257631446607,-29.9109595773362,
172.851546776078));
#33311=CARTESIAN_POINT('Ctrl Pts',(-30.0419737959887,-31.181295843529,172.740416986858));
#33312=CARTESIAN_POINT('Ctrl Pts',(-30.2501487953179,-33.2009012752471,
172.629287197638));
#33313=CARTESIAN_POINT('Ctrl Pts',(-32.059768640826,-34.1214548830912,172.518157408419));
#33314=CARTESIAN_POINT('Ctrl Pts',(-33.814688874414,-33.1004759881503,172.407027619199));
#33315=CARTESIAN_POINT('Ctrl Pts',(-33.9088255296197,-31.0723534030195,
172.295897829979));
#33316=CARTESIAN_POINT('Ctrl Pts',(-32.2560257604683,-29.8932029235367,
172.184768040759));
#33317=CARTESIAN_POINT('Ctrl Pts',(-30.3689139918201,-30.6421702811702,
172.07363825154));
#33318=CARTESIAN_POINT('Ctrl Pts',(-29.9745544494668,-32.6338086724266,
171.96250846232));
#33319=CARTESIAN_POINT('Ctrl Pts',(-31.4338607099192,-34.045392240047,171.8513786731));
#33320=CARTESIAN_POINT('Ctrl Pts',(-33.4112915091286,-33.5850550109315,
171.74024888388));
#33321=CARTESIAN_POINT('Ctrl Pts',(-34.0971236240025,-31.6740926250174,
171.629119094661));
#33322=CARTESIAN_POINT('Ctrl Pts',(-32.8636909405481,-30.0613971343689,
171.517989305441));
#33323=CARTESIAN_POINT('Ctrl Pts',(-30.8398176746423,-30.2228899630735,
171.406859516221));
#33324=CARTESIAN_POINT('Ctrl Pts',(-29.8777306912504,-32.0107746256172,
171.295729727001));
#33325=CARTESIAN_POINT('Ctrl Pts',(-30.8579215641739,-33.7887984676421,
171.184599937782));
#33326=CARTESIAN_POINT('Ctrl Pts',(-32.8833302362405,-33.9297333507925,
171.073470148562));
#33327=CARTESIAN_POINT('Ctrl Pts',(-34.1003246554173,-32.3045971983844,
170.962340359343));
#33328=CARTESIAN_POINT('Ctrl Pts',(-33.3951247270286,-30.4006969932339,
170.851210570123));
#33329=CARTESIAN_POINT('Ctrl Pts',(-31.413121777961,-29.9604615561569,170.740080780903));
#33330=CARTESIAN_POINT('Ctrl Pts',(-29.9682234132741,-31.3867895850116,
170.628950991683));
#33331=CARTESIAN_POINT('Ctrl Pts',(-30.3827849470592,-33.3743211356737,
170.517821202464));
#33332=CARTESIAN_POINT('Ctrl Pts',(-32.2774041593287,-34.1040888868593,
170.406691413244));
#33333=CARTESIAN_POINT('Ctrl Pts',(-33.9181460933034,-32.9082173066851,
170.295561624024));
#33334=CARTESIAN_POINT('Ctrl Pts',(-33.803421524115,-30.8811550966393,170.184431834804));
#33335=CARTESIAN_POINT('Ctrl Pts',(-32.0382251333486,-29.8780476087814,
170.073302045585));
#33336=CARTESIAN_POINT('Ctrl Pts',(-30.2380455150758,-30.8169279377514,
169.962172256365));
#33337=CARTESIAN_POINT('Ctrl Pts',(-30.050387533805,-32.838542988209,169.851042467145));
#33338=CARTESIAN_POINT('Ctrl Pts',(-31.6469937389289,-34.0927325894777,
169.739912677925));
#33339=CARTESIAN_POINT('Ctrl Pts',(-33.5666674459918,-33.4316760195965,
169.628782888706));
#33340=CARTESIAN_POINT('Ctrl Pts',(-34.0525440962835,-31.4603650824602,
169.517653099486));
#33341=CARTESIAN_POINT('Ctrl Pts',(-32.6599546485714,-29.9829221697599,
169.406523310266));
#33342=CARTESIAN_POINT('Ctrl Pts',(-30.6633818633947,-30.3514870129961,
169.295393521047));
#33343=CARTESIAN_POINT('Ctrl Pts',(-29.8900675018235,-32.2287530645612,
169.184263731827));
#33344=CARTESIAN_POINT('Ctrl Pts',(-31.0477404813091,-33.89666679216,169.073133942607));
#33345=CARTESIAN_POINT('Ctrl Pts',(-33.0769110454948,-33.8287716400761,
168.962004153387));
#33346=CARTESIAN_POINT('Ctrl Pts',(-34.1205042994196,-32.0872045151823,
168.850874364168));
#33347=CARTESIAN_POINT('Ctrl Pts',(-33.2234350145046,-30.2658287637176,
168.739744574948));
#33348=CARTESIAN_POINT('Ctrl Pts',(-31.2066912717576,-30.0315477213328,
168.628614785728));
#33349=CARTESIAN_POINT('Ctrl Pts',(-29.915975074344,-31.598772857534,168.517484996508));
#33350=CARTESIAN_POINT('Ctrl Pts',(-30.5325358879284,-33.5331967231367,
168.406355207289));
#33351=CARTESIAN_POINT('Ctrl Pts',(-32.4921039442249,-34.0644555750725,
168.295225418069));
#33352=CARTESIAN_POINT('Ctrl Pts',(-34.0013038047043,-32.7063470717282,
168.184095628849));
#33353=CARTESIAN_POINT('Ctrl Pts',(-33.6789321318671,-30.7017973905159,
168.07296583963));
#33354=CARTESIAN_POINT('Ctrl Pts',(-31.8200199679818,-29.8853486546794,
167.96183605041));
#33355=CARTESIAN_POINT('Ctrl Pts',(-30.12582360045,-31.0042059066059,167.85070626119));
#33356=CARTESIAN_POINT('Ctrl Pts',(-30.1468531026612,-33.0344030956174,
167.73957647197));
#33357=CARTESIAN_POINT('Ctrl Pts',(-31.8638626435088,-34.1179258263161,
167.628446682751));
#33358=CARTESIAN_POINT('Ctrl Pts',(-33.7054634237896,-33.263145733057,167.517316893531));
#33359=CARTESIAN_POINT('Ctrl Pts',(-33.9862429663067,-31.2523485172001,
167.406187104311));
#33360=CARTESIAN_POINT('Ctrl Pts',(-32.4492336864037,-29.9257935168071,
167.295057315092));
#33361=CARTESIAN_POINT('Ctrl Pts',(-30.5010922363758,-30.4975304346034,
167.183927525872));
#33362=CARTESIAN_POINT('Ctrl Pts',(-29.9247316021171,-32.4443099048315,
167.072797736652));
#33363=CARTESIAN_POINT('Ctrl Pts',(-31.2476408487112,-33.9844644157726,
166.961667947432));
#33364=CARTESIAN_POINT('Ctrl Pts',(-33.2590872915183,-33.7084532240939,
166.850538158213));
#33365=CARTESIAN_POINT('Ctrl Pts',(-34.1182586744898,-31.8688951431669,
166.739408368993));
#33366=CARTESIAN_POINT('Ctrl Pts',(-33.0387657319783,-30.1493004619863,
166.628278579773));
#33367=CARTESIAN_POINT('Ctrl Pts',(-31.008721624956,-30.1234914199773,166.517148790553));
#33368=CARTESIAN_POINT('Ctrl Pts',(-29.8856486208318,-31.8149500565308,
166.406019001334));
#33369=CARTESIAN_POINT('Ctrl Pts',(-30.698087825552,-33.6759530024763,166.294889212114));
#33370=CARTESIAN_POINT('Ctrl Pts',(-32.7010438784557,-34.0027577193661,
166.183759422894));
#33371=CARTESIAN_POINT('Ctrl Pts',(-34.0644100767541,-32.4974493081529,
166.072629633674));
#33372=CARTESIAN_POINT('Ctrl Pts',(-33.5343357820042,-30.535250165203,165.961499844455));
#33373=CARTESIAN_POINT('Ctrl Pts',(-32.2512547397669,-30.12451708512,165.887413318308));
#33374=CARTESIAN_POINT('Ctrl Pts',(-31.664724241751,-30.2359961244728,165.850370055235));
#33375=CARTESIAN_POINT('Ctrl Pts',(-30.5335096305347,-30.7527339134291,
179.149629944765));
#33376=CARTESIAN_POINT('Ctrl Pts',(-30.1187942157535,-31.24034130402,179.112586681692));
#33377=CARTESIAN_POINT('Ctrl Pts',(-29.8217004812893,-32.6539026883187,
179.038500155545));
#33378=CARTESIAN_POINT('Ctrl Pts',(-31.3696944095162,-34.187758987581,178.927370366326));
#33379=CARTESIAN_POINT('Ctrl Pts',(-33.4951979122261,-33.7147027325285,
178.816240577106));
#33380=CARTESIAN_POINT('Ctrl Pts',(-34.2519891983425,-31.6746494057936,
178.705110787886));
#33381=CARTESIAN_POINT('Ctrl Pts',(-32.9479450937516,-29.9312372751889,
178.593980998666));
#33382=CARTESIAN_POINT('Ctrl Pts',(-30.7762729544227,-30.0816823946173,
178.482851209447));
#33383=CARTESIAN_POINT('Ctrl Pts',(-29.724581326304,-31.9874818262765,178.371721420227));
#33384=CARTESIAN_POINT('Ctrl Pts',(-30.7553091405056,-33.9048699511283,
178.260591631007));
#33385=CARTESIAN_POINT('Ctrl Pts',(-32.9251738886423,-34.078876825659,178.149461841787));
#33386=CARTESIAN_POINT('Ctrl Pts',(-34.2483249310584,-32.3503500636134,
178.038332052568));
#33387=CARTESIAN_POINT('Ctrl Pts',(-33.5138356359396,-30.3011710599924,
177.927202263348));
#33388=CARTESIAN_POINT('Ctrl Pts',(-31.3938992749938,-29.8067495720281,
177.816072474128));
#33389=CARTESIAN_POINT('Ctrl Pts',(-29.8286602692153,-31.3195633125989,
177.704942684908));
#33390=CARTESIAN_POINT('Ctrl Pts',(-30.2506075704047,-33.4551071861885,
177.593812895689));
#33391=CARTESIAN_POINT('Ctrl Pts',(-32.2735799831462,-34.2589518315086,
177.482683106469));
#33392=CARTESIAN_POINT('Ctrl Pts',(-34.0461748976471,-32.9954287056055,
177.371553317249));
#33393=CARTESIAN_POINT('Ctrl Pts',(-33.9461327673516,-30.8208998034373,
177.26042352803));
#33394=CARTESIAN_POINT('Ctrl Pts',(-32.0650110177436,-29.7254707223437,
177.14929373881));
#33395=CARTESIAN_POINT('Ctrl Pts',(-30.1243918973557,-30.7116661168789,
177.03816394959));
#33396=CARTESIAN_POINT('Ctrl Pts',(-29.9003089686307,-32.8769307358977,
176.92703416037));
#33397=CARTESIAN_POINT('Ctrl Pts',(-31.5978405034577,-34.2396378425461,
176.815904371151));
#33398=CARTESIAN_POINT('Ctrl Pts',(-33.6634240473765,-33.5526526898415,
176.704774581931));
#33399=CARTESIAN_POINT('Ctrl Pts',(-34.2066599426637,-31.4446966301247,
176.593644792711));
#33400=CARTESIAN_POINT('Ctrl Pts',(-32.7303845884373,-29.8449481940195,
176.482515003492));
#33401=CARTESIAN_POINT('Ctrl Pts',(-30.5856691796714,-30.2174797994394,
176.371385214272));
#33402=CARTESIAN_POINT('Ctrl Pts',(-29.7353339998384,-32.2213545621514,
176.260255425052));
#33403=CARTESIAN_POINT('Ctrl Pts',(-30.9575965840992,-34.0226480298931,
176.149125635832));
#33404=CARTESIAN_POINT('Ctrl Pts',(-33.1338554701853,-33.9728359554694,
176.037995846613));
#33405=CARTESIAN_POINT('Ctrl Pts',(-34.2724221261146,-32.1175058090718,
175.926866057393));
#33406=CARTESIAN_POINT('Ctrl Pts',(-33.3312926956126,-30.1546356205304,
175.815736268173));
#33407=CARTESIAN_POINT('Ctrl Pts',(-31.1717786273556,-29.8806228999258,
175.704606478953));
#33408=CARTESIAN_POINT('Ctrl Pts',(-29.7702437776551,-31.5462411176266,
175.593476689734));
#33409=CARTESIAN_POINT('Ctrl Pts',(-30.4093576419459,-33.6271345436629,
175.482346900514));
#33410=CARTESIAN_POINT('Ctrl Pts',(-32.5042101425294,-34.2188920808795,
175.371217111294));
#33411=CARTESIAN_POINT('Ctrl Pts',(-34.1376149886015,-32.7799436485572,
175.260087322074));
#33412=CARTESIAN_POINT('Ctrl Pts',(-33.8146977785746,-30.6271992472123,
175.148957532855));
#33413=CARTESIAN_POINT('Ctrl Pts',(-31.8309888411744,-29.7308272074143,
175.037827743635));
#33414=CARTESIAN_POINT('Ctrl Pts',(-30.0019570834814,-30.9111774992366,
174.926697954415));
#33415=CARTESIAN_POINT('Ctrl Pts',(-30.0015125351133,-33.0880063359691,
174.815568165196));
#33416=CARTESIAN_POINT('Ctrl Pts',(-31.8300620419152,-34.2691035729601,
174.704438375976));
#33417=CARTESIAN_POINT('Ctrl Pts',(-33.814136925056,-33.3735418273816,174.593308586756));
#33418=CARTESIAN_POINT('Ctrl Pts',(-34.1379333678812,-31.2209294968243,
174.482178797536));
#33419=CARTESIAN_POINT('Ctrl Pts',(-32.5051163773435,-29.7813140421056,
174.371049008317));
#33420=CARTESIAN_POINT('Ctrl Pts',(-30.41002235602,-30.3722159154045,174.259919219097));
#33421=CARTESIAN_POINT('Ctrl Pts',(-29.7700586318775,-32.452848130342,174.148789429877));
#33422=CARTESIAN_POINT('Ctrl Pts',(-31.1709130651335,-34.1190386473239,
174.037659640657));
#33423=CARTESIAN_POINT('Ctrl Pts',(-33.330538870106,-33.8459079742922,173.926529851438));
#33424=CARTESIAN_POINT('Ctrl Pts',(-34.2724699302506,-31.8834223412267,
173.815400062218));
#33425=CARTESIAN_POINT('Ctrl Pts',(-33.1346611541401,-30.0276273172385,
173.704270272998));
#33426=CARTESIAN_POINT('Ctrl Pts',(-30.9584227946484,-29.9769263830225,
173.593140483779));
#33427=CARTESIAN_POINT('Ctrl Pts',(-29.73542459806,-31.7777204837445,173.482010694559));
#33428=CARTESIAN_POINT('Ctrl Pts',(-30.5849412510295,-33.7819423872226,
173.370880905339));
#33429=CARTESIAN_POINT('Ctrl Pts',(-32.7295043253836,-34.155349942275,173.259751116119));
#33430=CARTESIAN_POINT('Ctrl Pts',(-34.2064329522917,-32.5562046039542,
173.1486213269));
#33431=CARTESIAN_POINT('Ctrl Pts',(-33.6640580690314,-30.4480268438822,
173.03749153768));
#33432=CARTESIAN_POINT('Ctrl Pts',(-31.5987552869518,-29.7601980858412,
172.92636174846));
#33433=CARTESIAN_POINT('Ctrl Pts',(-29.9006673149363,-31.122211749998,172.815231959241));
#33434=CARTESIAN_POINT('Ctrl Pts',(-30.123865849976,-33.2875677013394,172.704102170021));
#33435=CARTESIAN_POINT('Ctrl Pts',(-32.0640820132901,-34.2745556555053,
172.592972380801));
#33436=CARTESIAN_POINT('Ctrl Pts',(-33.9456510129815,-33.1798949402817,
172.481842591581));
#33437=CARTESIAN_POINT('Ctrl Pts',(-34.0465813052989,-31.0054071711401,
172.370712802362));
#33438=CARTESIAN_POINT('Ctrl Pts',(-32.2745025812568,-29.741159973061,172.259583013142));
#33439=CARTESIAN_POINT('Ctrl Pts',(-30.251202071705,-30.5441786715364,172.148453223922));
#33440=CARTESIAN_POINT('Ctrl Pts',(-29.828382461205,-32.6795492620968,172.037323434702));
#33441=CARTESIAN_POINT('Ctrl Pts',(-31.3930036719987,-34.1930037373911,
171.926193645483));
#33442=CARTESIAN_POINT('Ctrl Pts',(-33.513141339578,-33.6994449743603,171.815063856263));
#33443=CARTESIAN_POINT('Ctrl Pts',(-34.2484684625102,-31.6505726005082,
171.703934067043));
#33444=CARTESIAN_POINT('Ctrl Pts',(-32.9260216321781,-29.9214923932887,
171.592804277823));
#33445=CARTESIAN_POINT('Ctrl Pts',(-30.7560898463631,-30.0946398072549,
171.481674488604));
#33446=CARTESIAN_POINT('Ctrl Pts',(-29.7245711435126,-32.0115522068506,
171.370544699384));
#33447=CARTESIAN_POINT('Ctrl Pts',(-30.775500254121,-33.917892152015,171.259414910165));
#33448=CARTESIAN_POINT('Ctrl Pts',(-32.947078253011,-34.0689979983296,171.148285120944));
#33449=CARTESIAN_POINT('Ctrl Pts',(-34.2519005053813,-32.326579313922,171.037155331725));
#33450=CARTESIAN_POINT('Ctrl Pts',(-33.4958078360707,-30.2852787830181,
170.926025542505));
#33451=CARTESIAN_POINT('Ctrl Pts',(-31.3707680565487,-29.8132725145188,
170.814895753286));
#33452=CARTESIAN_POINT('Ctrl Pts',(-29.821594527937,-31.3425355266598,170.703765964066));
#33453=CARTESIAN_POINT('Ctrl Pts',(-30.2660740635338,-33.4735028948964,
170.592636174846));
#33454=CARTESIAN_POINT('Ctrl Pts',(-32.2974238125406,-34.2559363931974,
170.481506385626));
#33455=CARTESIAN_POINT('Ctrl Pts',(-34.0565745137372,-32.9737613690555,
170.370376596407));
#33456=CARTESIAN_POINT('Ctrl Pts',(-33.9335705225834,-30.8004104999564,
170.259246807187));
#33457=CARTESIAN_POINT('Ctrl Pts',(-32.0409837578605,-29.7249109322907,
170.148117017967));
#33458=CARTESIAN_POINT('Ctrl Pts',(-30.1108891023939,-30.731548207079,170.036987228747));
#33459=CARTESIAN_POINT('Ctrl Pts',(-29.9096882538619,-32.8990588069617,
169.925857439528));
#33460=CARTESIAN_POINT('Ctrl Pts',(-31.6215180469084,-34.2437605365997,
169.814727650308));
#33461=CARTESIAN_POINT('Ctrl Pts',(-33.6797304189587,-33.5349969557116,
169.703597861088));
#33462=CARTESIAN_POINT('Ctrl Pts',(-34.2006717274953,-31.4214208073048,
169.592468071868));
#33463=CARTESIAN_POINT('Ctrl Pts',(-32.7075821363205,-29.837354061623,169.481338282649));
#33464=CARTESIAN_POINT('Ctrl Pts',(-30.5669210473915,-30.2325174258244,
169.370208493429));
#33465=CARTESIAN_POINT('Ctrl Pts',(-29.7377982748005,-32.2452616743627,
169.259078704209));
#33466=CARTESIAN_POINT('Ctrl Pts',(-30.9790179885462,-34.0335450982727,
169.14794891499));
#33467=CARTESIAN_POINT('Ctrl Pts',(-33.1546293671055,-33.9607501011295,
169.03681912577));
#33468=CARTESIAN_POINT('Ctrl Pts',(-34.2735364702832,-32.0934978748662,
168.92568933655));
#33469=CARTESIAN_POINT('Ctrl Pts',(-33.3117276514171,-30.1406774075,168.81455954733));
#33470=CARTESIAN_POINT('Ctrl Pts',(-31.1494399108992,-29.8894888132097,
168.703429758111));
#33471=CARTESIAN_POINT('Ctrl Pts',(-29.7655755403302,-31.569817169664,168.592299968891));
#33472=CARTESIAN_POINT('Ctrl Pts',(-30.4266322032265,-33.6438441870286,
168.481170179671));
#33473=CARTESIAN_POINT('Ctrl Pts',(-32.5276180126925,-34.2134428317317,
168.370040390452));
#33474=CARTESIAN_POINT('Ctrl Pts',(-34.1457335358184,-32.7573225994832,
168.258910601232));
#33475=CARTESIAN_POINT('Ctrl Pts',(-33.8000970023852,-30.6081089393279,
168.147780812012));
#33476=CARTESIAN_POINT('Ctrl Pts',(-31.807031201574,-29.7327388787489,168.036651022792));
#33477=CARTESIAN_POINT('Ctrl Pts',(-29.9905683769247,-30.9323416185274,
167.925521233573));
#33478=CARTESIAN_POINT('Ctrl Pts',(-30.013115532449,-33.1090537111873,167.814391444353));
#33479=CARTESIAN_POINT('Ctrl Pts',(-31.8540379073811,-34.2707719143989,
167.703261655133));
#33480=CARTESIAN_POINT('Ctrl Pts',(-33.8285429997859,-33.3543042059258,
167.592131865913));
#33481=CARTESIAN_POINT('Ctrl Pts',(-34.1295857895586,-31.1983921401753,
167.481002076694));
#33482=CARTESIAN_POINT('Ctrl Pts',(-32.4816539018563,-29.7761025583737,
167.369872287474));
#33483=CARTESIAN_POINT('Ctrl Pts',(-30.3929193319141,-30.3891004826755,
167.258742498254));
#33484=CARTESIAN_POINT('Ctrl Pts',(-29.7749640076164,-32.4763747817059,
167.147612709034));
#33485=CARTESIAN_POINT('Ctrl Pts',(-31.1933447295181,-34.1276788849111,
167.036482919815));
#33486=CARTESIAN_POINT('Ctrl Pts',(-33.349952875512,-33.8317485674581,166.925353130595));
#33487=CARTESIAN_POINT('Ctrl Pts',(-34.2711287834995,-31.8594335915646,
166.814223341375));
#33488=CARTESIAN_POINT('Ctrl Pts',(-33.1137311895003,-30.0157395123594,
166.703093552156));
#33489=CARTESIAN_POINT('Ctrl Pts',(-30.9371832264228,-29.9880678880733,
166.591963762936));
#33490=CARTESIAN_POINT('Ctrl Pts',(-29.7330604928044,-31.8015954056701,
166.480833973716));
#33491=CARTESIAN_POINT('Ctrl Pts',(-30.6041316631504,-33.7969028757232,
166.369704184496));
#33492=CARTESIAN_POINT('Ctrl Pts',(-32.7516366863175,-34.1472923763307,
166.258574395277));
#33493=CARTESIAN_POINT('Ctrl Pts',(-34.213394049899,-32.5333491398779,166.147444606057));
#33494=CARTESIAN_POINT('Ctrl Pts',(-33.6450654492904,-30.4295423639727,
166.036314816837));
#33495=CARTESIAN_POINT('Ctrl Pts',(-32.2693872463961,-29.9891675732325,
165.962228290691));
#33496=CARTESIAN_POINT('Ctrl Pts',(-31.6405281214523,-30.1086918117404,
165.925185027618));
#33497=CARTESIAN_POINT('Ctrl Pts',(-30.4347998857282,-30.6687801966679,
179.224444917147));
#33498=CARTESIAN_POINT('Ctrl Pts',(-29.9921698977506,-31.1892085331669,
179.187401654074));
#33499=CARTESIAN_POINT('Ctrl Pts',(-29.6750787276925,-32.6979170022453,
179.113315127928));
#33500=CARTESIAN_POINT('Ctrl Pts',(-31.3272684207187,-34.3350174598211,
179.002185338708));
#33501=CARTESIAN_POINT('Ctrl Pts',(-33.5958399671785,-33.8301196985523,
178.891055549488));
#33502=CARTESIAN_POINT('Ctrl Pts',(-34.4035710182465,-31.6527499956131,
178.779925760269));
#33503=CARTESIAN_POINT('Ctrl Pts',(-33.0117514577367,-29.791988463957,178.668795971049));
#33504=CARTESIAN_POINT('Ctrl Pts',(-30.6939036549736,-29.9525600728975,
178.557666181829));
#33505=CARTESIAN_POINT('Ctrl Pts',(-29.5714224639719,-31.9866392256298,
178.446536392609));
#33506=CARTESIAN_POINT('Ctrl Pts',(-30.6715287627672,-34.0330871086906,
178.33540660339));
#33507=CARTESIAN_POINT('Ctrl Pts',(-32.9874475184943,-34.2188064189366,
178.22427681417));
#33508=CARTESIAN_POINT('Ctrl Pts',(-34.3996601084368,-32.3739321928194,
178.11314702495));
#33509=CARTESIAN_POINT('Ctrl Pts',(-33.6157321996089,-30.1868225619527,
178.002017235731));
#33510=CARTESIAN_POINT('Ctrl Pts',(-31.3531025202806,-29.6591214698943,
177.890887446511));
#33511=CARTESIAN_POINT('Ctrl Pts',(-29.6825069802633,-31.2737629901632,
177.779757657291));
#33512=CARTESIAN_POINT('Ctrl Pts',(-30.1328556342944,-33.5530507267704,
177.668627868071));
#33513=CARTESIAN_POINT('Ctrl Pts',(-32.2919947036809,-34.4110023075711,
177.557498078851));
#33514=CARTESIAN_POINT('Ctrl Pts',(-34.1839033179502,-33.062431200507,177.446368289632));
#33515=CARTESIAN_POINT('Ctrl Pts',(-34.0771273328971,-30.7415343456564,
177.335238500412));
#33516=CARTESIAN_POINT('Ctrl Pts',(-32.0693869216736,-29.5723717254276,
177.224108711192));
#33517=CARTESIAN_POINT('Ctrl Pts',(-29.9981443603627,-30.6249481189457,
177.112978921973));
#33518=CARTESIAN_POINT('Ctrl Pts',(-29.7589783672204,-32.9359571099918,
177.001849132753));
#33519=CARTESIAN_POINT('Ctrl Pts',(-31.5707710714985,-34.3903882903498,
176.890719343533));
#33520=CARTESIAN_POINT('Ctrl Pts',(-33.7753894353805,-33.6571620367683,
176.779589554314));
#33521=CARTESIAN_POINT('Ctrl Pts',(-34.3551906417739,-31.4073190550162,
176.668459765094));
#33522=CARTESIAN_POINT('Ctrl Pts',(-32.7795469135615,-29.6998912483741,
176.557329975874));
#33523=CARTESIAN_POINT('Ctrl Pts',(-30.4904703040065,-30.0974980267845,
176.446200186654));
#33524=CARTESIAN_POINT('Ctrl Pts',(-29.5828989020006,-32.2362539796973,
176.335070397435));
#33525=CARTESIAN_POINT('Ctrl Pts',(-30.8874322125415,-34.1587928522671,
176.223940608215));
#33526=CARTESIAN_POINT('Ctrl Pts',(-33.2101754968556,-34.1056279176698,
176.112810818995));
#33527=CARTESIAN_POINT('Ctrl Pts',(-34.4253792902609,-32.1254151473588,
176.001681029775));
#33528=CARTESIAN_POINT('Ctrl Pts',(-33.4209022593593,-30.0304237942783,
175.890551240556));
#33529=CARTESIAN_POINT('Ctrl Pts',(-31.116030889737,-29.7379672254987,175.779421451336));
#33530=CARTESIAN_POINT('Ctrl Pts',(-29.6201584635808,-31.5156985212241,
175.668291662116));
#33531=CARTESIAN_POINT('Ctrl Pts',(-30.302291203249,-33.7366572782917,175.557161872896));
#33532=CARTESIAN_POINT('Ctrl Pts',(-32.5381486228183,-34.368246127532,175.446032083677));
#33533=CARTESIAN_POINT('Ctrl Pts',(-34.2814982587632,-32.8324418034142,
175.334902294457));
#33534=CARTESIAN_POINT('Ctrl Pts',(-33.9368454301063,-30.5347957682674,
175.223772505237));
#33535=CARTESIAN_POINT('Ctrl Pts',(-31.8196126680302,-29.5780887565239,
175.112642716018));
#33536=CARTESIAN_POINT('Ctrl Pts',(-29.8674684359538,-30.837888650276,175.001512926798));
#33537=CARTESIAN_POINT('Ctrl Pts',(-29.8669939649505,-33.1612402487227,
174.890383137578));
#33538=CARTESIAN_POINT('Ctrl Pts',(-31.8186234857374,-34.4218373646645,
174.779253348358));
#33539=CARTESIAN_POINT('Ctrl Pts',(-33.936246825431,-33.4659951881979,174.668123559139));
#33540=CARTESIAN_POINT('Ctrl Pts',(-34.2818380682126,-31.1684901135484,
174.556993769919));
#33541=CARTESIAN_POINT('Ctrl Pts',(-32.5391158564695,-29.6319738696303,
174.445863980699));
#33542=CARTESIAN_POINT('Ctrl Pts',(-30.3030006593535,-30.2626494600523,
174.334734191479));
#33543=CARTESIAN_POINT('Ctrl Pts',(-29.6199608556057,-32.4833294238526,
174.22360440226));
#33544=CARTESIAN_POINT('Ctrl Pts',(-31.1151070663578,-34.2616715404322,
174.11247461304));
#33545=CARTESIAN_POINT('Ctrl Pts',(-33.420097693715,-33.9701563900148,174.00134482382));
#33546=CARTESIAN_POINT('Ctrl Pts',(-34.4254303121024,-31.8755754769123,
173.890215034601));
#33547=CARTESIAN_POINT('Ctrl Pts',(-33.2110354115502,-29.8948665380118,
173.779085245381));
#33548=CARTESIAN_POINT('Ctrl Pts',(-30.8883140354794,-29.8407529143012,
173.667955456161));
#33549=CARTESIAN_POINT('Ctrl Pts',(-29.5829955984056,-31.7627588073625,
173.556825666941));
#33550=CARTESIAN_POINT('Ctrl Pts',(-30.4896933783496,-33.9018852671521,
173.445695877722));
#33551=CARTESIAN_POINT('Ctrl Pts',(-32.7786073998349,-34.3004269555309,
173.334566088502));
#33552=CARTESIAN_POINT('Ctrl Pts',(-34.3549483726368,-32.5936428412994,
173.223436299282));
#33553=CARTESIAN_POINT('Ctrl Pts',(-33.7760661331533,-30.3435632364992,
173.112306510063));
#33554=CARTESIAN_POINT('Ctrl Pts',(-31.571747429243,-29.6094365943462,173.001176720843));
#33555=CARTESIAN_POINT('Ctrl Pts',(-29.7593608338838,-31.063127656467,172.890046931623));
#33556=CARTESIAN_POINT('Ctrl Pts',(-29.9975829046342,-33.3742341274316,
172.778917142403));
#33557=CARTESIAN_POINT('Ctrl Pts',(-32.0683953857542,-34.4276564279194,
172.667787353184));
#33558=CARTESIAN_POINT('Ctrl Pts',(-34.076613151549,-33.2593138924131,172.556657563964));
#33559=CARTESIAN_POINT('Ctrl Pts',(-34.184337080978,-30.9384609392607,172.445527774744));
#33560=CARTESIAN_POINT('Ctrl Pts',(-32.2929794020452,-29.5891170225852,
172.334397985524));
#33561=CARTESIAN_POINT('Ctrl Pts',(-30.1334901515899,-30.4461870619026,
172.223268196305));
#33562=CARTESIAN_POINT('Ctrl Pts',(-29.6822104729431,-32.7252898517669,
172.112138407085));
#33563=CARTESIAN_POINT('Ctrl Pts',(-31.352146634078,-34.3406152347352,172.001008617865));
#33564=CARTESIAN_POINT('Ctrl Pts',(-33.6149911700275,-33.813834937789,171.889878828645));
#33565=CARTESIAN_POINT('Ctrl Pts',(-34.3998133010178,-31.6270525759992,
171.778749039426));
#33566=CARTESIAN_POINT('Ctrl Pts',(-32.9883523238082,-29.7815876522084,
171.667619250206));
#33567=CARTESIAN_POINT('Ctrl Pts',(-30.6723620180839,-29.9663896514365,
171.556489460986));
#33568=CARTESIAN_POINT('Ctrl Pts',(-29.5714115957749,-32.0123297880839,
171.445359671767));
#33569=CARTESIAN_POINT('Ctrl Pts',(-30.6930789440682,-34.046985836388,171.334229882547));
#33570=CARTESIAN_POINT('Ctrl Pts',(-33.0108262697815,-34.2082626458667,
171.223100093327));
#33571=CARTESIAN_POINT('Ctrl Pts',(-34.4034763553453,-32.3485614294596,
171.111970304107));
#33572=CARTESIAN_POINT('Ctrl Pts',(-33.5964909451128,-30.1698605728022,
171.000840514888));
#33573=CARTESIAN_POINT('Ctrl Pts',(-31.3284143351364,-29.6660834728807,
170.889710725668));
#33574=CARTESIAN_POINT('Ctrl Pts',(-29.6749656425999,-31.298281468308,170.778580936448));
#33575=CARTESIAN_POINT('Ctrl Pts',(-30.1493631800083,-33.5726846541191,
170.667451147229));
#33576=CARTESIAN_POINT('Ctrl Pts',(-32.3174434657525,-34.4077838995354,
170.556321358009));
#33577=CARTESIAN_POINT('Ctrl Pts',(-34.195002934171,-33.0393054314259,170.445191568789));
#33578=CARTESIAN_POINT('Ctrl Pts',(-34.0637195210518,-30.7196659032736,
170.334061779569));
#33579=CARTESIAN_POINT('Ctrl Pts',(-32.0437423823724,-29.5717742558001,
170.22293199035));
#33580=CARTESIAN_POINT('Ctrl Pts',(-29.983732689712,-30.6461684764067,170.11180220113));
#33581=CARTESIAN_POINT('Ctrl Pts',(-29.7689889739188,-32.9595746257144,
170.00067241191));
#33582=CARTESIAN_POINT('Ctrl Pts',(-31.5960423548879,-34.3947884837217,
169.88954262269));
#33583=CARTESIAN_POINT('Ctrl Pts',(-33.7927933919256,-33.6383178918267,
169.778412833471));
#33584=CARTESIAN_POINT('Ctrl Pts',(-34.3487993587072,-31.3824765321494,
169.667283044251));
#33585=CARTESIAN_POINT('Ctrl Pts',(-32.7552096240695,-29.6917859534862,
169.556153255031));
#33586=CARTESIAN_POINT('Ctrl Pts',(-30.4704602313883,-30.1135478386525,
169.445023465812));
#33587=CARTESIAN_POINT('Ctrl Pts',(-29.5855290477775,-32.2617702841642,
169.333893676592));
#33588=CARTESIAN_POINT('Ctrl Pts',(-30.9102954957832,-34.1704234043853,
169.222763887372));
#33589=CARTESIAN_POINT('Ctrl Pts',(-33.2323476887161,-34.0927285621829,
169.111634098152));
#33590=CARTESIAN_POINT('Ctrl Pts',(-34.4265686411468,-32.09979123455,169.000504308932));
#33591=CARTESIAN_POINT('Ctrl Pts',(-33.4000202883296,-30.0155260512825,
168.889374519713));
#33592=CARTESIAN_POINT('Ctrl Pts',(-31.0921885500407,-29.7474299050867,
168.778244730493));
#33593=CARTESIAN_POINT('Ctrl Pts',(-29.6151760063164,-31.540861481794,168.667114941273));
#33594=CARTESIAN_POINT('Ctrl Pts',(-30.3207285185246,-33.7544916509204,
168.555985152054));
#33595=CARTESIAN_POINT('Ctrl Pts',(-32.56313208116,-34.3624300883911,168.444855362834));
#33596=CARTESIAN_POINT('Ctrl Pts',(-34.2901632669325,-32.8082981272383,
168.333725573614));
#33597=CARTESIAN_POINT('Ctrl Pts',(-33.9212618729032,-30.5144204881399,
168.222595784395));
#33598=CARTESIAN_POINT('Ctrl Pts',(-31.7940424351662,-29.5801291028184,
168.111465995175));
#33599=CARTESIAN_POINT('Ctrl Pts',(-29.8553131533993,-30.8604773304489,
168.000336205955));
#33600=CARTESIAN_POINT('Ctrl Pts',(-29.8793779622368,-33.1837043267573,
167.889206416735));
#33601=CARTESIAN_POINT('Ctrl Pts',(-31.8442131712534,-34.4236180024818,
167.778076627516));
#33602=CARTESIAN_POINT('Ctrl Pts',(-33.9516225757822,-33.4454626787946,
167.666946838296));
#33603=CARTESIAN_POINT('Ctrl Pts',(-34.2729286128104,-31.1444357631505,
167.555817049076));
#33604=CARTESIAN_POINT('Ctrl Pts',(-32.514074117309,-29.6264115999403,167.444687259856));
#33605=CARTESIAN_POINT('Ctrl Pts',(-30.2847464274524,-30.2806705307475,
167.333557470637));
#33606=CARTESIAN_POINT('Ctrl Pts',(-29.6251964131156,-32.5084396585803,
167.222427681417));
#33607=CARTESIAN_POINT('Ctrl Pts',(-31.139048610325,-34.2708933540495,167.111297892197));
#33608=CARTESIAN_POINT('Ctrl Pts',(-33.4408184595056,-33.9550439108221,
167.000168102978));
#33609=CARTESIAN_POINT('Ctrl Pts',(-34.4239988925092,-31.8499720399622,
166.889038313758));
#33610=CARTESIAN_POINT('Ctrl Pts',(-33.1886966470223,-29.8821785627325,
166.777908524538));
#33611=CARTESIAN_POINT('Ctrl Pts',(-30.8656448278897,-29.8526443561693,
166.666778735318));
#33612=CARTESIAN_POINT('Ctrl Pts',(-29.580472364777,-31.7882407548095,166.555648946099));
#33613=CARTESIAN_POINT('Ctrl Pts',(-30.5101755007489,-33.9178527489701,
166.444519156879));
#33614=CARTESIAN_POINT('Ctrl Pts',(-32.8022294941794,-34.2918270332952,
166.333389367659));
#33615=CARTESIAN_POINT('Ctrl Pts',(-34.3623780230438,-32.5692489716029,
166.222259578439));
#33616=CARTESIAN_POINT('Ctrl Pts',(-33.7557951165766,-30.3238345627424,
166.11112978922));
#33617=CARTESIAN_POINT('Ctrl Pts',(-32.2875197530252,-29.8538180613451,
166.037043263073));
#33618=CARTESIAN_POINT('Ctrl Pts',(-31.6163320011535,-29.981387499008,166.));
#33619=CARTESIAN_POINT('Ctrl Pts',(-30.7309291201476,-30.9206413469516,
179.));
#33620=CARTESIAN_POINT('Ctrl Pts',(-30.6856062030546,-30.962922818334,179.));
#33621=CARTESIAN_POINT('Ctrl Pts',(-30.6430136434112,-31.0077738784331,
179.));
#33622=CARTESIAN_POINT('Ctrl Pts',(-30.6031497132239,-31.0548493830004,
179.));
#33623=CARTESIAN_POINT('Ctrl Pts',(-30.5606495403132,-31.1050380391255,
179.));
#33624=CARTESIAN_POINT('Ctrl Pts',(-30.5212500994078,-31.1577553100502,
179.));
#33625=CARTESIAN_POINT('Ctrl Pts',(-30.4849781474539,-31.2126376829455,
179.));
#33626=CARTESIAN_POINT('Ctrl Pts',(-30.4532401894943,-31.260659759229,179.));
#33627=CARTESIAN_POINT('Ctrl Pts',(-30.4238969592621,-31.3103407178797,
179.));
#33628=CARTESIAN_POINT('Ctrl Pts',(-30.3969892820085,-31.3614645973307,
179.));
#33629=CARTESIAN_POINT('Ctrl Pts',(-30.3834951193651,-31.3871031516275,
179.));
#33630=CARTESIAN_POINT('Ctrl Pts',(-30.3706138609554,-31.4131049574139,
179.));
#33631=CARTESIAN_POINT('Ctrl Pts',(-30.3583529950348,-31.4394446156991,
179.));
#33632=CARTESIAN_POINT('Ctrl Pts',(-30.3527381728228,-31.4515067734091,
179.));
#33633=CARTESIAN_POINT('Ctrl Pts',(-30.3472528660996,-31.4636414961716,
179.));
#33634=CARTESIAN_POINT('Ctrl Pts',(-30.3419063336923,-31.4758263198916,
179.));
#33635=CARTESIAN_POINT('Ctrl Pts',(-30.314994749283,-31.5371582051345,179.));
#33636=CARTESIAN_POINT('Ctrl Pts',(-30.2915439633216,-31.5998656461968,
179.));
#33637=CARTESIAN_POINT('Ctrl Pts',(-30.2715772012624,-31.6635906893212,
179.));
#33638=CARTESIAN_POINT('Ctrl Pts',(-30.2512551602859,-31.7284496250744,
179.));
#33639=CARTESIAN_POINT('Ctrl Pts',(-30.2345416753266,-31.7943635399902,
179.));
#33640=CARTESIAN_POINT('Ctrl Pts',(-30.2215005522,-31.860991549714,179.));
#33641=CARTESIAN_POINT('Ctrl Pts',(-30.210592869978,-31.9167196607127,179.));
#33642=CARTESIAN_POINT('Ctrl Pts',(-30.2022548395526,-31.9729482768223,
179.));
#33643=CARTESIAN_POINT('Ctrl Pts',(-30.1965486177622,-32.0294902235943,
179.));
#33644=CARTESIAN_POINT('Ctrl Pts',(-30.1939214710931,-32.0555221572595,
179.));
#33645=CARTESIAN_POINT('Ctrl Pts',(-30.1918525198042,-32.0816206201513,
179.));
#33646=CARTESIAN_POINT('Ctrl Pts',(-30.1903496283998,-32.107767746287,179.));
#33647=CARTESIAN_POINT('Ctrl Pts',(-30.1896917076954,-32.1192141725515,
179.));
#33648=CARTESIAN_POINT('Ctrl Pts',(-30.189142383326,-32.1306697639313,179.));
#33649=CARTESIAN_POINT('Ctrl Pts',(-30.1887026532007,-32.1421188060292,
179.));
#33650=CARTESIAN_POINT('Ctrl Pts',(-30.1860090542042,-32.2122507495274,
179.));
#33651=CARTESIAN_POINT('Ctrl Pts',(-30.1874155654491,-32.2822683610148,
179.));
#33652=CARTESIAN_POINT('Ctrl Pts',(-30.1929765281086,-32.3518105278729,
179.));
#33653=CARTESIAN_POINT('Ctrl Pts',(-30.1979467071931,-32.4139646987207,
179.));
#33654=CARTESIAN_POINT('Ctrl Pts',(-30.2062358596473,-32.4757400430717,
179.));
#33655=CARTESIAN_POINT('Ctrl Pts',(-30.2179158795994,-32.5368908724721,
179.));
#33656=CARTESIAN_POINT('Ctrl Pts',(-30.2306456144363,-32.6035374917853,
179.));
#33657=CARTESIAN_POINT('Ctrl Pts',(-30.2474020092586,-32.6694431322195,
179.));
#33658=CARTESIAN_POINT('Ctrl Pts',(-30.2679400111633,-32.7343943852058,
179.));
#33659=CARTESIAN_POINT('Ctrl Pts',(-30.2758707783801,-32.7594753677795,
179.));
#33660=CARTESIAN_POINT('Ctrl Pts',(-30.2843659849015,-32.7844139919257,
179.));
#33661=CARTESIAN_POINT('Ctrl Pts',(-30.2934135323341,-32.8091976483089,
179.));
#33662=CARTESIAN_POINT('Ctrl Pts',(-30.2973812067702,-32.8200661715852,
179.));
#33663=CARTESIAN_POINT('Ctrl Pts',(-30.3014550058364,-32.8309043340832,
179.));
#33664=CARTESIAN_POINT('Ctrl Pts',(-30.3056288188997,-32.8416985210892,
179.));
#33665=CARTESIAN_POINT('Ctrl Pts',(-30.3308503323267,-32.9069256235929,
179.));
#33666=CARTESIAN_POINT('Ctrl Pts',(-30.3597622632288,-32.9706662212829,
179.));
#33667=CARTESIAN_POINT('Ctrl Pts',(-30.3920521450586,-33.0327016892519,
179.));
#33668=CARTESIAN_POINT('Ctrl Pts',(-30.425088851225,-33.096171959536,179.));
#33669=CARTESIAN_POINT('Ctrl Pts',(-30.4616618729745,-33.1578581320537,
179.));
#33670=CARTESIAN_POINT('Ctrl Pts',(-30.5014926867972,-33.2175223280988,
179.));
#33671=CARTESIAN_POINT('Ctrl Pts',(-30.5319855016706,-33.2631987557176,
179.));
#33672=CARTESIAN_POINT('Ctrl Pts',(-30.5643888576175,-33.3076901760244,
179.));
#33673=CARTESIAN_POINT('Ctrl Pts',(-30.5985973406978,-33.3508837471854,
179.));
#33674=CARTESIAN_POINT('Ctrl Pts',(-30.619899662223,-33.3777812666846,179.));
#33675=CARTESIAN_POINT('Ctrl Pts',(-30.6419023011681,-33.4041753823072,
179.));
#33676=CARTESIAN_POINT('Ctrl Pts',(-30.664582713691,-33.4300371526971,179.));
#33677=CARTESIAN_POINT('Ctrl Pts',(-30.6772410834679,-33.4444710988324,
179.));
#33678=CARTESIAN_POINT('Ctrl Pts',(-30.6901150229931,-33.4587437314971,
179.));
#33679=CARTESIAN_POINT('Ctrl Pts',(-30.7031769988168,-33.4728246891271,
179.));
#33680=CARTESIAN_POINT('Ctrl Pts',(-30.7540414798183,-33.5276571747721,
179.));
#33681=CARTESIAN_POINT('Ctrl Pts',(-30.8078024741205,-33.5796445815827,
179.));
#33682=CARTESIAN_POINT('Ctrl Pts',(-30.8641753039031,-33.6285232274692,
179.));
#33683=CARTESIAN_POINT('Ctrl Pts',(-30.9063225983237,-33.6650674755938,
179.));
#33684=CARTESIAN_POINT('Ctrl Pts',(-30.9499310243967,-33.6998737756725,
179.));
#33685=CARTESIAN_POINT('Ctrl Pts',(-30.994897985227,-33.7328221880585,179.));
#33686=CARTESIAN_POINT('Ctrl Pts',(-31.0089818323205,-33.7431417736709,
179.));
#33687=CARTESIAN_POINT('Ctrl Pts',(-31.0231990403432,-33.7532790290714,
179.));
#33688=CARTESIAN_POINT('Ctrl Pts',(-31.0375466996756,-33.7632300412436,
179.));
#33689=CARTESIAN_POINT('Ctrl Pts',(-31.0513257036538,-33.7727866548438,
179.));
#33690=CARTESIAN_POINT('Ctrl Pts',(-31.065217962404,-33.7821665362252,179.));
#33691=CARTESIAN_POINT('Ctrl Pts',(-31.0792155749848,-33.7913635116716,
179.));
#33692=CARTESIAN_POINT('Ctrl Pts',(-31.1421637728842,-33.8327229240097,
179.));
#33693=CARTESIAN_POINT('Ctrl Pts',(-31.2072699803896,-33.870407069935,179.));
#33694=CARTESIAN_POINT('Ctrl Pts',(-31.2742731852794,-33.9041370162845,
179.));
#33695=CARTESIAN_POINT('Ctrl Pts',(-31.3254578858164,-33.9299038017072,
179.));
#33696=CARTESIAN_POINT('Ctrl Pts',(-31.3777505811556,-33.9533626457797,
179.));
#33697=CARTESIAN_POINT('Ctrl Pts',(-31.4310487463576,-33.9743739898132,
179.));
#33698=CARTESIAN_POINT('Ctrl Pts',(-31.4435331568518,-33.979295627227,179.));
#33699=CARTESIAN_POINT('Ctrl Pts',(-31.4560727789483,-33.9840829100841,
179.));
#33700=CARTESIAN_POINT('Ctrl Pts',(-31.4686656554564,-33.9887364314851,
179.));
#33701=CARTESIAN_POINT('Ctrl Pts',(-33.6673324974466,-32.0013033571361,
177.87148036339));
#33702=CARTESIAN_POINT('Ctrl Pts',(-33.668068719752,-32.0869545002621,177.877220944861));
#33703=CARTESIAN_POINT('Ctrl Pts',(-33.6620385737897,-32.1725016588414,
177.882961526332));
#33704=CARTESIAN_POINT('Ctrl Pts',(-33.6488812404577,-32.2569381526634,
177.888702107803));
#33705=CARTESIAN_POINT('Ctrl Pts',(-33.5639785938473,-32.801796416502,177.925745370876));
#33706=CARTESIAN_POINT('Ctrl Pts',(-33.1823026113929,-33.3004070278029,
177.962788633949));
#33707=CARTESIAN_POINT('Ctrl Pts',(-32.678505164673,-33.5246153329366,177.999831897022));
#33708=CARTESIAN_POINT('Ctrl Pts',(-32.1747077179532,-33.7488236380704,
178.036875160096));
#33709=CARTESIAN_POINT('Ctrl Pts',(-31.5487888069679,-33.698629637037,178.073918423169));
#33710=CARTESIAN_POINT('Ctrl Pts',(-31.0871675439728,-33.3969878684481,
178.110961686242));
#33711=CARTESIAN_POINT('Ctrl Pts',(-30.6255462809778,-33.0953460998591,
178.148004949315));
#33712=CARTESIAN_POINT('Ctrl Pts',(-30.3282226659731,-32.5422565637145,
178.185048212389));
#33713=CARTESIAN_POINT('Ctrl Pts',(-30.3312462755294,-31.9908384640567,
178.222091475462));
#33714=CARTESIAN_POINT('Ctrl Pts',(-30.3342698850858,-31.4394203643989,
178.259134738535));
#33715=CARTESIAN_POINT('Ctrl Pts',(-30.6376407192033,-30.8896737012279,
178.296178001608));
#33716=CARTESIAN_POINT('Ctrl Pts',(-31.1025462716722,-30.593101679575,178.333221264682));
#33717=CARTESIAN_POINT('Ctrl Pts',(-31.567451824141,-30.2965296579222,178.370264527755));
#33718=CARTESIAN_POINT('Ctrl Pts',(-32.1938920949612,-30.2531322777876,
178.407307790828));
#33719=CARTESIAN_POINT('Ctrl Pts',(-32.6951944291635,-30.4828858091372,
178.444351053901));
#33720=CARTESIAN_POINT('Ctrl Pts',(-33.1964967633658,-30.7126393404869,
178.481394316975));
#33721=CARTESIAN_POINT('Ctrl Pts',(-33.5726611609501,-31.2155437833208,
178.518437580048));
#33722=CARTESIAN_POINT('Ctrl Pts',(-33.6515914003734,-31.7612327671255,
178.555480843121));
#33723=CARTESIAN_POINT('Ctrl Pts',(-33.6629551037905,-31.839796417955,178.560814016544));
#33724=CARTESIAN_POINT('Ctrl Pts',(-33.6681578008391,-31.9192468976437,
178.566147189967));
#33725=CARTESIAN_POINT('Ctrl Pts',(-33.6674973899495,-31.9987820730806,
178.57148036339));
#33726=CARTESIAN_POINT('Ctrl Pts',(-32.5301702171889,-33.9851743256717,
179.));
#33727=CARTESIAN_POINT('Ctrl Pts',(-33.190239790753,-33.8088929660697,178.962956736927));
#33728=CARTESIAN_POINT('Ctrl Pts',(-34.3091776399806,-32.7483617530395,
178.88887021078));
#33729=CARTESIAN_POINT('Ctrl Pts',(-33.8814412030322,-30.4621270434605,
178.777740421561));
#33730=CARTESIAN_POINT('Ctrl Pts',(-31.7283973144122,-29.5870608054774,
178.666610632341));
#33731=CARTESIAN_POINT('Ctrl Pts',(-29.8255893685038,-30.9184850177167,
178.555480843121));
#33732=CARTESIAN_POINT('Ctrl Pts',(-29.9119598065434,-33.2405821817579,
178.444351053901));
#33733=CARTESIAN_POINT('Ctrl Pts',(-31.909683998457,-34.4268788699842,178.333221264681));
#33734=CARTESIAN_POINT('Ctrl Pts',(-33.9898669711731,-33.392335043116,178.222091475462));
#33735=CARTESIAN_POINT('Ctrl Pts',(-34.2490422451154,-31.0834368136807,
178.110961686242));
#33736=CARTESIAN_POINT('Ctrl Pts',(-32.4498708176529,-29.6134185829238,
177.999831897022));
#33737=CARTESIAN_POINT('Ctrl Pts',(-30.23900588914,-30.3275485827783,177.888702107803));
#33738=CARTESIAN_POINT('Ctrl Pts',(-29.6397721844782,-32.5723003600472,
177.777572318583));
#33739=CARTESIAN_POINT('Ctrl Pts',(-31.2005990238776,-34.293282975036,177.666442529363));
#33740=CARTESIAN_POINT('Ctrl Pts',(-33.4930261959862,-33.9154808666257,
177.555312740144));
#33741=CARTESIAN_POINT('Ctrl Pts',(-34.4190533459356,-31.7846499751686,
177.444182950924));
#33742=CARTESIAN_POINT('Ctrl Pts',(-33.1311884386701,-29.8509058112995,
177.333053161704));
#33743=CARTESIAN_POINT('Ctrl Pts',(-30.8080724679209,-29.8839889892312,
177.221923372484));
#33744=CARTESIAN_POINT('Ctrl Pts',(-29.5757954873418,-31.853622670774,177.110793583265));
#33745=CARTESIAN_POINT('Ctrl Pts',(-30.562124266553,-33.9572192112968,176.999663794045));
#33746=CARTESIAN_POINT('Ctrl Pts',(-32.8643812849987,-34.2695899967097,
176.888534004825));
#33747=CARTESIAN_POINT('Ctrl Pts',(-34.3755659443455,-32.5048566092284,
176.777404215605));
#33748=CARTESIAN_POINT('Ctrl Pts',(-33.7126584039828,-30.278083938033,176.666274426386));
#33749=CARTESIAN_POINT('Ctrl Pts',(-31.4823444699111,-29.6271901683823,
176.555144637166));
#33750=CARTESIAN_POINT('Ctrl Pts',(-29.7257832609726,-31.1478662270158,
176.444014847946));
#33751=CARTESIAN_POINT('Ctrl Pts',(-30.0505605498502,-33.4484058724806,
176.332885058726));
#33752=CARTESIAN_POINT('Ctrl Pts',(-32.1594436821683,-34.4233801713471,
176.221755269507));
#33753=CARTESIAN_POINT('Ctrl Pts',(-34.1224056859289,-33.1805032175714,
176.110625480287));
#33754=CARTESIAN_POINT('Ctrl Pts',(-34.1429650223268,-30.8572425212406,
175.999495691067));
#33755=CARTESIAN_POINT('Ctrl Pts',(-32.2023060098439,-29.5798210767118,
175.888365901848));
#33756=CARTESIAN_POINT('Ctrl Pts',(-30.0764987310374,-30.5173211370632,
175.777236112628));
#33757=CARTESIAN_POINT('Ctrl Pts',(-29.7110589540984,-32.8117528137747,
175.666106323408));
#33758=CARTESIAN_POINT('Ctrl Pts',(-31.4404331998289,-34.3632771184206,
175.554976534188));
#33759=CARTESIAN_POINT('Ctrl Pts',(-33.6819169128305,-33.7519558329571,
175.443846744969));
#33760=CARTESIAN_POINT('Ctrl Pts',(-34.3841285068372,-31.5372635683431,
175.332716955749));
#33761=CARTESIAN_POINT('Ctrl Pts',(-32.9044115461845,-29.7460626678129,
175.221587166529));
#33762=CARTESIAN_POINT('Ctrl Pts',(-30.5969869463981,-30.0176407707682,
175.110457377309));
#33763=CARTESIAN_POINT('Ctrl Pts',(-29.5735846782254,-32.1034525425256,
174.99932758809));
#33764=CARTESIAN_POINT('Ctrl Pts',(-30.7708113991622,-34.0945856692598,
174.88819779887));
#33765=CARTESIAN_POINT('Ctrl Pts',(-33.0929781975906,-34.168776706323,174.77706800965));
#33766=CARTESIAN_POINT('Ctrl Pts',(-34.414863202439,-32.2581268211635,174.665938220431));
#33767=CARTESIAN_POINT('Ctrl Pts',(-33.5266915925162,-30.1112420685439,
174.554808431211));
#33768=CARTESIAN_POINT('Ctrl Pts',(-31.2413083934035,-29.6929280920661,
174.443678641991));
#33769=CARTESIAN_POINT('Ctrl Pts',(-29.65027152498,-31.3860213065764,174.332548852771));
#33770=CARTESIAN_POINT('Ctrl Pts',(-30.2096806751507,-33.6410211629863,
174.221419063552));
#33771=CARTESIAN_POINT('Ctrl Pts',(-32.4075706562188,-34.3941762471646,
174.110289274332));
#33772=CARTESIAN_POINT('Ctrl Pts',(-34.2324563926352,-32.9562071936981,
173.999159485112));
#33773=CARTESIAN_POINT('Ctrl Pts',(-34.0142222484933,-30.6431276861944,
173.888029695892));
#33774=CARTESIAN_POINT('Ctrl Pts',(-31.9525937458611,-29.571843005618,173.776899906673));
#33775=CARTESIAN_POINT('Ctrl Pts',(-29.9343509329174,-30.722781274034,173.665770117453));
#33776=CARTESIAN_POINT('Ctrl Pts',(-29.8065677451363,-33.0426162695937,
173.554640328234));
#33777=CARTESIAN_POINT('Ctrl Pts',(-31.6861899702242,-34.4082601619239,
173.443510539014));
#33778=CARTESIAN_POINT('Ctrl Pts',(-33.8530077314349,-33.5698904705553,
173.332380749794));
#33779=CARTESIAN_POINT('Ctrl Pts',(-34.3239729118684,-31.2947740452877,
173.221250960574));
#33780=CARTESIAN_POINT('Ctrl Pts',(-32.6680632857967,-29.6650727659158,
173.110121171355));
#33781=CARTESIAN_POINT('Ctrl Pts',(-30.4007493854086,-30.1722715699463,
172.998991382135));
#33782=CARTESIAN_POINT('Ctrl Pts',(-29.5970523043438,-32.3521876122724,
172.887861592915));
#33783=CARTESIAN_POINT('Ctrl Pts',(-30.9925068954609,-34.2097853711626,
172.776731803695));
#33784=CARTESIAN_POINT('Ctrl Pts',(-33.3100082500444,-34.0450115224891,
172.665602014476));
#33785=CARTESIAN_POINT('Ctrl Pts',(-34.4286042606353,-32.0086653056602,
172.554472225256));
#33786=CARTESIAN_POINT('Ctrl Pts',(-33.3245679890092,-29.9643886950623,
172.443342436036));
#33787=CARTESIAN_POINT('Ctrl Pts',(-31.0083014581836,-29.7830814754581,
172.332212646816));
#33788=CARTESIAN_POINT('Ctrl Pts',(-29.5996266783055,-31.6306740480343,
172.221082857597));
#33789=CARTESIAN_POINT('Ctrl Pts',(-30.3877475314776,-33.8162697266764,
172.109953068377));
#33790=CARTESIAN_POINT('Ctrl Pts',(-32.6513843596913,-34.3396350480892,
171.998823279157));
#33791=CARTESIAN_POINT('Ctrl Pts',(-34.3188812858848,-32.7217917457764,
171.887693489937));
#33792=CARTESIAN_POINT('Ctrl Pts',(-33.864163206457,-30.4433724652345,171.776563700718));
#33793=CARTESIAN_POINT('Ctrl Pts',(-31.7033831764878,-29.5895618235874,
171.665433911498));
#33794=CARTESIAN_POINT('Ctrl Pts',(-29.8140636467216,-30.9417580608795,
171.554304122278));
#33795=CARTESIAN_POINT('Ctrl Pts',(-29.925289361983,-33.2624458446987,171.443174333059));
#33796=CARTESIAN_POINT('Ctrl Pts',(-31.9352677538577,-34.4277568821048,
171.332044543839));
#33797=CARTESIAN_POINT('Ctrl Pts',(-34.0044883954098,-33.3712111489356,
171.220914754619));
#33798=CARTESIAN_POINT('Ctrl Pts',(-34.2392229952543,-31.0597478424262,
171.109784965399));
#33799=CARTESIAN_POINT('Ctrl Pts',(-32.4246449932043,-29.6087931139184,
170.99865517618));
#33800=CARTESIAN_POINT('Ctrl Pts',(-30.2214364984569,-30.3462449959935,
170.88752538696));
#33801=CARTESIAN_POINT('Ctrl Pts',(-29.6459500326037,-32.5971955235092,
170.77639559774));
#33802=CARTESIAN_POINT('Ctrl Pts',(-31.2248645683027,-34.3015991842251,
170.66526580852));
#33803=CARTESIAN_POINT('Ctrl Pts',(-33.5131746450974,-33.8996042313419,
170.554136019301));
#33804=CARTESIAN_POINT('Ctrl Pts',(-34.4166436963946,-31.7591120862848,
170.443006230081));
#33805=CARTESIAN_POINT('Ctrl Pts',(-33.1084266441611,-29.8390779475391,
170.331876440861));
#33806=CARTESIAN_POINT('Ctrl Pts',(-30.7857895475778,-29.8966962369818,
170.220746651642));
#33807=CARTESIAN_POINT('Ctrl Pts',(-29.5743846894872,-31.8792353209593,
170.109616862422));
#33808=CARTESIAN_POINT('Ctrl Pts',(-30.5828766588753,-33.9722969295563,
169.998487073202));
#33809=CARTESIAN_POINT('Ctrl Pts',(-32.888304541998,-34.2603337768931,169.887357283982));
#33810=CARTESIAN_POINT('Ctrl Pts',(-34.3807657415457,-32.4797376639163,
169.776227494763));
#33811=CARTESIAN_POINT('Ctrl Pts',(-33.6943759527602,-30.2600908434617,
169.665097705543));
#33812=CARTESIAN_POINT('Ctrl Pts',(-31.4573116667505,-29.6327900145418,
169.553967916323));
#33813=CARTESIAN_POINT('Ctrl Pts',(-29.7169098581211,-31.1719340929902,
169.442838127103));
#33814=CARTESIAN_POINT('Ctrl Pts',(-30.065967388257,-33.4689151095322,169.331708337884));
#33815=CARTESIAN_POINT('Ctrl Pts',(-32.1850305909512,-34.4215609475536,
169.220578548664));
#33816=CARTESIAN_POINT('Ctrl Pts',(-34.1347558033771,-33.1580204671043,
169.109448759444));
#33817=CARTESIAN_POINT('Ctrl Pts',(-34.1307756550211,-30.8346722133795,
168.998318970225));
#33818=CARTESIAN_POINT('Ctrl Pts',(-32.1767327344769,-29.5778193124972,
168.887189181005));
#33819=CARTESIAN_POINT('Ctrl Pts',(-30.0609459319521,-30.5377199094004,
168.776059391785));
#33820=CARTESIAN_POINT('Ctrl Pts',(-29.719760384286,-32.8358833873742,168.664929602565));
#33821=CARTESIAN_POINT('Ctrl Pts',(-31.4654254048604,-34.3690554541617,
168.553799813346));
#33822=CARTESIAN_POINT('Ctrl Pts',(-33.7003272974666,-33.7340936603098,
168.442670024126));
#33823=CARTESIAN_POINT('Ctrl Pts',(-34.3791080871609,-31.5121081546712,
168.331540234906));
#33824=CARTESIAN_POINT('Ctrl Pts',(-32.8805549549265,-29.7366359735545,
168.220410445687));
#33825=CARTESIAN_POINT('Ctrl Pts',(-30.576127479021,-30.0325700070413,168.109280656467));
#33826=CARTESIAN_POINT('Ctrl Pts',(-29.5748126892805,-32.1290746285719,
167.998150867247));
#33827=CARTESIAN_POINT('Ctrl Pts',(-30.7930030339464,-34.1074515612365,
167.887021078027));
#33828=CARTESIAN_POINT('Ctrl Pts',(-33.1158238969359,-34.1571116561114,
167.775891288808));
#33829=CARTESIAN_POINT('Ctrl Pts',(-34.4174548619641,-32.2326066036682,
167.664761499588));
#33830=CARTESIAN_POINT('Ctrl Pts',(-33.5066572885625,-30.0952224134444,
167.553631710368));
#33831=CARTESIAN_POINT('Ctrl Pts',(-31.2169834359616,-29.7010702107005,
167.442501921148));
#33832=CARTESIAN_POINT('Ctrl Pts',(-29.643917581989,-31.4108732197425,167.331372131929));
#33833=CARTESIAN_POINT('Ctrl Pts',(-30.2271133546761,-33.6598394847521,
167.220242342709));
#33834=CARTESIAN_POINT('Ctrl Pts',(-32.4328346425493,-34.389736993149,167.109112553489));
#33835=CARTESIAN_POINT('Ctrl Pts',(-34.2424326326234,-32.932576501644,166.99798276427));
#33836=CARTESIAN_POINT('Ctrl Pts',(-33.9997759672129,-30.6219252261187,
166.886852975049));
#33837=CARTESIAN_POINT('Ctrl Pts',(-31.9269554466752,-29.5724870533531,
166.77572318583));
#33838=CARTESIAN_POINT('Ctrl Pts',(-29.9209653227032,-30.7446538702704,
166.66459339661));
#33839=CARTESIAN_POINT('Ctrl Pts',(-29.8177242538605,-33.0657579476906,
166.553463607391));
#33840=CARTESIAN_POINT('Ctrl Pts',(-31.7115987445193,-34.4113736221389,
166.442333818171));
#33841=CARTESIAN_POINT('Ctrl Pts',(-33.8695768792418,-33.5503671474171,
166.331204028951));
#33842=CARTESIAN_POINT('Ctrl Pts',(-34.3162088044827,-31.2699910786138,
166.220074239731));
#33843=CARTESIAN_POINT('Ctrl Pts',(-32.6437429613104,-29.6587100617298,
166.108944450512));
#33844=CARTESIAN_POINT('Ctrl Pts',(-30.3807636536437,-30.1881093063979,
165.997814661292));
#33845=CARTESIAN_POINT('Ctrl Pts',(-29.6025035271829,-32.3799438764187,
165.886684872072));
#33846=CARTESIAN_POINT('Ctrl Pts',(-30.5427968191103,-33.6016627022545,
165.812598345926));
#33847=CARTESIAN_POINT('Ctrl Pts',(-31.1673980508611,-33.878502477185,165.775555082853));
#33848=CARTESIAN_POINT('Ctrl Pts',(-32.4967348970879,-33.8599788000027,
179.074814972382));
#33849=CARTESIAN_POINT('Ctrl Pts',(-33.1151770144777,-33.6948146693492,
179.037771709309));
#33850=CARTESIAN_POINT('Ctrl Pts',(-34.1635487625758,-32.7011661280252,
178.963685183163));
#33851=CARTESIAN_POINT('Ctrl Pts',(-33.7627876332259,-30.5591133940879,
178.852555393943));
#33852=CARTESIAN_POINT('Ctrl Pts',(-31.7455260071196,-29.73923343181,178.741425604723));
#33853=CARTESIAN_POINT('Ctrl Pts',(-29.9627191301121,-30.9866910361882,
178.630295815504));
#33854=CARTESIAN_POINT('Ctrl Pts',(-30.0436425944261,-33.1623445497413,
178.519166026284));
#33855=CARTESIAN_POINT('Ctrl Pts',(-31.9153798001522,-34.2738271344597,
178.408036237064));
#33856=CARTESIAN_POINT('Ctrl Pts',(-33.8643755026176,-33.3045270781549,
178.296906447844));
#33857=CARTESIAN_POINT('Ctrl Pts',(-34.1072058217405,-31.1412401050271,
178.185776658625));
#33858=CARTESIAN_POINT('Ctrl Pts',(-32.4214995996843,-29.7639289492925,
178.074646869405));
#33859=CARTESIAN_POINT('Ctrl Pts',(-30.3500634323281,-30.4330221583869,
177.963517080185));
#33860=CARTESIAN_POINT('Ctrl Pts',(-29.7886205542368,-32.5362080917309,
177.852387290965));
#33861=CARTESIAN_POINT('Ctrl Pts',(-31.251013450526,-34.1486564987339,177.741257501746));
#33862=CARTESIAN_POINT('Ctrl Pts',(-33.3988681177627,-33.7946805767444,
177.630127712526));
#33863=CARTESIAN_POINT('Ctrl Pts',(-34.2664951290832,-31.798231079464,177.518997923306));
#33864=CARTESIAN_POINT('Ctrl Pts',(-33.0598497509898,-29.9864389849795,
177.407868134087));
#33865=CARTESIAN_POINT('Ctrl Pts',(-30.8832416820338,-30.0174357638488,
177.296738344867));
#33866=CARTESIAN_POINT('Ctrl Pts',(-29.7286785638387,-31.8628539944121,
177.185608555647));
#33867=CARTESIAN_POINT('Ctrl Pts',(-30.6528042667765,-33.8337866820529,
177.074478766427));
#33868=CARTESIAN_POINT('Ctrl Pts',(-32.8098688585814,-34.1264577241346,
176.963348977208));
#33869=CARTESIAN_POINT('Ctrl Pts',(-34.2257502715768,-32.4730176982761,
176.852219187988));
#33870=CARTESIAN_POINT('Ctrl Pts',(-33.6046491644892,-30.3866770140909,
176.741089398768));
#33871=CARTESIAN_POINT('Ctrl Pts',(-31.5149905480751,-29.7768320261982,
176.629959609548));
#33872=CARTESIAN_POINT('Ctrl Pts',(-29.8692073202332,-31.2016062609611,
176.518829820329));
#33873=CARTESIAN_POINT('Ctrl Pts',(-30.1735024464712,-33.3570617863506,
176.407700031109));
#33874=CARTESIAN_POINT('Ctrl Pts',(-32.149388325646,-34.2705490821455,176.296570241889));
#33875=CARTESIAN_POINT('Ctrl Pts',(-33.9885556294898,-33.1060544807695,
176.18544045267));
#33876=CARTESIAN_POINT('Ctrl Pts',(-34.007818386089,-30.9293108133877,176.07431066345));
#33877=CARTESIAN_POINT('Ctrl Pts',(-32.1895475296838,-29.7324502783874,
175.96318087423));
#33878=CARTESIAN_POINT('Ctrl Pts',(-30.1978048296397,-30.6108266580862,
175.85205108501));
#33879=CARTESIAN_POINT('Ctrl Pts',(-29.8554116055311,-32.7605594153313,
175.740921295791));
#33880=CARTESIAN_POINT('Ctrl Pts',(-31.4757224229406,-34.2142364435962,
175.629791506571));
#33881=CARTESIAN_POINT('Ctrl Pts',(-33.5758463933248,-33.6414682910725,
175.518661717351));
#33882=CARTESIAN_POINT('Ctrl Pts',(-34.2337728338789,-31.5664461595434,
175.407531928132));
#33883=CARTESIAN_POINT('Ctrl Pts',(-32.8473746011256,-29.8882078011037,
175.296402138912));
#33884=CARTESIAN_POINT('Ctrl Pts',(-30.6854683228166,-30.1426587616615,
175.185272349692));
#33885=CARTESIAN_POINT('Ctrl Pts',(-29.7266071799636,-32.0969282815195,
175.074142560472));
#33886=CARTESIAN_POINT('Ctrl Pts',(-30.8483304920893,-33.9624900892745,
174.963012771253));
#33887=CARTESIAN_POINT('Ctrl Pts',(-33.0240492485192,-34.0320022496441,
174.851882982033));
#33888=CARTESIAN_POINT('Ctrl Pts',(-34.2625692380559,-32.2418479872864,
174.740753192813));
#33889=CARTESIAN_POINT('Ctrl Pts',(-33.4304103974656,-30.2303570696963,
174.629623403593));
#33890=CARTESIAN_POINT('Ctrl Pts',(-31.2891554732695,-29.8384241709418,
174.518493614374));
#33891=CARTESIAN_POINT('Ctrl Pts',(-29.7984577511493,-31.4247420296276,
174.407363825154));
#33892=CARTESIAN_POINT('Ctrl Pts',(-30.3225876204458,-33.5375297443853,
174.296234035934));
#33893=CARTESIAN_POINT('Ctrl Pts',(-32.3818671087304,-34.2431869108974,
174.185104246714));
#33894=CARTESIAN_POINT('Ctrl Pts',(-34.0916659602814,-32.8959037429052,
174.073974457495));
#33895=CARTESIAN_POINT('Ctrl Pts',(-33.8871948081556,-30.7286991850778,
173.962844668275));
#33896=CARTESIAN_POINT('Ctrl Pts',(-31.9555834333813,-29.7249753463838,
173.851714879055));
#33897=CARTESIAN_POINT('Ctrl Pts',(-30.0646216186988,-30.8033293990645,
173.740585089835));
#33898=CARTESIAN_POINT('Ctrl Pts',(-29.9448971102786,-32.976863408369,173.629455300616));
#33899=CARTESIAN_POINT('Ctrl Pts',(-31.7059804798686,-34.2563826199768,
173.518325511396));
#33900=CARTESIAN_POINT('Ctrl Pts',(-33.7361473257739,-33.4708849272324,
173.407195722177));
#33901=CARTESIAN_POINT('Ctrl Pts',(-34.1774109668647,-31.3392493001677,
173.296065932957));
#33902=CARTESIAN_POINT('Ctrl Pts',(-32.6259317041196,-29.8123255480467,
173.184936143737));
#33903=CARTESIAN_POINT('Ctrl Pts',(-30.5016065337109,-30.2875377300117,
173.073806354517));
#33904=CARTESIAN_POINT('Ctrl Pts',(-29.7485948142495,-32.3299768105901,
172.962676565298));
#33905=CARTESIAN_POINT('Ctrl Pts',(-31.0560447053144,-34.0704246925659,
172.851546776078));
#33906=CARTESIAN_POINT('Ctrl Pts',(-33.2273922453066,-33.9160423487263,
172.740416986858));
#33907=CARTESIAN_POINT('Ctrl Pts',(-34.2754437129089,-32.0081188259464,
172.629287197638));
#33908=CARTESIAN_POINT('Ctrl Pts',(-33.2410337706164,-30.0927650417054,
172.518157408419));
#33909=CARTESIAN_POINT('Ctrl Pts',(-31.0708431799067,-29.9228920081938,
172.407027619199));
#33910=CARTESIAN_POINT('Ctrl Pts',(-29.7510068346601,-31.6539656834849,
172.295897829979));
#33911=CARTESIAN_POINT('Ctrl Pts',(-30.4894246450174,-33.7017262126649,
172.18476804076));
#33912=CARTESIAN_POINT('Ctrl Pts',(-32.6103046387472,-34.1920853664661,
172.07363825154));
#33913=CARTESIAN_POINT('Ctrl Pts',(-34.1726404455737,-32.6762717650536,
171.96250846232));
#33914=CARTESIAN_POINT('Ctrl Pts',(-33.7465992779157,-30.5415415781258,
171.8513786731));
#33915=CARTESIAN_POINT('Ctrl Pts',(-31.7220893921897,-29.7415767225744,
171.74024888388));
#33916=CARTESIAN_POINT('Ctrl Pts',(-29.9519202809166,-31.0084963589422,
171.629119094661));
#33917=CARTESIAN_POINT('Ctrl Pts',(-30.056131518049,-33.1828293751969,171.517989305441));
#33918=CARTESIAN_POINT('Ctrl Pts',(-31.9393501094869,-34.2746497745218,
171.406859516221));
#33919=CARTESIAN_POINT('Ctrl Pts',(-33.8780748230019,-33.284735367754,171.295729727002));
#33920=CARTESIAN_POINT('Ctrl Pts',(-34.0980058253788,-31.1190450847926,
171.184599937782));
#33921=CARTESIAN_POINT('Ctrl Pts',(-32.3978646482948,-29.7595951866708,
171.073470148562));
#33922=CARTESIAN_POINT('Ctrl Pts',(-30.3336020597539,-30.4505394775294,
170.962340359343));
#33923=CARTESIAN_POINT('Ctrl Pts',(-29.794408794793,-32.5595332353534,170.851210570123));
#33924=CARTESIAN_POINT('Ctrl Pts',(-31.273748682197,-34.1564482440673,170.740080780903));
#33925=CARTESIAN_POINT('Ctrl Pts',(-33.4177458997867,-33.7798052055182,
170.628950991683));
#33926=CARTESIAN_POINT('Ctrl Pts',(-34.2642374447057,-31.7743037440626,
170.517821202464));
#33927=CARTESIAN_POINT('Ctrl Pts',(-33.0385234348626,-29.975357048467,170.406691413244));
#33928=CARTESIAN_POINT('Ctrl Pts',(-30.8623640397511,-30.0293416257758,
170.295561624024));
#33929=CARTESIAN_POINT('Ctrl Pts',(-29.727356738311,-31.8868513762745,170.184431834804));
#33930=CARTESIAN_POINT('Ctrl Pts',(-30.6722479041788,-33.847913520161,170.073302045585));
#33931=CARTESIAN_POINT('Ctrl Pts',(-32.8322833892703,-34.1177852501839,
169.962172256365));
#33932=CARTESIAN_POINT('Ctrl Pts',(-34.2306221422391,-32.4494828856631,
169.851042467145));
#33933=CARTESIAN_POINT('Ctrl Pts',(-33.5875197007206,-30.3698186586225,
169.739912677925));
#33934=CARTESIAN_POINT('Ctrl Pts',(-31.4915364450367,-29.7820787166299,
169.628782888706));
#33935=CARTESIAN_POINT('Ctrl Pts',(-29.8608935207979,-31.2241562808234,
169.517653099486));
#33936=CARTESIAN_POINT('Ctrl Pts',(-30.1879376486804,-33.3762776031315,
169.406523310266));
#33937=CARTESIAN_POINT('Ctrl Pts',(-32.1733615894941,-34.2688445881649,
169.295393521047));
#33938=CARTESIAN_POINT('Ctrl Pts',(-34.0001268836281,-33.0849896107005,
169.184263731827));
#33939=CARTESIAN_POINT('Ctrl Pts',(-33.9963977443443,-30.9081639077541,
169.073133942607));
#33940=CARTESIAN_POINT('Ctrl Pts',(-32.1655870394568,-29.730574755944,168.962004153387));
#33941=CARTESIAN_POINT('Ctrl Pts',(-30.1832328717994,-30.6299389766382,
168.850874364168));
#33942=CARTESIAN_POINT('Ctrl Pts',(-29.8635642778024,-32.7831681881461,
168.739744574948));
#33943=CARTESIAN_POINT('Ctrl Pts',(-31.4991384881812,-34.2196503671186,
168.628614785728));
#33944=CARTESIAN_POINT('Ctrl Pts',(-33.5930957223536,-33.6247326009035,
168.517484996508));
#33945=CARTESIAN_POINT('Ctrl Pts',(-34.2290690282512,-31.5428771784569,
168.406355207289));
#33946=CARTESIAN_POINT('Ctrl Pts',(-32.825022531886,-29.8793756037254,168.295225418069));
#33947=CARTESIAN_POINT('Ctrl Pts',(-30.6659243630751,-30.1566464818375,
168.184095628849));
#33948=CARTESIAN_POINT('Ctrl Pts',(-29.7277577461881,-32.1209345041679,
168.072965839629));
#33949=CARTESIAN_POINT('Ctrl Pts',(-30.8691226057602,-33.9745445904889,
167.96183605041));
#33950=CARTESIAN_POINT('Ctrl Pts',(-33.0454541780027,-34.0210728588022,
167.85070626119));
#33951=CARTESIAN_POINT('Ctrl Pts',(-34.2649974539114,-32.2179372088228,
167.73957647197));
#33952=CARTESIAN_POINT('Ctrl Pts',(-33.4116395620055,-30.2153476982354,
167.628446682751));
#33953=CARTESIAN_POINT('Ctrl Pts',(-31.266364575479,-29.8460528047858,167.517316893531));
#33954=CARTESIAN_POINT('Ctrl Pts',(-29.7925045211951,-31.4480266505451,
167.406187104311));
#33955=CARTESIAN_POINT('Ctrl Pts',(-30.3389209035863,-33.5551612838846,
167.295057315091));
#33956=CARTESIAN_POINT('Ctrl Pts',(-32.4055378153131,-34.2390276195696,
167.183927525872));
#33957=CARTESIAN_POINT('Ctrl Pts',(-34.1010130461478,-32.8737633264784,
167.072797736652));
#33958=CARTESIAN_POINT('Ctrl Pts',(-33.8736595852923,-30.7088338635598,
166.961667947432));
#33959=CARTESIAN_POINT('Ctrl Pts',(-31.9315620200791,-29.7255787770841,
166.850538158213));
#33960=CARTESIAN_POINT('Ctrl Pts',(-30.0520801754102,-30.8238225944352,
166.739408368993));
#33961=CARTESIAN_POINT('Ctrl Pts',(-29.9553500309319,-32.9985456506286,
166.628278579773));
#33962=CARTESIAN_POINT('Ctrl Pts',(-31.7297868433258,-34.2592997290284,
166.517148790554));
#33963=CARTESIAN_POINT('Ctrl Pts',(-33.7516715360443,-33.4525928474522,
166.406019001334));
#33964=CARTESIAN_POINT('Ctrl Pts',(-34.1701365048935,-31.3160292776143,
166.294889212114));
#33965=CARTESIAN_POINT('Ctrl Pts',(-32.603145147106,-29.8063641094246,166.183759422894));
#33966=CARTESIAN_POINT('Ctrl Pts',(-30.4828812072222,-30.3023766555707,
166.072629633674));
#33967=CARTESIAN_POINT('Ctrl Pts',(-29.7537022543286,-32.3559826188516,
165.961499844455));
#33968=CARTESIAN_POINT('Ctrl Pts',(-30.6346957097411,-33.5006534350279,
165.887413318308));
#33969=CARTESIAN_POINT('Ctrl Pts',(-31.2199063053492,-33.7600342388745,
165.850370055235));
#33970=CARTESIAN_POINT('Ctrl Pts',(-32.463299576987,-33.7347832743337,179.149629944765));
#33971=CARTESIAN_POINT('Ctrl Pts',(-33.0401142382023,-33.5807363726286,
179.112586681692));
#33972=CARTESIAN_POINT('Ctrl Pts',(-34.017919885171,-32.653970503011,179.038500155545));
#33973=CARTESIAN_POINT('Ctrl Pts',(-33.6441340634195,-30.6560997447152,
178.927370366326));
#33974=CARTESIAN_POINT('Ctrl Pts',(-31.7626546998272,-29.8914060581426,
178.816240577106));
#33975=CARTESIAN_POINT('Ctrl Pts',(-30.0998488917205,-31.0548970546596,
178.705110787886));
#33976=CARTESIAN_POINT('Ctrl Pts',(-30.1753253823088,-33.0841069177247,
178.593980998666));
#33977=CARTESIAN_POINT('Ctrl Pts',(-31.9210756018475,-34.1207753989353,
178.482851209446));
#33978=CARTESIAN_POINT('Ctrl Pts',(-33.738884034062,-33.2167191131938,178.371721420227));
#33979=CARTESIAN_POINT('Ctrl Pts',(-33.9653693983657,-31.1990433963734,
178.260591631007));
#33980=CARTESIAN_POINT('Ctrl Pts',(-32.3931283817158,-29.9144393156612,
178.149461841787));
#33981=CARTESIAN_POINT('Ctrl Pts',(-30.4611209755161,-30.5384957339954,
178.038332052568));
#33982=CARTESIAN_POINT('Ctrl Pts',(-29.9374689239953,-32.5001158234147,
177.927202263348));
#33983=CARTESIAN_POINT('Ctrl Pts',(-31.3014278771744,-34.0040300224318,
177.816072474128));
#33984=CARTESIAN_POINT('Ctrl Pts',(-33.3047100395391,-33.6738802868631,
177.704942684909));
#33985=CARTESIAN_POINT('Ctrl Pts',(-34.1139369122308,-31.8118121837595,
177.593812895689));
#33986=CARTESIAN_POINT('Ctrl Pts',(-32.9885110633096,-30.1219721586597,
177.482683106469));
#33987=CARTESIAN_POINT('Ctrl Pts',(-30.9584108961468,-30.1508825384663,
177.371553317249));
#33988=CARTESIAN_POINT('Ctrl Pts',(-29.8815616403355,-31.8720853180504,
177.260423528029));
#33989=CARTESIAN_POINT('Ctrl Pts',(-30.743484267,-33.710354152809,177.14929373881));
#33990=CARTESIAN_POINT('Ctrl Pts',(-32.755356432164,-33.9833254515596,177.03816394959));
#33991=CARTESIAN_POINT('Ctrl Pts',(-34.0759345988082,-32.4411787873238,
176.927034160371));
#33992=CARTESIAN_POINT('Ctrl Pts',(-33.4966399249956,-30.4952700901487,
176.815904371151));
#33993=CARTESIAN_POINT('Ctrl Pts',(-31.547636626239,-29.9264738840141,176.704774581931));
#33994=CARTESIAN_POINT('Ctrl Pts',(-30.0126313794938,-31.2553462949064,
176.593644792711));
#33995=CARTESIAN_POINT('Ctrl Pts',(-30.2964443430921,-33.2657177002206,
176.482515003491));
#33996=CARTESIAN_POINT('Ctrl Pts',(-32.1393329691236,-34.1177179929438,
176.371385214272));
#33997=CARTESIAN_POINT('Ctrl Pts',(-33.8547055730506,-33.0316057439677,
176.260255425052));
#33998=CARTESIAN_POINT('Ctrl Pts',(-33.872671749851,-31.0013791055347,176.149125635832));
#33999=CARTESIAN_POINT('Ctrl Pts',(-32.1767890495237,-29.8850794800629,
176.037995846613));
#34000=CARTESIAN_POINT('Ctrl Pts',(-30.319110928242,-30.7043321791094,175.926866057393));
#34001=CARTESIAN_POINT('Ctrl Pts',(-29.9997642569639,-32.7093660168879,
175.815736268173));
#34002=CARTESIAN_POINT('Ctrl Pts',(-31.5110116460523,-34.0651957687719,
175.704606478954));
#34003=CARTESIAN_POINT('Ctrl Pts',(-33.4697758738191,-33.5309807491879,
175.593476689734));
#34004=CARTESIAN_POINT('Ctrl Pts',(-34.0834171609207,-31.5956287507438,
175.482346900514));
#34005=CARTESIAN_POINT('Ctrl Pts',(-32.7903376560667,-30.0303529343944,
175.371217111294));
#34006=CARTESIAN_POINT('Ctrl Pts',(-30.7739496992351,-30.2676767525548,
175.260087322075));
#34007=CARTESIAN_POINT('Ctrl Pts',(-29.8796296817018,-32.0904040205134,
175.148957532855));
#34008=CARTESIAN_POINT('Ctrl Pts',(-30.9258495850164,-33.8303945092891,
175.037827743635));
#34009=CARTESIAN_POINT('Ctrl Pts',(-32.9551202994478,-33.8952277929652,
174.926697954415));
#34010=CARTESIAN_POINT('Ctrl Pts',(-34.1102752736729,-32.2255691534092,
174.815568165196));
#34011=CARTESIAN_POINT('Ctrl Pts',(-33.334129202415,-30.3494720708486,174.704438375976));
#34012=CARTESIAN_POINT('Ctrl Pts',(-31.3370025531356,-29.9839202498175,
174.593308586756));
#34013=CARTESIAN_POINT('Ctrl Pts',(-29.9466439773186,-31.4634627526788,
174.482178797536));
#34014=CARTESIAN_POINT('Ctrl Pts',(-30.4354945657408,-33.4340383257844,
174.371049008317));
#34015=CARTESIAN_POINT('Ctrl Pts',(-32.3561635612421,-34.0921975746302,
174.259919219097));
#34016=CARTESIAN_POINT('Ctrl Pts',(-33.9508755279276,-32.8356002921123,
174.148789429877));
#34017=CARTESIAN_POINT('Ctrl Pts',(-33.7601673678179,-30.8142706839612,
174.037659640658));
#34018=CARTESIAN_POINT('Ctrl Pts',(-31.9585731209015,-29.8781076871497,
173.926529851438));
#34019=CARTESIAN_POINT('Ctrl Pts',(-30.1948923044803,-30.883877524095,173.815400062218));
#34020=CARTESIAN_POINT('Ctrl Pts',(-30.0832264754209,-32.9111105471442,
173.704270272998));
#34021=CARTESIAN_POINT('Ctrl Pts',(-31.725770989513,-34.1045050780296,173.593140483779));
#34022=CARTESIAN_POINT('Ctrl Pts',(-33.619286920113,-33.3718793839095,173.482010694559));
#34023=CARTESIAN_POINT('Ctrl Pts',(-34.0308490218611,-31.3837245550478,
173.370880905339));
#34024=CARTESIAN_POINT('Ctrl Pts',(-32.5838001224424,-29.9595783301775,
173.25975111612));
#34025=CARTESIAN_POINT('Ctrl Pts',(-30.6024636820132,-30.4028038900771,
173.1486213269));
#34026=CARTESIAN_POINT('Ctrl Pts',(-29.9001373241552,-32.3077660089076,
173.03749153768));
#34027=CARTESIAN_POINT('Ctrl Pts',(-31.1195825151679,-33.9310640139692,
172.92636174846));
#34028=CARTESIAN_POINT('Ctrl Pts',(-33.1447762405689,-33.7870731749634,
172.815231959241));
#34029=CARTESIAN_POINT('Ctrl Pts',(-34.1222831651826,-32.0075723462327,
172.704102170021));
#34030=CARTESIAN_POINT('Ctrl Pts',(-33.1574995522237,-30.2211413883485,
172.592972380801));
#34031=CARTESIAN_POINT('Ctrl Pts',(-31.1333849016297,-30.0627025409294,
172.481842591581));
#34032=CARTESIAN_POINT('Ctrl Pts',(-29.9023869910147,-31.6772573189356,
172.370712802361));
#34033=CARTESIAN_POINT('Ctrl Pts',(-30.5911017585573,-33.5871826986533,
172.259583013142));
#34034=CARTESIAN_POINT('Ctrl Pts',(-32.569224917803,-34.0445356848432,172.148453223922));
#34035=CARTESIAN_POINT('Ctrl Pts',(-34.0263996052626,-32.6307517843307,
172.037323434703));
#34036=CARTESIAN_POINT('Ctrl Pts',(-33.6290353493745,-30.6397106910171,
171.926193645483));
#34037=CARTESIAN_POINT('Ctrl Pts',(-31.7407956078916,-29.8935916215613,
171.815063856263));
#34038=CARTESIAN_POINT('Ctrl Pts',(-30.0897769151117,-31.0752346570049,
171.703934067043));
#34039=CARTESIAN_POINT('Ctrl Pts',(-30.1869736741148,-33.1032129056951,
171.592804277824));
#34040=CARTESIAN_POINT('Ctrl Pts',(-31.9434324651163,-34.1215426669389,
171.481674488604));
#34041=CARTESIAN_POINT('Ctrl Pts',(-33.7516612505939,-33.1982595865724,
171.370544699384));
#34042=CARTESIAN_POINT('Ctrl Pts',(-33.9567886555033,-31.1783423271589,
171.259414910164));
#34043=CARTESIAN_POINT('Ctrl Pts',(-32.3710843033854,-29.9103972594232,
171.148285120945));
#34044=CARTESIAN_POINT('Ctrl Pts',(-30.4457676210508,-30.5548339590653,
171.037155331725));
#34045=CARTESIAN_POINT('Ctrl Pts',(-29.9428675569823,-32.5218709471976,
170.926025542505));
#34046=CARTESIAN_POINT('Ctrl Pts',(-31.3226327960912,-34.0112973039095,
170.814895753286));
#34047=CARTESIAN_POINT('Ctrl Pts',(-33.3223171544759,-33.6600061796944,
170.703765964066));
#34048=CARTESIAN_POINT('Ctrl Pts',(-34.1118311930168,-31.7894954018404,
170.592636174846));
#34049=CARTESIAN_POINT('Ctrl Pts',(-32.9686202255643,-30.1116361493947,
170.481506385626));
#34050=CARTESIAN_POINT('Ctrl Pts',(-30.9389385319243,-30.1619870145698,
170.370376596406));
#34051=CARTESIAN_POINT('Ctrl Pts',(-29.8803287871347,-31.8944674315897,
170.259246807187));
#34052=CARTESIAN_POINT('Ctrl Pts',(-30.7616191494823,-33.7235301107657,
170.148117017967));
#34053=CARTESIAN_POINT('Ctrl Pts',(-32.7762622365426,-33.9752367234746,
170.036987228747));
#34054=CARTESIAN_POINT('Ctrl Pts',(-34.0804785429325,-32.4192281074099,
169.925857439528));
#34055=CARTESIAN_POINT('Ctrl Pts',(-33.4806634486809,-30.4795464737831,
169.814727650308));
#34056=CARTESIAN_POINT('Ctrl Pts',(-31.5257612233229,-29.9313674187181,
169.703597861088));
#34057=CARTESIAN_POINT('Ctrl Pts',(-30.0048771834747,-31.2763784686564,
169.592468071869));
#34058=CARTESIAN_POINT('Ctrl Pts',(-30.3099079091038,-33.2836400967308,
169.481338282649));
#34059=CARTESIAN_POINT('Ctrl Pts',(-32.161692588037,-34.1161282287762,169.370208493429));
#34060=CARTESIAN_POINT('Ctrl Pts',(-33.865497963879,-33.0119587542968,169.259078704209));
#34061=CARTESIAN_POINT('Ctrl Pts',(-33.8620198336676,-30.9816556021287,
169.14794891499));
#34062=CARTESIAN_POINT('Ctrl Pts',(-32.1544413444366,-29.8833301993908,
169.03681912577));
#34063=CARTESIAN_POINT('Ctrl Pts',(-30.3055198116467,-30.722158043876,168.92568933655));
#34064=CARTESIAN_POINT('Ctrl Pts',(-30.0073681713189,-32.7304529889181,
168.81455954733));
#34065=CARTESIAN_POINT('Ctrl Pts',(-31.5328515715021,-34.0702452800755,
168.703429758111));
#34066=CARTESIAN_POINT('Ctrl Pts',(-33.4858641472406,-33.5153715414972,
168.592299968891));
#34067=CARTESIAN_POINT('Ctrl Pts',(-34.0790299693416,-31.5736462022427,
168.481170179671));
#34068=CARTESIAN_POINT('Ctrl Pts',(-32.7694901088454,-30.0221152338963,
168.370040390451));
#34069=CARTESIAN_POINT('Ctrl Pts',(-30.7557212471292,-30.2807229566338,
168.258910601232));
#34070=CARTESIAN_POINT('Ctrl Pts',(-29.8807028030956,-32.1127943797639,
168.147780812012));
#34071=CARTESIAN_POINT('Ctrl Pts',(-30.9452421775741,-33.8416376197414,
168.036651022792));
#34072=CARTESIAN_POINT('Ctrl Pts',(-32.9750844590695,-33.885034061493,167.925521233573));
#34073=CARTESIAN_POINT('Ctrl Pts',(-34.1125400458588,-32.2032678139773,
167.814391444353));
#34074=CARTESIAN_POINT('Ctrl Pts',(-33.3166218354486,-30.3354729830266,
167.703261655133));
#34075=CARTESIAN_POINT('Ctrl Pts',(-31.3157457149963,-29.9910353988711,
167.592131865913));
#34076=CARTESIAN_POINT('Ctrl Pts',(-29.9410914604013,-31.4851800813478,
167.481002076694));
#34077=CARTESIAN_POINT('Ctrl Pts',(-30.4507284524965,-33.4504830830171,
167.369872287474));
#34078=CARTESIAN_POINT('Ctrl Pts',(-32.3782409880768,-34.0883182459902,
167.258742498254));
#34079=CARTESIAN_POINT('Ctrl Pts',(-33.9595934596722,-32.8149501513129,
167.147612709035));
#34080=CARTESIAN_POINT('Ctrl Pts',(-33.7475432033717,-30.7957425010009,
167.036482919815));
#34081=CARTESIAN_POINT('Ctrl Pts',(-31.936168593483,-29.8786705008151,166.925353130595));
#34082=CARTESIAN_POINT('Ctrl Pts',(-30.1831950281172,-30.9029913185999,
166.814223341375));
#34083=CARTESIAN_POINT('Ctrl Pts',(-30.0929758080031,-32.9313333535665,
166.703093552156));
#34084=CARTESIAN_POINT('Ctrl Pts',(-31.7479749421323,-34.1072258359179,
166.591963762936));
#34085=CARTESIAN_POINT('Ctrl Pts',(-33.6337661928468,-33.3548185474873,
166.480833973716));
#34086=CARTESIAN_POINT('Ctrl Pts',(-34.0240642053043,-31.3620674766148,
166.369704184496));
#34087=CARTESIAN_POINT('Ctrl Pts',(-32.5625473329016,-29.9540181571193,
166.258574395277));
#34088=CARTESIAN_POINT('Ctrl Pts',(-30.5849987608006,-30.4166440047433,
166.147444606057));
#34089=CARTESIAN_POINT('Ctrl Pts',(-29.9049009814742,-32.3320213612846,
166.036314816837));
#34090=CARTESIAN_POINT('Ctrl Pts',(-30.7265946003719,-33.3996441678013,
165.962228290691));
#34091=CARTESIAN_POINT('Ctrl Pts',(-31.2724145598372,-33.6415660005639,
165.925185027618));
#34092=CARTESIAN_POINT('Ctrl Pts',(-32.4298642568861,-33.6095877486648,
179.224444917147));
#34093=CARTESIAN_POINT('Ctrl Pts',(-32.965051461927,-33.4666580759081,179.187401654074));
#34094=CARTESIAN_POINT('Ctrl Pts',(-33.8722910077662,-32.6067748779967,
179.113315127928));
#34095=CARTESIAN_POINT('Ctrl Pts',(-33.5254804936132,-30.7530860953427,
179.002185338708));
#34096=CARTESIAN_POINT('Ctrl Pts',(-31.7797833925347,-30.0435786844751,
178.891055549488));
#34097=CARTESIAN_POINT('Ctrl Pts',(-30.2369786533288,-31.1231030731311,
178.779925760269));
#34098=CARTESIAN_POINT('Ctrl Pts',(-30.3070081701916,-33.0058692857081,
178.668795971049));
#34099=CARTESIAN_POINT('Ctrl Pts',(-31.9267714035427,-33.9677236634109,
178.557666181829));
#34100=CARTESIAN_POINT('Ctrl Pts',(-33.6133925655065,-33.1289111482327,
178.446536392609));
#34101=CARTESIAN_POINT('Ctrl Pts',(-33.8235329749908,-31.2568466877197,
178.33540660339));
#34102=CARTESIAN_POINT('Ctrl Pts',(-32.3647571637473,-30.0649496820299,
178.22427681417));
#34103=CARTESIAN_POINT('Ctrl Pts',(-30.5721785187041,-30.643969309604,178.11314702495));
#34104=CARTESIAN_POINT('Ctrl Pts',(-30.0863172937539,-32.4640235550984,
178.00201723573));
#34105=CARTESIAN_POINT('Ctrl Pts',(-31.3518423038228,-33.8594035461297,
177.890887446511));
#34106=CARTESIAN_POINT('Ctrl Pts',(-33.2105519613155,-33.5530799969818,
177.779757657291));
#34107=CARTESIAN_POINT('Ctrl Pts',(-33.9613786953784,-31.8253932880549,
177.668627868071));
#34108=CARTESIAN_POINT('Ctrl Pts',(-32.9171723756293,-30.2575053323397,
177.557498078851));
#34109=CARTESIAN_POINT('Ctrl Pts',(-31.0335801102598,-30.2843293130839,
177.446368289632));
#34110=CARTESIAN_POINT('Ctrl Pts',(-30.0344447168324,-31.8813166416885,
177.335238500412));
#34111=CARTESIAN_POINT('Ctrl Pts',(-30.8341642672234,-33.5869216235651,
177.224108711192));
#34112=CARTESIAN_POINT('Ctrl Pts',(-32.7008440057466,-33.8401931789845,
177.112978921973));
#34113=CARTESIAN_POINT('Ctrl Pts',(-33.9261189260395,-32.4093398763715,
177.001849132753));
#34114=CARTESIAN_POINT('Ctrl Pts',(-33.388630685502,-30.6038631662066,176.890719343533));
#34115=CARTESIAN_POINT('Ctrl Pts',(-31.5802827044029,-30.0761157418299,
176.779589554313));
#34116=CARTESIAN_POINT('Ctrl Pts',(-30.1560554387543,-31.3090863288518,
176.668459765094));
#34117=CARTESIAN_POINT('Ctrl Pts',(-30.4193862397131,-33.1743736140907,
176.557329975874));
#34118=CARTESIAN_POINT('Ctrl Pts',(-32.1292776126013,-33.9648869037422,
176.446200186654));
#34119=CARTESIAN_POINT('Ctrl Pts',(-33.7208555166115,-32.9571570071658,
176.335070397434));
#34120=CARTESIAN_POINT('Ctrl Pts',(-33.7375251136131,-31.0734473976818,
176.223940608215));
#34121=CARTESIAN_POINT('Ctrl Pts',(-32.1640305693636,-30.0377086817384,
176.112810818995));
#34122=CARTESIAN_POINT('Ctrl Pts',(-30.4404170268443,-30.7978377001325,
176.001681029775));
#34123=CARTESIAN_POINT('Ctrl Pts',(-30.1441169083966,-32.6581726184444,
175.890551240556));
#34124=CARTESIAN_POINT('Ctrl Pts',(-31.5463008691641,-33.9161550939476,
175.779421451336));
#34125=CARTESIAN_POINT('Ctrl Pts',(-33.3637053543134,-33.4204932073033,
175.668291662116));
#34126=CARTESIAN_POINT('Ctrl Pts',(-33.9330614879624,-31.6248113419441,
175.557161872897));
#34127=CARTESIAN_POINT('Ctrl Pts',(-32.7333007110078,-30.1724980676852,
175.446032083677));
#34128=CARTESIAN_POINT('Ctrl Pts',(-30.8624310756536,-30.3926947434481,
175.334902294457));
#34129=CARTESIAN_POINT('Ctrl Pts',(-30.0326521834401,-32.0838797595073,
175.223772505237));
#34130=CARTESIAN_POINT('Ctrl Pts',(-31.0033686779435,-33.6982989293037,
175.112642716018));
#34131=CARTESIAN_POINT('Ctrl Pts',(-32.8861913503764,-33.7584533362862,
175.001512926798));
#34132=CARTESIAN_POINT('Ctrl Pts',(-33.9579813092899,-32.209290319532,174.890383137578));
#34133=CARTESIAN_POINT('Ctrl Pts',(-33.2378480073643,-30.4685870720011,
174.779253348358));
#34134=CARTESIAN_POINT('Ctrl Pts',(-31.3848496330017,-30.1294163286931,
174.668123559139));
#34135=CARTESIAN_POINT('Ctrl Pts',(-30.0948302034879,-31.50218347573,174.556993769919));
#34136=CARTESIAN_POINT('Ctrl Pts',(-30.5484015110359,-33.3305469071834,
174.445863980699));
#34137=CARTESIAN_POINT('Ctrl Pts',(-32.3304600137538,-33.9412082383629,
174.33473419148));
#34138=CARTESIAN_POINT('Ctrl Pts',(-33.8100850955738,-32.7752968413194,
174.22360440226));
#34139=CARTESIAN_POINT('Ctrl Pts',(-33.6331399274802,-30.8998421828445,
174.11247461304));
#34140=CARTESIAN_POINT('Ctrl Pts',(-31.9615628084217,-30.0312400279156,
174.00134482382));
#34141=CARTESIAN_POINT('Ctrl Pts',(-30.3251629902618,-30.9644256491254,
173.890215034601));
#34142=CARTESIAN_POINT('Ctrl Pts',(-30.2215558405631,-32.8453576859195,
173.779085245381));
#34143=CARTESIAN_POINT('Ctrl Pts',(-31.7455614991574,-33.9526275360824,
173.667955456161));
#34144=CARTESIAN_POINT('Ctrl Pts',(-33.5024265144521,-33.2728738405865,
173.556825666942));
#34145=CARTESIAN_POINT('Ctrl Pts',(-33.8842870768574,-31.4281998099279,
173.445695877722));
#34146=CARTESIAN_POINT('Ctrl Pts',(-32.5416685407652,-30.1068311123084,
173.334566088502));
#34147=CARTESIAN_POINT('Ctrl Pts',(-30.7033208303155,-30.5180700501426,
173.223436299282));
#34148=CARTESIAN_POINT('Ctrl Pts',(-30.0516798340609,-32.2855552072252,
173.112306510062));
#34149=CARTESIAN_POINT('Ctrl Pts',(-31.1831203250215,-33.7917033353726,
173.001176720843));
#34150=CARTESIAN_POINT('Ctrl Pts',(-33.0621602358311,-33.6581040012006,
172.890046931623));
#34151=CARTESIAN_POINT('Ctrl Pts',(-33.9691226174563,-32.007025866519,172.778917142403));
#34152=CARTESIAN_POINT('Ctrl Pts',(-33.073965333831,-30.3495177349915,172.667787353183));
#34153=CARTESIAN_POINT('Ctrl Pts',(-31.1959266233527,-30.202513073665,172.556657563964));
#34154=CARTESIAN_POINT('Ctrl Pts',(-30.0537671473693,-31.7005489543862,
172.445527774744));
#34155=CARTESIAN_POINT('Ctrl Pts',(-30.6927788720971,-33.4726391846419,
172.334397985525));
#34156=CARTESIAN_POINT('Ctrl Pts',(-32.5281451968589,-33.8969860032201,
172.223268196305));
#34157=CARTESIAN_POINT('Ctrl Pts',(-33.8801587649515,-32.585231803608,172.112138407085));
#34158=CARTESIAN_POINT('Ctrl Pts',(-33.5114714208333,-30.7378798039084,
172.001008617865));
#34159=CARTESIAN_POINT('Ctrl Pts',(-31.7595018235935,-30.0456065205483,
171.889878828645));
#34160=CARTESIAN_POINT('Ctrl Pts',(-30.2276335493068,-31.1419729550677,
171.778749039426));
#34161=CARTESIAN_POINT('Ctrl Pts',(-30.3178158301807,-33.0235964361933,
171.667619250206));
#34162=CARTESIAN_POINT('Ctrl Pts',(-31.9475148207455,-33.9684355593559,
171.556489460986));
#34163=CARTESIAN_POINT('Ctrl Pts',(-33.625247678186,-33.1117838053908,171.445359671767));
#34164=CARTESIAN_POINT('Ctrl Pts',(-33.8155714856278,-31.2376395695253,
171.334229882547));
#34165=CARTESIAN_POINT('Ctrl Pts',(-32.3443039584759,-30.0611993321757,
171.223100093327));
#34166=CARTESIAN_POINT('Ctrl Pts',(-30.5579331823478,-30.6591284406011,
171.111970304108));
#34167=CARTESIAN_POINT('Ctrl Pts',(-30.0913263191716,-32.4842086590419,
171.000840514888));
#34168=CARTESIAN_POINT('Ctrl Pts',(-31.3715169099854,-33.8661463637517,
170.889710725668));
#34169=CARTESIAN_POINT('Ctrl Pts',(-33.2268884091652,-33.5402071538707,
170.778580936448));
#34170=CARTESIAN_POINT('Ctrl Pts',(-33.9594249413278,-31.8046870596182,
170.667451147228));
#34171=CARTESIAN_POINT('Ctrl Pts',(-32.8987170162659,-30.2479152503225,
170.556321358009));
#34172=CARTESIAN_POINT('Ctrl Pts',(-31.0155130240976,-30.2946324033638,
170.445191568789));
#34173=CARTESIAN_POINT('Ctrl Pts',(-30.0333008359585,-31.902083486905,170.334061779569));
#34174=CARTESIAN_POINT('Ctrl Pts',(-30.8509903947858,-33.5991467013704,
170.22293199035));
#34175=CARTESIAN_POINT('Ctrl Pts',(-32.7202410838149,-33.8326881967655,
170.11180220113));
#34176=CARTESIAN_POINT('Ctrl Pts',(-33.9303349436258,-32.3889733291566,
170.00067241191));
#34177=CARTESIAN_POINT('Ctrl Pts',(-33.3738071966412,-30.5892742889438,
169.88954262269));
#34178=CARTESIAN_POINT('Ctrl Pts',(-31.5599860016091,-30.0806561208062,
169.778412833471));
#34179=CARTESIAN_POINT('Ctrl Pts',(-30.1488608461515,-31.3286006564895,
169.667283044251));
#34180=CARTESIAN_POINT('Ctrl Pts',(-30.4318781695273,-33.1910025903301,
169.556153255031));
#34181=CARTESIAN_POINT('Ctrl Pts',(-32.1500235865798,-33.9634118693876,
169.445023465812));
#34182=CARTESIAN_POINT('Ctrl Pts',(-33.7308690441301,-32.938927897893,169.333893676592));
#34183=CARTESIAN_POINT('Ctrl Pts',(-33.7276419229907,-31.0551472965034,
169.222763887372));
#34184=CARTESIAN_POINT('Ctrl Pts',(-32.1432956494165,-30.0360856428375,
169.111634098152));
#34185=CARTESIAN_POINT('Ctrl Pts',(-30.427806751494,-30.8143771111138,169.000504308933));
#34186=CARTESIAN_POINT('Ctrl Pts',(-30.1511720648354,-32.6777377896899,
168.889374519713));
#34187=CARTESIAN_POINT('Ctrl Pts',(-31.5665646548229,-33.9208401930324,
168.778244730493));
#34188=CARTESIAN_POINT('Ctrl Pts',(-33.3786325721277,-33.4060104820908,
168.667114941273));
#34189=CARTESIAN_POINT('Ctrl Pts',(-33.9289909104319,-31.6044152260286,
168.555985152054));
#34190=CARTESIAN_POINT('Ctrl Pts',(-32.7139576858049,-30.1648548640671,
168.444855362834));
#34191=CARTESIAN_POINT('Ctrl Pts',(-30.8455181311833,-30.4047994314301,
168.333725573614));
#34192=CARTESIAN_POINT('Ctrl Pts',(-30.0336478600031,-32.1046542553599,
168.222595784394));
#34193=CARTESIAN_POINT('Ctrl Pts',(-31.0213617493879,-33.7087306489938,
168.111465995175));
#34194=CARTESIAN_POINT('Ctrl Pts',(-32.9047147401363,-33.7489952641838,
168.000336205955));
#34195=CARTESIAN_POINT('Ctrl Pts',(-33.9600826378061,-32.1885984191319,
167.889206416735));
#34196=CARTESIAN_POINT('Ctrl Pts',(-33.2216041088917,-30.4555982678176,
167.778076627516));
#34197=CARTESIAN_POINT('Ctrl Pts',(-31.3651268545137,-30.1360179929564,
167.666946838296));
#34198=CARTESIAN_POINT('Ctrl Pts',(-30.0896783996075,-31.5223335121504,
167.555817049076));
#34199=CARTESIAN_POINT('Ctrl Pts',(-30.5625360014067,-33.3458048821496,
167.444687259856));
#34200=CARTESIAN_POINT('Ctrl Pts',(-32.3509441608406,-33.9376088724108,
167.333557470637));
#34201=CARTESIAN_POINT('Ctrl Pts',(-33.8181738731966,-32.7561369761474,
167.222427681417));
#34202=CARTESIAN_POINT('Ctrl Pts',(-33.6214268214511,-30.8826511384421,
167.111297892197));
#34203=CARTESIAN_POINT('Ctrl Pts',(-31.9407751668869,-30.0317622245461,
167.000168102978));
#34204=CARTESIAN_POINT('Ctrl Pts',(-30.3143098808242,-30.9821600427646,
166.889038313758));
#34205=CARTESIAN_POINT('Ctrl Pts',(-30.2306015850745,-32.8641210565045,
166.777908524538));
#34206=CARTESIAN_POINT('Ctrl Pts',(-31.7661630409388,-33.9551519428074,
166.666778735318));
#34207=CARTESIAN_POINT('Ctrl Pts',(-33.5158608496493,-33.2570442475225,
166.555648946099));
#34208=CARTESIAN_POINT('Ctrl Pts',(-33.8779919057151,-31.4081056756153,
166.444519156879));
#34209=CARTESIAN_POINT('Ctrl Pts',(-32.5219495186972,-30.1016722048141,
166.333389367659));
#34210=CARTESIAN_POINT('Ctrl Pts',(-30.6871163143791,-30.5309113539161,
166.222259578439));
#34211=CARTESIAN_POINT('Ctrl Pts',(-30.0560997086199,-32.3080601037175,
166.11112978922));
#34212=CARTESIAN_POINT('Ctrl Pts',(-30.8184934910027,-33.2986349005748,
166.037043263073));
#34213=CARTESIAN_POINT('Ctrl Pts',(-31.3249228143252,-33.5230977622534,
166.));
#34214=CARTESIAN_POINT('Ctrl Pts',(-33.6638666881858,-31.9990537019747,
178.37851963661));
#34215=CARTESIAN_POINT('Ctrl Pts',(-33.6649866280482,-31.7834929812639,
178.364148625536));
#34216=CARTESIAN_POINT('Ctrl Pts',(-33.6261153890564,-31.5683196357392,
178.349777614463));
#34217=CARTESIAN_POINT('Ctrl Pts',(-33.5453802715361,-31.3702079301903,
178.33540660339));
#34218=CARTESIAN_POINT('Ctrl Pts',(-33.3372743712429,-30.8595476858231,
178.298363340316));
#34219=CARTESIAN_POINT('Ctrl Pts',(-32.8510157674951,-30.4622486839265,
178.261320077243));
#34220=CARTESIAN_POINT('Ctrl Pts',(-32.309123358114,-30.3601024542406,178.22427681417));
#34221=CARTESIAN_POINT('Ctrl Pts',(-31.7672309487329,-30.2579562245546,
178.187233551097));
#34222=CARTESIAN_POINT('Ctrl Pts',(-31.1697047337185,-30.4509627670793,
178.150190288024));
#34223=CARTESIAN_POINT('Ctrl Pts',(-30.7899647553863,-30.8508084125907,
178.11314702495));
#34224=CARTESIAN_POINT('Ctrl Pts',(-30.410224777054,-31.2506540581021,178.076103761877));
#34225=CARTESIAN_POINT('Ctrl Pts',(-30.2482710354039,-31.8573388066003,
178.039060498804));
#34226=CARTESIAN_POINT('Ctrl Pts',(-30.3782149995904,-32.3932445126879,
178.002017235731));
#34227=CARTESIAN_POINT('Ctrl Pts',(-30.5081589637769,-32.9291502187755,
177.964973972657));
#34228=CARTESIAN_POINT('Ctrl Pts',(-30.9300006337998,-33.3942768824526,
177.927930709584));
#34229=CARTESIAN_POINT('Ctrl Pts',(-31.4507064117268,-33.5757862894332,
177.890887446511));
#34230=CARTESIAN_POINT('Ctrl Pts',(-31.9714121896537,-33.7572956964137,
177.853844183438));
#34231=CARTESIAN_POINT('Ctrl Pts',(-32.5909820754846,-33.6551878466978,
177.816800920364));
#34232=CARTESIAN_POINT('Ctrl Pts',(-33.0259048074106,-33.3161861370186,
177.779757657291));
#34233=CARTESIAN_POINT('Ctrl Pts',(-33.4221146521209,-33.0073592928715,
177.746011650397));
#34234=CARTESIAN_POINT('Ctrl Pts',(-33.6650856313621,-32.5019339874448,
177.712265643504));
#34235=CARTESIAN_POINT('Ctrl Pts',(-33.6682333060465,-31.9991447275653,
177.67851963661));
#34236=CARTESIAN_POINT('Ctrl Pts',(-32.5301702171889,-33.9851743256717,
179.));
#34237=CARTESIAN_POINT('Ctrl Pts',(-32.5988282168344,-33.9597528138625,
179.));
#34238=CARTESIAN_POINT('Ctrl Pts',(-32.6657829343011,-33.9304405480476,
179.));
#34239=CARTESIAN_POINT('Ctrl Pts',(-32.7308455531179,-33.8975318719722,
179.));
#34240=CARTESIAN_POINT('Ctrl Pts',(-32.7977248428542,-33.8637043236487,
179.));
#34241=CARTESIAN_POINT('Ctrl Pts',(-32.8626056686009,-33.8260760354227,
179.));
#34242=CARTESIAN_POINT('Ctrl Pts',(-32.9252517375558,-33.7849220422036,
179.));
#34243=CARTESIAN_POINT('Ctrl Pts',(-32.9781830025095,-33.7501499813973,
179.));
#34244=CARTESIAN_POINT('Ctrl Pts',(-33.0295185420485,-33.7128598710975,
179.));
#34245=CARTESIAN_POINT('Ctrl Pts',(-33.0790930888641,-33.6731995961689,
179.));
#34246=CARTESIAN_POINT('Ctrl Pts',(-33.1011284696503,-33.6555710081884,
179.));
#34247=CARTESIAN_POINT('Ctrl Pts',(-33.1228156256912,-33.6374739649692,
179.));
#34248=CARTESIAN_POINT('Ctrl Pts',(-33.1441384887267,-33.6189207291506,
179.));
#34249=CARTESIAN_POINT('Ctrl Pts',(-33.1558499891621,-33.6087304358017,
179.));
#34250=CARTESIAN_POINT('Ctrl Pts',(-33.1674515751521,-33.5984025156165,
179.));
#34251=CARTESIAN_POINT('Ctrl Pts',(-33.1789404500937,-33.5879389587906,
179.));
#34252=CARTESIAN_POINT('Ctrl Pts',(-33.1895353200388,-33.5782896219933,
179.));
#34253=CARTESIAN_POINT('Ctrl Pts',(-33.2000357743432,-33.568523417913,179.));
#34254=CARTESIAN_POINT('Ctrl Pts',(-33.2104237260108,-33.5586573714086,
179.));
#34255=CARTESIAN_POINT('Ctrl Pts',(-33.2635074325071,-33.5082406642775,
179.));
#34256=CARTESIAN_POINT('Ctrl Pts',(-33.3137511044884,-33.4551351988,179.));
#34257=CARTESIAN_POINT('Ctrl Pts',(-33.3609361378531,-33.3996008414489,
179.));
#34258=CARTESIAN_POINT('Ctrl Pts',(-33.4077563290928,-33.3444958845135,
179.));
#34259=CARTESIAN_POINT('Ctrl Pts',(-33.4515655070966,-33.2869985673899,
179.));
#34260=CARTESIAN_POINT('Ctrl Pts',(-33.4921053042421,-33.2273385372884,
179.));
#34261=CARTESIAN_POINT('Ctrl Pts',(-33.5257899646654,-33.1777668078692,
179.));
#34262=CARTESIAN_POINT('Ctrl Pts',(-33.5572167980499,-33.1267012881111,
179.));
#34263=CARTESIAN_POINT('Ctrl Pts',(-33.586209996391,-33.0742672521662,179.));
#34264=CARTESIAN_POINT('Ctrl Pts',(-33.5983166726236,-33.0523723963699,
179.));
#34265=CARTESIAN_POINT('Ctrl Pts',(-33.6099986880749,-33.0302388812303,
179.));
#34266=CARTESIAN_POINT('Ctrl Pts',(-33.6212418007289,-33.0078757455458,
179.));
#34267=CARTESIAN_POINT('Ctrl Pts',(-33.6264400400048,-32.9975361773298,
179.));
#34268=CARTESIAN_POINT('Ctrl Pts',(-33.6315444442265,-32.9871475240125,
179.));
#34269=CARTESIAN_POINT('Ctrl Pts',(-33.6365535406754,-32.9767106809501,
179.));
#34270=CARTESIAN_POINT('Ctrl Pts',(-33.6417882346349,-32.965803787882,179.));
#34271=CARTESIAN_POINT('Ctrl Pts',(-33.646915240041,-32.9548517050336,179.));
#34272=CARTESIAN_POINT('Ctrl Pts',(-33.6519314793551,-32.9438597806135,
179.));
#34273=CARTESIAN_POINT('Ctrl Pts',(-33.6804723551455,-32.8813190743342,
179.));
#34274=CARTESIAN_POINT('Ctrl Pts',(-33.7054522044227,-32.8174462149676,
179.));
#34275=CARTESIAN_POINT('Ctrl Pts',(-33.726647601974,-32.752446031535,179.));
#34276=CARTESIAN_POINT('Ctrl Pts',(-33.7458438908687,-32.6935765389313,
179.));
#34277=CARTESIAN_POINT('Ctrl Pts',(-33.7619356221037,-32.633781749793,179.));
#34278=CARTESIAN_POINT('Ctrl Pts',(-33.7747201576386,-32.5732090252637,
179.));
#34279=CARTESIAN_POINT('Ctrl Pts',(-33.7898548837777,-32.5015011720726,
179.));
#34280=CARTESIAN_POINT('Ctrl Pts',(-33.800355329414,-32.4287015605003,179.));
#34281=CARTESIAN_POINT('Ctrl Pts',(-33.8062965446138,-32.355232863435,179.));
#34282=CARTESIAN_POINT('Ctrl Pts',(-33.8076038423758,-32.3390669007456,
179.));
#34283=CARTESIAN_POINT('Ctrl Pts',(-33.8086901718668,-32.3228686246414,
179.));
#34284=CARTESIAN_POINT('Ctrl Pts',(-33.8095559636441,-32.3066427023709,
179.));
#34285=CARTESIAN_POINT('Ctrl Pts',(-33.8104538965015,-32.2898144197184,
179.));
#34286=CARTESIAN_POINT('Ctrl Pts',(-33.8111146239095,-32.2729501736476,
179.));
#34287=CARTESIAN_POINT('Ctrl Pts',(-33.8115380624634,-32.2560895659403,
179.));
#34288=CARTESIAN_POINT('Ctrl Pts',(-33.8132597908656,-32.1875332502793,
179.));
#34289=CARTESIAN_POINT('Ctrl Pts',(-33.8110702051067,-32.1189505986289,
179.));
#34290=CARTESIAN_POINT('Ctrl Pts',(-33.8050897978935,-32.0506795924014,
179.));
#34291=CARTESIAN_POINT('Ctrl Pts',(-33.7991106060521,-31.9824224605892,
179.));
#34292=CARTESIAN_POINT('Ctrl Pts',(-33.7893416799664,-31.9144757768024,
179.));
#34293=CARTESIAN_POINT('Ctrl Pts',(-33.775853835733,-31.8471923584511,179.));
#34294=CARTESIAN_POINT('Ctrl Pts',(-33.7660958992626,-31.7985153934433,
179.));
#34295=CARTESIAN_POINT('Ctrl Pts',(-33.7543904437871,-31.7501858451891,
179.));
#34296=CARTESIAN_POINT('Ctrl Pts',(-33.7407500867331,-31.7023469553251,
179.));
#34297=CARTESIAN_POINT('Ctrl Pts',(-33.7305145998785,-31.6664494838438,
179.));
#34298=CARTESIAN_POINT('Ctrl Pts',(-33.7191893710348,-31.6308284441348,
179.));
#34299=CARTESIAN_POINT('Ctrl Pts',(-33.706775815965,-31.595548533918,179.));
#34300=CARTESIAN_POINT('Ctrl Pts',(-33.7026466613343,-31.5838132812991,
179.));
#34301=CARTESIAN_POINT('Ctrl Pts',(-33.6984002845091,-31.5721249678948,
179.));
#34302=CARTESIAN_POINT('Ctrl Pts',(-33.6940373283514,-31.560486148014,179.));
#34303=CARTESIAN_POINT('Ctrl Pts',(-33.6709143145649,-31.4988021468828,
179.));
#34304=CARTESIAN_POINT('Ctrl Pts',(-33.6445184276946,-31.4385017846299,
179.));
#34305=CARTESIAN_POINT('Ctrl Pts',(-33.6148995884413,-31.3799188808691,
179.));
#34306=CARTESIAN_POINT('Ctrl Pts',(-33.5940729902705,-31.3387260918518,
179.));
#34307=CARTESIAN_POINT('Ctrl Pts',(-33.5716520282499,-31.2983829870109,
179.));
#34308=CARTESIAN_POINT('Ctrl Pts',(-33.5476436633208,-31.2590169558985,
179.));
#34309=CARTESIAN_POINT('Ctrl Pts',(-33.5399305936275,-31.2463699912919,
179.));
#34310=CARTESIAN_POINT('Ctrl Pts',(-33.5320525316577,-31.2338222713431,
179.));
#34311=CARTESIAN_POINT('Ctrl Pts',(-33.524013020168,-31.2213836352321,179.));
#34312=CARTESIAN_POINT('Ctrl Pts',(-33.4897680757568,-31.1684002664396,
179.));
#34313=CARTESIAN_POINT('Ctrl Pts',(-33.4526667826938,-31.1175003544769,
179.));
#34314=CARTESIAN_POINT('Ctrl Pts',(-33.4127433144394,-31.0689988956573,
179.));
#34315=CARTESIAN_POINT('Ctrl Pts',(-33.3759774110677,-31.0243334388139,
179.));
#34316=CARTESIAN_POINT('Ctrl Pts',(-33.336817505376,-30.9817019587916,179.));
#34317=CARTESIAN_POINT('Ctrl Pts',(-33.2952688824592,-30.9413832873573,
179.));
#34318=CARTESIAN_POINT('Ctrl Pts',(-33.2874271850203,-30.933773725347,179.));
#34319=CARTESIAN_POINT('Ctrl Pts',(-33.2795003456115,-30.9262466517635,
179.));
#34320=CARTESIAN_POINT('Ctrl Pts',(-33.2714899711316,-30.9188027398162,
179.));
#34321=CARTESIAN_POINT('Origin',(-32.,-32.,172.));
#34322=CARTESIAN_POINT('Origin',(-32.,32.,166.));
#34323=CARTESIAN_POINT('Ctrl Pts',(-31.3249228143257,30.4769022377464,166.));
#34324=CARTESIAN_POINT('Ctrl Pts',(-31.2652496529217,30.4954852962336,166.));
#34325=CARTESIAN_POINT('Ctrl Pts',(-31.2068892521994,30.5176437837123,166.));
#34326=CARTESIAN_POINT('Ctrl Pts',(-31.149997930983,30.543078521238,166.));
#34327=CARTESIAN_POINT('Ctrl Pts',(-31.1139308250343,30.5592032543871,166.));
#34328=CARTESIAN_POINT('Ctrl Pts',(-31.0784541088344,30.57664585217,166.));
#34329=CARTESIAN_POINT('Ctrl Pts',(-31.0436085110974,30.5953405136239,166.));
#34330=CARTESIAN_POINT('Ctrl Pts',(-31.0200367372352,30.6079867691293,166.));
#34331=CARTESIAN_POINT('Ctrl Pts',(-30.9967537833441,30.6212061370888,166.));
#34332=CARTESIAN_POINT('Ctrl Pts',(-30.9737727083008,30.6349801542912,166.));
#34333=CARTESIAN_POINT('Ctrl Pts',(-30.9613018107735,30.6424547548808,166.));
#34334=CARTESIAN_POINT('Ctrl Pts',(-30.9489197191831,30.6500929212155,166.));
#34335=CARTESIAN_POINT('Ctrl Pts',(-30.9366411005164,30.6578835033087,166.));
#34336=CARTESIAN_POINT('Ctrl Pts',(-30.8809433698913,30.6932227995781,166.));
#34337=CARTESIAN_POINT('Ctrl Pts',(-30.8273088794392,30.7317322690669,166.));
#34338=CARTESIAN_POINT('Ctrl Pts',(-30.7759191889064,30.7731089876249,166.));
#34339=CARTESIAN_POINT('Ctrl Pts',(-30.7388357321088,30.8029669560067,166.));
#34340=CARTESIAN_POINT('Ctrl Pts',(-30.7029212833327,30.8343191918032,166.));
#34341=CARTESIAN_POINT('Ctrl Pts',(-30.6682493534813,30.8670677622712,166.));
#34342=CARTESIAN_POINT('Ctrl Pts',(-30.6588706375682,30.8759262117518,166.));
#34343=CARTESIAN_POINT('Ctrl Pts',(-30.6495828699885,30.884886899106,166.));
#34344=CARTESIAN_POINT('Ctrl Pts',(-30.6403875871116,30.893948033715,166.));
#34345=CARTESIAN_POINT('Ctrl Pts',(-30.6306791049162,30.9035148806733,166.));
#34346=CARTESIAN_POINT('Ctrl Pts',(-30.6210791487639,30.9131884173309,166.));
#34347=CARTESIAN_POINT('Ctrl Pts',(-30.611593764049,30.9229613523084,166.));
#34348=CARTESIAN_POINT('Ctrl Pts',(-30.5643377407046,30.9716499461109,166.));
#34349=CARTESIAN_POINT('Ctrl Pts',(-30.5198879151527,31.0228371550682,166.));
#34350=CARTESIAN_POINT('Ctrl Pts',(-30.4784277579538,31.0762154699866,166.));
#34351=CARTESIAN_POINT('Ctrl Pts',(-30.4363631767253,31.1303719569714,166.));
#34352=CARTESIAN_POINT('Ctrl Pts',(-30.3973751779897,31.1867844829168,166.));
#34353=CARTESIAN_POINT('Ctrl Pts',(-30.3616797296655,31.2451788214444,166.));
#34354=CARTESIAN_POINT('Ctrl Pts',(-30.3395644350503,31.2813573276974,166.));
#34355=CARTESIAN_POINT('Ctrl Pts',(-30.3187135104441,31.3182974422918,166.));
#34356=CARTESIAN_POINT('Ctrl Pts',(-30.299185233179,31.3559412292716,166.));
#34357=CARTESIAN_POINT('Ctrl Pts',(-30.2832061926244,31.3867433113299,166.));
#34358=CARTESIAN_POINT('Ctrl Pts',(-30.2681127925988,31.4180166428631,166.));
#34359=CARTESIAN_POINT('Ctrl Pts',(-30.2539402801135,31.4497316930281,166.));
#34360=CARTESIAN_POINT('Ctrl Pts',(-30.2481176636228,31.4627614627521,166.));
#34361=CARTESIAN_POINT('Ctrl Pts',(-30.2424496090511,31.475868333721,166.));
#34362=CARTESIAN_POINT('Ctrl Pts',(-30.2369477740253,31.4890276669845,166.));
#34363=CARTESIAN_POINT('Ctrl Pts',(-30.2097572377756,31.5540622102674,166.));
#34364=CARTESIAN_POINT('Ctrl Pts',(-30.1865718180333,31.6204869404992,166.));
#34365=CARTESIAN_POINT('Ctrl Pts',(-30.167602913195,31.6880061970132,166.));
#34366=CARTESIAN_POINT('Ctrl Pts',(-30.1654997751652,31.6954922547127,166.));
#34367=CARTESIAN_POINT('Ctrl Pts',(-30.1634485057444,31.7029918059433,166.));
#34368=CARTESIAN_POINT('Ctrl Pts',(-30.1614494212112,31.7105044754886,166.));
#34369=CARTESIAN_POINT('Ctrl Pts',(-30.1441093782497,31.7756693099455,166.));
#34370=CARTESIAN_POINT('Ctrl Pts',(-30.1306917361854,31.8418190894582,166.));
#34371=CARTESIAN_POINT('Ctrl Pts',(-30.121042543408,31.908649652992,166.));
#34372=CARTESIAN_POINT('Ctrl Pts',(-30.1106635819057,31.980534613952,166.));
#34373=CARTESIAN_POINT('Ctrl Pts',(-30.104644022139,32.0532080204044,166.));
#34374=CARTESIAN_POINT('Ctrl Pts',(-30.102852408182,32.1263138620071,166.));
#34375=CARTESIAN_POINT('Ctrl Pts',(-30.1025311237508,32.1394237000121,166.));
#34376=CARTESIAN_POINT('Ctrl Pts',(-30.1023459616189,32.1525474788775,166.));
#34377=CARTESIAN_POINT('Ctrl Pts',(-30.1022963720935,32.1656831804107,166.));
#34378=CARTESIAN_POINT('Ctrl Pts',(-30.1022518409735,32.1774789678619,166.));
#34379=CARTESIAN_POINT('Ctrl Pts',(-30.1023166880166,32.1892756806987,166.));
#34380=CARTESIAN_POINT('Ctrl Pts',(-30.1024899696769,32.201068577993,166.));
#34381=CARTESIAN_POINT('Ctrl Pts',(-30.103534091715,32.272127592208,166.));
#34382=CARTESIAN_POINT('Ctrl Pts',(-30.1085109983323,32.3430831832316,166.));
#34383=CARTESIAN_POINT('Ctrl Pts',(-30.1172406743503,32.4136000964793,166.));
#34384=CARTESIAN_POINT('Ctrl Pts',(-30.1261541338587,32.485601583085,166.));
#34385=CARTESIAN_POINT('Ctrl Pts',(-30.1389799843928,32.5571466616736,166.));
#34386=CARTESIAN_POINT('Ctrl Pts',(-30.1555792981318,32.627894619499,166.));
#34387=CARTESIAN_POINT('Ctrl Pts',(-30.1722789267301,32.6990701294235,166.));
#34388=CARTESIAN_POINT('Ctrl Pts',(-30.1927978434914,32.7694399245741,166.));
#34389=CARTESIAN_POINT('Ctrl Pts',(-30.2170469852316,32.838657990524,166.));
#34390=CARTESIAN_POINT('Ctrl Pts',(-30.2230311731062,32.8557395810976,166.));
#34391=CARTESIAN_POINT('Ctrl Pts',(-30.2292427770505,32.8727509916663,166.));
#34392=CARTESIAN_POINT('Ctrl Pts',(-30.2356809367261,32.8896869118155,166.));
#34393=CARTESIAN_POINT('Ctrl Pts',(-30.2407432797558,32.9030036733807,166.));
#34394=CARTESIAN_POINT('Ctrl Pts',(-30.2459464565493,32.9162753272425,166.));
#34395=CARTESIAN_POINT('Ctrl Pts',(-30.2512816393884,32.9294791679086,166.));
#34396=CARTESIAN_POINT('Ctrl Pts',(-30.2795038677291,32.9993252851818,166.));
#34397=CARTESIAN_POINT('Ctrl Pts',(-30.311462547048,33.0674005959196,166.));
#34398=CARTESIAN_POINT('Ctrl Pts',(-30.3469997305368,33.1333481914682,166.));
#34399=CARTESIAN_POINT('Ctrl Pts',(-30.382575226724,33.1993668852328,166.));
#34400=CARTESIAN_POINT('Ctrl Pts',(-30.4217371183794,33.2632543879031,166.));
#34401=CARTESIAN_POINT('Ctrl Pts',(-30.4643787112962,33.3246482023152,166.));
#34402=CARTESIAN_POINT('Ctrl Pts',(-30.5060510266821,33.3846464861954,166.));
#34403=CARTESIAN_POINT('Ctrl Pts',(-30.5510469865186,33.4422641424414,166.));
#34404=CARTESIAN_POINT('Ctrl Pts',(-30.5993123479533,33.4971432210983,166.));
#34405=CARTESIAN_POINT('Ctrl Pts',(-30.609639774304,33.5088857964396,166.));
#34406=CARTESIAN_POINT('Ctrl Pts',(-30.6201170449146,33.5205028855144,166.));
#34407=CARTESIAN_POINT('Ctrl Pts',(-30.6307438842162,33.5319907951258,166.));
#34408=CARTESIAN_POINT('Ctrl Pts',(-30.6398545795245,33.5418397108032,166.));
#34409=CARTESIAN_POINT('Ctrl Pts',(-30.6490752115469,33.5515936765095,166.));
#34410=CARTESIAN_POINT('Ctrl Pts',(-30.6584039191552,33.5612522752607,166.));
#34411=CARTESIAN_POINT('Ctrl Pts',(-31.6163320011529,34.0186125009919,166.));
#34412=CARTESIAN_POINT('Ctrl Pts',(-31.6906427588626,34.0256324377615,166.));
#34413=CARTESIAN_POINT('Ctrl Pts',(-31.7652023131977,34.0282488164819,166.));
#34414=CARTESIAN_POINT('Ctrl Pts',(-31.8396884813956,34.0266257252458,166.));
#34415=CARTESIAN_POINT('Ctrl Pts',(-31.9122243505307,34.0250451320115,166.));
#34416=CARTESIAN_POINT('Ctrl Pts',(-31.9846914092729,34.0194435195122,166.));
#34417=CARTESIAN_POINT('Ctrl Pts',(-32.0567789289828,34.0099285531527,166.));
#34418=CARTESIAN_POINT('Ctrl Pts',(-32.0728687183824,34.0078048318001,166.));
#34419=CARTESIAN_POINT('Ctrl Pts',(-32.0889416464922,34.0054856654506,166.));
#34420=CARTESIAN_POINT('Ctrl Pts',(-32.1049873135507,34.0029730647847,166.));
#34421=CARTESIAN_POINT('Ctrl Pts',(-32.1786235791049,33.9914423176246,166.));
#34422=CARTESIAN_POINT('Ctrl Pts',(-32.2515406184048,33.9758657941873,166.));
#34423=CARTESIAN_POINT('Ctrl Pts',(-32.3234063428329,33.9563835294395,166.));
#34424=CARTESIAN_POINT('Ctrl Pts',(-32.3738567719135,33.9427067923884,166.));
#34425=CARTESIAN_POINT('Ctrl Pts',(-32.4237888208937,33.9271041460939,166.));
#34426=CARTESIAN_POINT('Ctrl Pts',(-32.4730796607622,33.9096108952537,166.));
#34427=CARTESIAN_POINT('Ctrl Pts',(-32.4918010174038,33.902966711696,166.));
#34428=CARTESIAN_POINT('Ctrl Pts',(-32.5104297908714,33.8960496891882,166.));
#34429=CARTESIAN_POINT('Ctrl Pts',(-32.5289589179083,33.8888614002562,166.));
#34430=CARTESIAN_POINT('Ctrl Pts',(-32.5466609278563,33.8819939875644,166.));
#34431=CARTESIAN_POINT('Ctrl Pts',(-32.5642774649958,33.8748765254527,166.));
#34432=CARTESIAN_POINT('Ctrl Pts',(-32.5817714091896,33.8675236367515,166.));
#34433=CARTESIAN_POINT('Ctrl Pts',(-32.6487029413755,33.8393916099592,166.));
#34434=CARTESIAN_POINT('Ctrl Pts',(-32.7139143188879,33.8077914467863,166.));
#34435=CARTESIAN_POINT('Ctrl Pts',(-32.7770971725608,33.7728508117707,166.));
#34436=CARTESIAN_POINT('Ctrl Pts',(-32.8389245367741,33.7386597735164,166.));
#34437=CARTESIAN_POINT('Ctrl Pts',(-32.8988101782919,33.7012694276233,166.));
#34438=CARTESIAN_POINT('Ctrl Pts',(-32.9564327793223,33.660762586154,166.));
#34439=CARTESIAN_POINT('Ctrl Pts',(-33.0127910447732,33.6211445320697,166.));
#34440=CARTESIAN_POINT('Ctrl Pts',(-33.0669850520193,33.5785447170987,166.));
#34441=CARTESIAN_POINT('Ctrl Pts',(-33.1186737258448,33.53301341985,166.));
#34442=CARTESIAN_POINT('Ctrl Pts',(-33.1354926710747,33.5181980195313,166.));
#34443=CARTESIAN_POINT('Ctrl Pts',(-33.1520459961584,33.5030720531806,166.));
#34444=CARTESIAN_POINT('Ctrl Pts',(-33.1683208481947,33.4876367513471,166.));
#34445=CARTESIAN_POINT('Ctrl Pts',(-33.177455472586,33.4789733432682,166.));
#34446=CARTESIAN_POINT('Ctrl Pts',(-33.1865031947452,33.4702115198622,166.));
#34447=CARTESIAN_POINT('Ctrl Pts',(-33.195449274418,33.4613641289918,166.));
#34448=CARTESIAN_POINT('Ctrl Pts',(-33.2440183877757,33.4133308064843,166.));
#34449=CARTESIAN_POINT('Ctrl Pts',(-33.2896824911655,33.3626963940901,166.));
#34450=CARTESIAN_POINT('Ctrl Pts',(-33.3321490497204,33.3095423506968,166.));
#34451=CARTESIAN_POINT('Ctrl Pts',(-33.3382529548252,33.3019022864239,166.));
#34452=CARTESIAN_POINT('Ctrl Pts',(-33.3442907274727,33.2942101177445,166.));
#34453=CARTESIAN_POINT('Ctrl Pts',(-33.3502614231889,33.2864660381261,166.));
#34454=CARTESIAN_POINT('Ctrl Pts',(-33.392620387346,33.2315258424474,166.));
#34455=CARTESIAN_POINT('Ctrl Pts',(-33.4316073256674,33.1739742618556,166.));
#34456=CARTESIAN_POINT('Ctrl Pts',(-33.4671551192539,33.1141730601304,166.));
#34457=CARTESIAN_POINT('Ctrl Pts',(-33.5003163244037,33.0583867589698,166.));
#34458=CARTESIAN_POINT('Ctrl Pts',(-33.5304842720454,33.0006417881322,166.));
#34459=CARTESIAN_POINT('Ctrl Pts',(-33.557564760225,32.9412263929792,166.));
#34460=CARTESIAN_POINT('Ctrl Pts',(-33.563460103192,32.9282918354623,166.));
#34461=CARTESIAN_POINT('Ctrl Pts',(-33.569208978742,32.9152781209338,166.));
#34462=CARTESIAN_POINT('Ctrl Pts',(-33.5748101691781,32.9021882506626,166.));
#34463=CARTESIAN_POINT('Ctrl Pts',(-33.5793366711509,32.8916099058836,166.));
#34464=CARTESIAN_POINT('Ctrl Pts',(-33.5837664961298,32.8809821314316,166.));
#34465=CARTESIAN_POINT('Ctrl Pts',(-33.5880939820481,32.8703195344679,166.));
#34466=CARTESIAN_POINT('Ctrl Pts',(-33.6138044493615,32.8069708937352,166.));
#34467=CARTESIAN_POINT('Ctrl Pts',(-33.6359573309018,32.7422777280778,166.));
#34468=CARTESIAN_POINT('Ctrl Pts',(-33.654506474946,32.6765896583697,166.));
#34469=CARTESIAN_POINT('Ctrl Pts',(-33.672970327122,32.6112036326896,166.));
#34470=CARTESIAN_POINT('Ctrl Pts',(-33.6878635141003,32.5448306965761,166.));
#34471=CARTESIAN_POINT('Ctrl Pts',(-33.6990894526804,32.4778130439757,166.));
#34472=CARTESIAN_POINT('Ctrl Pts',(-33.7100753481424,32.4122284231156,166.));
#34473=CARTESIAN_POINT('Ctrl Pts',(-33.7175490214282,32.3460253994248,166.));
#34474=CARTESIAN_POINT('Ctrl Pts',(-33.7213720579008,32.2795375564111,166.));
#34475=CARTESIAN_POINT('Ctrl Pts',(-33.7221759064895,32.2655575279288,166.));
#34476=CARTESIAN_POINT('Ctrl Pts',(-33.7228181881339,32.2515649821506,166.));
#34477=CARTESIAN_POINT('Ctrl Pts',(-33.72329734684,32.2375631548068,166.));
#34478=CARTESIAN_POINT('Ctrl Pts',(-33.7237537386745,32.2242266139311,166.));
#34479=CARTESIAN_POINT('Ctrl Pts',(-33.7240620424032,32.2108797919198,166.));
#34480=CARTESIAN_POINT('Ctrl Pts',(-33.7242209355861,32.1975471702555,166.));
#34481=CARTESIAN_POINT('Ctrl Pts',(-33.7249995439963,32.1322146546463,166.));
#34482=CARTESIAN_POINT('Ctrl Pts',(-33.7221997863358,32.0671063303133,166.));
#34483=CARTESIAN_POINT('Ctrl Pts',(-33.715743471838,32.0025317991948,166.));
#34484=CARTESIAN_POINT('Ctrl Pts',(-33.7094097335377,31.9391832462227,166.));
#34485=CARTESIAN_POINT('Ctrl Pts',(-33.6995568087996,31.8763475422056,166.));
#34486=CARTESIAN_POINT('Ctrl Pts',(-33.6860642167824,31.8143341524862,166.));
#34487=CARTESIAN_POINT('Ctrl Pts',(-33.67300924081,31.7543320927102,166.));
#34488=CARTESIAN_POINT('Ctrl Pts',(-33.6565466301776,31.6950992468525,166.));
#34489=CARTESIAN_POINT('Ctrl Pts',(-33.6365261315778,31.6369428273527,166.));
#34490=CARTESIAN_POINT('Ctrl Pts',(-33.6332193297538,31.627337084862,166.));
#34491=CARTESIAN_POINT('Ctrl Pts',(-33.6298153744735,31.6177607817841,166.));
#34492=CARTESIAN_POINT('Ctrl Pts',(-33.6263134827184,31.6082153937475,166.));
#34493=CARTESIAN_POINT('Ctrl Pts',(-33.6225506333734,31.5979586926172,166.));
#34494=CARTESIAN_POINT('Ctrl Pts',(-33.6186747062679,31.5877376855654,166.));
#34495=CARTESIAN_POINT('Ctrl Pts',(-33.6146867573338,31.577553736751,166.));
#34496=CARTESIAN_POINT('Origin',(-32.,32.,180.545925280538));
#34497=CARTESIAN_POINT('Ctrl Pts',(-34.0565967526292,32.0015021117824,178.795925280538));
#34498=CARTESIAN_POINT('Ctrl Pts',(-34.0574112680809,32.0995962853728,178.790592107115));
#34499=CARTESIAN_POINT('Ctrl Pts',(-34.0064252466113,32.8782049323825,178.748215670618));
#34500=CARTESIAN_POINT('Ctrl Pts',(-33.0117514203349,34.2080115215553,178.668795971049));
#34501=CARTESIAN_POINT('Ctrl Pts',(-30.6939036908508,34.0474398623436,178.557666181829));
#34502=CARTESIAN_POINT('Ctrl Pts',(-29.5714225144095,32.0133607849434,178.446536392609));
#34503=CARTESIAN_POINT('Ctrl Pts',(-30.6715287936437,29.9669129302815,178.33540660339));
#34504=CARTESIAN_POINT('Ctrl Pts',(-32.9874474959699,29.7811936333636,178.22427681417));
#34505=CARTESIAN_POINT('Ctrl Pts',(-34.0018725639557,31.1064095882227,178.144449706553));
#34506=CARTESIAN_POINT('Ctrl Pts',(-34.0573013963354,31.8927552482639,178.101665862009));
#34507=CARTESIAN_POINT('Ctrl Pts',(-34.0563933814841,31.9983925126321,178.095925280538));
#34508=CARTESIAN_POINT('Ctrl Pts',(-34.0526600320705,31.9978184065947,178.854074719462));
#34509=CARTESIAN_POINT('Ctrl Pts',(-34.0491237090593,32.4678825338461,178.828629953495));
#34510=CARTESIAN_POINT('Ctrl Pts',(-33.6567302575586,33.6292028150091,178.766141924454));
#34511=CARTESIAN_POINT('Ctrl Pts',(-31.7283973209264,34.4129390290683,178.666610632341));
#34512=CARTESIAN_POINT('Ctrl Pts',(-29.8255894209646,33.0815150230766,178.555480843121));
#34513=CARTESIAN_POINT('Ctrl Pts',(-29.9119598436444,30.7594178093493,178.444351053902));
#34514=CARTESIAN_POINT('Ctrl Pts',(-31.9096840054244,29.5731212000867,178.333221264681));
#34515=CARTESIAN_POINT('Ctrl Pts',(-33.7208631602512,30.4738805049478,178.236462486535));
#34516=CARTESIAN_POINT('Ctrl Pts',(-34.0499397056807,31.5817357019626,178.176746971462));
#34517=CARTESIAN_POINT('Ctrl Pts',(-34.0521188506995,32.0011671092335,178.154074719462));
#34518=CARTESIAN_POINT('Ctrl Pts',(-30.7309291201472,33.079358653048,179.));
#34519=CARTESIAN_POINT('Ctrl Pts',(-30.3720428517591,32.6573931542732,178.962956736927));
#34520=CARTESIAN_POINT('Ctrl Pts',(-30.1149436779728,31.4341262709582,178.88887021078));
#34521=CARTESIAN_POINT('Ctrl Pts',(-31.4545465157447,30.1067578728411,178.777740421561));
#34522=CARTESIAN_POINT('Ctrl Pts',(-33.2939137175247,30.5161313123725,178.666610632341));
#34523=CARTESIAN_POINT('Ctrl Pts',(-33.9488255415399,32.2815517198011,178.555480843121));
#34524=CARTESIAN_POINT('Ctrl Pts',(-32.8203323354559,33.7902650906004,178.444351053901));
#34525=CARTESIAN_POINT('Ctrl Pts',(-30.9410115824103,33.6600729094363,178.333221264682));
#34526=CARTESIAN_POINT('Ctrl Pts',(-30.0308990918633,32.0108329810029,178.222091475462));
#34527=CARTESIAN_POINT('Ctrl Pts',(-30.9228699210173,30.3515643955951,178.110961686242));
#34528=CARTESIAN_POINT('Ctrl Pts',(-32.8006266106757,30.2009824033015,177.999831897022));
#34529=CARTESIAN_POINT('Ctrl Pts',(-33.9456545335462,31.6968142000849,177.888702107803));
#34530=CARTESIAN_POINT('Ctrl Pts',(-33.3100424795202,33.4701319121845,177.777572318583));
#34531=CARTESIAN_POINT('Ctrl Pts',(-31.4754927960691,33.8979941813415,177.666442529363));
#34532=CARTESIAN_POINT('Ctrl Pts',(-30.1209668886363,32.5888360297234,177.555312740143));
#34533=CARTESIAN_POINT('Ctrl Pts',(-30.4861114761055,30.7407799227021,177.444182950924));
#34534=CARTESIAN_POINT('Ctrl Pts',(-32.2367505368386,30.0451491638923,177.333053161704));
#34535=CARTESIAN_POINT('Ctrl Pts',(-33.7707180178967,31.1385763032121,177.221923372484));
#34536=CARTESIAN_POINT('Ctrl Pts',(-33.6841435990266,33.020369258459,177.110793583264));
#34537=CARTESIAN_POINT('Ctrl Pts',(-32.0562592086395,33.9683312403004,176.999663794045));
#34538=CARTESIAN_POINT('Ctrl Pts',(-30.3768870072247,33.1148978626103,176.888534004825));
#34539=CARTESIAN_POINT('Ctrl Pts',(-30.1829702116221,31.2411220290648,176.777404215605));
#34540=CARTESIAN_POINT('Ctrl Pts',(-31.6519793750709,30.0618630959102,176.666274426386));
#34541=CARTESIAN_POINT('Ctrl Pts',(-33.4394932395446,30.656366033717,176.555144637166));
#34542=CARTESIAN_POINT('Ctrl Pts',(-33.9095985022262,32.4805482090353,176.444014847946));
#34543=CARTESIAN_POINT('Ctrl Pts',(-32.6320599242147,33.8649378734601,176.332885058727));
#34544=CARTESIAN_POINT('Ctrl Pts',(-30.7760669580592,33.542556621148,176.221755269507));
#34545=CARTESIAN_POINT('Ctrl Pts',(-30.0402042388412,31.8084442771746,176.110625480287));
#34546=CARTESIAN_POINT('Ctrl Pts',(-31.0979253471581,30.2496416535512,175.999495691067));
#34547=CARTESIAN_POINT('Ctrl Pts',(-32.9812153951526,30.2927480066755,175.888365901848));
#34548=CARTESIAN_POINT('Ctrl Pts',(-33.9665077543468,31.898312869751,175.777236112628));
#34549=CARTESIAN_POINT('Ctrl Pts',(-33.1520735426487,33.5969406916609,175.666106323408));
#34550=CARTESIAN_POINT('Ctrl Pts',(-31.2832741184371,33.8340657106725,175.554976534188));
#34551=CARTESIAN_POINT('Ctrl Pts',(-30.0704144484628,32.3926736808866,175.443846744969));
#34552=CARTESIAN_POINT('Ctrl Pts',(-30.6234905497716,30.5919109567242,175.332716955749));
#34553=CARTESIAN_POINT('Ctrl Pts',(-32.4363331723059,30.0798160548769,175.221587166529));
#34554=CARTESIAN_POINT('Ctrl Pts',(-33.8498484073821,31.3250526760791,175.110457377309));
#34555=CARTESIAN_POINT('Ctrl Pts',(-33.5704024407928,33.1879937686345,174.99932758809));
#34556=CARTESIAN_POINT('Ctrl Pts',(-31.8537411906952,33.9636958473916,174.88819779887));
#34557=CARTESIAN_POINT('Ctrl Pts',(-30.2709344167626,32.9422447820107,174.77706800965));
#34558=CARTESIAN_POINT('Ctrl Pts',(-30.2705497136734,31.0584615103527,174.66593822043));
#34559=CARTESIAN_POINT('Ctrl Pts',(-31.8529391575229,30.0363640538602,174.554808431211));
#34560=CARTESIAN_POINT('Ctrl Pts',(-33.569917089599,30.8113649205297,174.443678641991));
#34561=CARTESIAN_POINT('Ctrl Pts',(-33.850123926316,32.6741917217198,174.332548852772));
#34562=CARTESIAN_POINT('Ctrl Pts',(-32.4371174094271,33.9200055704967,174.221419063552));
#34563=CARTESIAN_POINT('Ctrl Pts',(-30.6240657797714,33.4086511427483,174.110289274332));
#34564=CARTESIAN_POINT('Ctrl Pts',(-30.0702542270837,31.6081144653424,173.999159485112));
#34565=CARTESIAN_POINT('Ctrl Pts',(-31.2825250785475,30.1662271794333,173.888029695893));
#34566=CARTESIAN_POINT('Ctrl Pts',(-33.1514211974331,30.4025888924688,173.776899906673));
#34567=CARTESIAN_POINT('Ctrl Pts',(-33.9665491230709,32.1008839279147,173.665770117453));
#34568=CARTESIAN_POINT('Ctrl Pts',(-32.9819126176114,33.7068510865737,173.554640328233));
#34569=CARTESIAN_POINT('Ctrl Pts',(-31.0986403329129,33.7507266408298,173.443510539014));
#34570=CARTESIAN_POINT('Ctrl Pts',(-30.0402826406939,32.1923561592382,173.332380749794));
#34571=CARTESIAN_POINT('Ctrl Pts',(-30.7754370234621,30.4579434067276,173.221250960574));
#34572=CARTESIAN_POINT('Ctrl Pts',(-32.6312981625253,30.1348041254724,173.110121171354));
#34573=CARTESIAN_POINT('Ctrl Pts',(-33.9094020693888,31.518671881378,172.998991382135));
#34574=CARTESIAN_POINT('Ctrl Pts',(-33.4400419089509,33.3430459116603,172.887861592915));
#34575=CARTESIAN_POINT('Ctrl Pts',(-31.6527710100454,33.9382788883175,172.776731803695));
#34576=CARTESIAN_POINT('Ctrl Pts',(-30.1832803172047,32.7596200461458,172.665602014475));
#34577=CARTESIAN_POINT('Ctrl Pts',(-30.3764317765537,30.8857651754778,172.554472225256));
#34578=CARTESIAN_POINT('Ctrl Pts',(-32.0554552671365,30.031645932839,172.443342436036));
#34579=CARTESIAN_POINT('Ctrl Pts',(-33.6837266986233,30.9789429865549,172.332212646816));
#34580=CARTESIAN_POINT('Ctrl Pts',(-33.7710697147857,32.8607003460735,172.221082857597));
#34581=CARTESIAN_POINT('Ctrl Pts',(-32.2375489344276,33.9547540827722,172.109953068377));
#34582=CARTESIAN_POINT('Ctrl Pts',(-30.4866259453921,33.2598380813431,171.998823279157));
#34583=CARTESIAN_POINT('Ctrl Pts',(-30.1207264792757,31.4119319302438,171.887693489937));
#34584=CARTESIAN_POINT('Ctrl Pts',(-31.4747177594533,30.1022192992527,171.776563700718));
#34585=CARTESIAN_POINT('Ctrl Pts',(-33.3094416497307,30.5293349850108,171.665433911498));
#34586=CARTESIAN_POINT('Ctrl Pts',(-33.9457787424778,32.302387343789,171.554304122278));
#34587=CARTESIAN_POINT('Ctrl Pts',(-32.8013602312011,33.7986980847857,171.443174333058));
#34588=CARTESIAN_POINT('Ctrl Pts',(-30.9235455267189,33.648859844655,171.332044543839));
#34589=CARTESIAN_POINT('Ctrl Pts',(-30.030890282521,31.9900029558365,171.220914754619));
#34590=CARTESIAN_POINT('Ctrl Pts',(-30.9403428976541,30.340295253423,171.109784965399));
#34591=CARTESIAN_POINT('Ctrl Pts',(-32.8195822013514,30.2095313363283,170.99865517618));
#34592=CARTESIAN_POINT('Ctrl Pts',(-33.9487487623708,31.7173849234018,170.88752538696));
#34593=CARTESIAN_POINT('Ctrl Pts',(-33.2944415893687,33.4838847637451,170.77639559774));
#34594=CARTESIAN_POINT('Ctrl Pts',(-31.4554755114109,33.8923493603691,170.66526580852));
#34595=CARTESIAN_POINT('Ctrl Pts',(-30.1148523402876,32.5689563440575,170.554136019301));
#34596=CARTESIAN_POINT('Ctrl Pts',(-30.499495863758,30.7248606517391,170.443006230081));
#34597=CARTESIAN_POINT('Ctrl Pts',(-32.2573845004273,30.0477586626387,170.331876440861));
#34598=CARTESIAN_POINT('Ctrl Pts',(-33.7797176335243,31.1573267743156,170.220746651641));
#34599=CARTESIAN_POINT('Ctrl Pts',(-33.6732724886538,33.0381002837283,170.109616862422));
#34600=CARTESIAN_POINT('Ctrl Pts',(-32.035466508052,33.9688156712016,169.998487073202));
#34601=CARTESIAN_POINT('Ctrl Pts',(-30.3652019638992,33.0976923073081,169.887357283983));
#34602=CARTESIAN_POINT('Ctrl Pts',(-30.1910868537395,31.2219728477436,169.776227494763));
#34603=CARTESIAN_POINT('Ctrl Pts',(-31.672469438191,30.0582954005711,169.665097705543));
#34604=CARTESIAN_POINT('Ctrl Pts',(-33.4536044408894,30.6716449458862,169.553967916323));
#34605=CARTESIAN_POINT('Ctrl Pts',(-33.904416422969,32.5006906313158,169.442838127104));
#34606=CARTESIAN_POINT('Ctrl Pts',(-32.6123271472845,33.8715096807286,169.331708337884));
#34607=CARTESIAN_POINT('Ctrl Pts',(-30.7598427068146,33.5295433660167,169.220578548664));
#34608=CARTESIAN_POINT('Ctrl Pts',(-30.0423367721263,31.7877555499318,169.109448759444));
#34609=CARTESIAN_POINT('Ctrl Pts',(-31.1164629936058,30.2402115528575,168.998318970225));
#34610=CARTESIAN_POINT('Ctrl Pts',(-32.9991927017948,30.3032068584901,168.887189181005));
#34611=CARTESIAN_POINT('Ctrl Pts',(-33.9674720850595,31.9190888462911,168.776059391785));
#34612=CARTESIAN_POINT('Ctrl Pts',(-33.1351423524959,33.6090198444933,168.664929602565));
#34613=CARTESIAN_POINT('Ctrl Pts',(-31.263942648888,33.8263933301663,168.553799813346));
#34614=CARTESIAN_POINT('Ctrl Pts',(-30.0663746511061,32.3722714463651,168.442670024126));
#34615=CARTESIAN_POINT('Ctrl Pts',(-30.6384396027317,30.5774507722043,168.331540234906));
#34616=CARTESIAN_POINT('Ctrl Pts',(-32.4565898656643,30.0845317239336,168.220410445686));
#34617=CARTESIAN_POINT('Ctrl Pts',(-33.856874032538,31.3446284705168,168.109280656467));
#34618=CARTESIAN_POINT('Ctrl Pts',(-33.5577672269115,33.2045141316663,167.998150867247));
#34619=CARTESIAN_POINT('Ctrl Pts',(-31.8330087380771,33.9620415260158,167.887021078027));
#34620=CARTESIAN_POINT('Ctrl Pts',(-30.2610788624257,32.9239297848845,167.775891288808));
#34621=CARTESIAN_POINT('Ctrl Pts',(-30.2805907108729,31.0402475411786,167.664761499588));
#34622=CARTESIAN_POINT('Ctrl Pts',(-31.873687382455,30.0349203051936,167.553631710368));
#34623=CARTESIAN_POINT('Ctrl Pts',(-33.5823838127623,30.8280127657554,167.442501921148));
#34624=CARTESIAN_POINT('Ctrl Pts',(-33.8429001024036,32.6936950903751,167.331372131929));
#34625=CARTESIAN_POINT('Ctrl Pts',(-32.4168134615631,33.9245154823387,167.220242342709));
#34626=CARTESIAN_POINT('Ctrl Pts',(-30.6092651719059,33.3940395824034,167.109112553489));
#34627=CARTESIAN_POINT('Ctrl Pts',(-30.0744992385868,31.5877549816332,166.997982764269));
#34628=CARTESIAN_POINT('Ctrl Pts',(-31.301936984442,30.1587500931461,166.88685297505));
#34629=CARTESIAN_POINT('Ctrl Pts',(-33.1682216796882,30.4148421561058,166.77572318583));
#34630=CARTESIAN_POINT('Ctrl Pts',(-33.9653885256372,32.1216432990863,166.66459339661));
#34631=CARTESIAN_POINT('Ctrl Pts',(-32.9638002467904,33.7171385570736,166.553463607391));
#34632=CARTESIAN_POINT('Ctrl Pts',(-31.080260054756,33.7410849968787,166.442333818171));
#34633=CARTESIAN_POINT('Ctrl Pts',(-30.038236774059,32.1716953131642,166.331204028951));
#34634=CARTESIAN_POINT('Ctrl Pts',(-30.7920440433359,30.4449968588325,166.220074239731));
#34635=CARTESIAN_POINT('Ctrl Pts',(-32.6504510143993,30.1417770670916,166.108944450512));
#34636=CARTESIAN_POINT('Ctrl Pts',(-33.9154261131066,31.5384503702043,165.997814661292));
#34637=CARTESIAN_POINT('Ctrl Pts',(-33.4236059800711,33.3590424673056,165.886684872072));
#34638=CARTESIAN_POINT('Ctrl Pts',(-32.2331222331372,33.7401334029927,165.812598345926));
#34639=CARTESIAN_POINT('Ctrl Pts',(-31.6889203620492,33.6366995627947,165.775555082853));
#34640=CARTESIAN_POINT('Ctrl Pts',(-30.6322193753407,33.1633123698092,179.074814972382));
#34641=CARTESIAN_POINT('Ctrl Pts',(-30.2454185337562,32.7085259251263,179.037771709309));
#34642=CARTESIAN_POINT('Ctrl Pts',(-29.9683219002241,31.3901119828099,178.963685183163));
#34643=CARTESIAN_POINT('Ctrl Pts',(-31.4121205369524,29.959499394063,178.852555393943));
#34644=CARTESIAN_POINT('Ctrl Pts',(-33.3945557658816,30.4007143551266,178.741425604723));
#34645=CARTESIAN_POINT('Ctrl Pts',(-34.100407360122,32.303451125778,178.630295815503));
#34646=CARTESIAN_POINT('Ctrl Pts',(-32.8841386970822,33.9295139009187,178.519166026284));
#34647=CARTESIAN_POINT('Ctrl Pts',(-30.8586422852238,33.7891952270721,178.408036237064));
#34648=CARTESIAN_POINT('Ctrl Pts',(-29.877740232712,32.0116755823164,178.296906447845));
#34649=CARTESIAN_POINT('Ctrl Pts',(-30.8390895452261,30.2233472404906,178.185776658624));
#34650=CARTESIAN_POINT('Ctrl Pts',(-32.8629002391071,30.0610528133222,178.074646869405));
#34651=CARTESIAN_POINT('Ctrl Pts',(-34.0969897075991,31.6732320712899,177.963517080185));
#34652=CARTESIAN_POINT('Ctrl Pts',(-33.4119390409275,33.5844804077551,177.852387290965));
#34653=CARTESIAN_POINT('Ctrl Pts',(-31.434696042262,34.0456222801803,177.741257501746));
#34654=CARTESIAN_POINT('Ctrl Pts',(-29.9748136029135,32.634636351163,177.630127712526));
#34655=CARTESIAN_POINT('Ctrl Pts',(-30.3683595425993,30.6428363842767,177.518997923306));
#34656=CARTESIAN_POINT('Ctrl Pts',(-32.2551652569659,29.8930986911959,177.407868134087));
#34657=CARTESIAN_POINT('Ctrl Pts',(-33.908446435155,31.0715738097895,177.296738344867));
#34658=CARTESIAN_POINT('Ctrl Pts',(-33.815138161676,33.0997347144866,177.185608555647));
#34659=CARTESIAN_POINT('Ctrl Pts',(-32.0606351124727,34.1214302338311,177.074478766427));
#34660=CARTESIAN_POINT('Ctrl Pts',(-30.2506394730227,33.2016158586267,176.963348977208));
#34661=CARTESIAN_POINT('Ctrl Pts',(-30.0416396133364,31.1820956562754,176.852219187988));
#34662=CARTESIAN_POINT('Ctrl Pts',(-31.6249099437101,29.9111126514394,176.741089398768));
#34663=CARTESIAN_POINT('Ctrl Pts',(-33.5514586250734,30.5518566891006,176.629959609548));
#34664=CARTESIAN_POINT('Ctrl Pts',(-34.0581291980526,32.5179257833176,176.518829820329));
#34665=CARTESIAN_POINT('Ctrl Pts',(-32.681222248252,34.0099948158986,176.407700031109));
#34666=CARTESIAN_POINT('Ctrl Pts',(-30.6808680844989,33.6625383911503,176.296570241889));
#34667=CARTESIAN_POINT('Ctrl Pts',(-29.8877691443733,31.793544859958,176.18544045267));
#34668=CARTESIAN_POINT('Ctrl Pts',(-31.0277609771516,30.1134968341871,176.07431066345));
#34669=CARTESIAN_POINT('Ctrl Pts',(-33.0575354201357,30.1599560474108,175.96318087423));
#34670=CARTESIAN_POINT('Ctrl Pts',(-34.1194649151115,31.8904035316389,175.85205108501));
#34671=CARTESIAN_POINT('Ctrl Pts',(-33.2416831044143,33.7211525151669,175.740921295791));
#34672=CARTESIAN_POINT('Ctrl Pts',(-31.2275263820511,33.9767213819458,175.629791506571));
#34673=CARTESIAN_POINT('Ctrl Pts',(-29.9203291377064,32.4232162766138,175.518661717351));
#34674=CARTESIAN_POINT('Ctrl Pts',(-30.5164241134418,30.4823882245166,175.407531928131));
#34675=CARTESIAN_POINT('Ctrl Pts',(-32.4702716518446,29.9304620115263,175.296402138912));
#34676=CARTESIAN_POINT('Ctrl Pts',(-33.9937316743629,31.2725545223828,175.185272349692));
#34677=CARTESIAN_POINT('Ctrl Pts',(-33.692550089624,33.2803972455365,175.074142560472));
#34678=CARTESIAN_POINT('Ctrl Pts',(-31.8423650178026,34.1164342949053,174.963012771252));
#34679=CARTESIAN_POINT('Ctrl Pts',(-30.1364457722081,33.0155336293509,174.851882982033));
#34680=CARTESIAN_POINT('Ctrl Pts',(-30.1360311464846,30.9852275992181,174.740753192813));
#34681=CARTESIAN_POINT('Ctrl Pts',(-31.841500601598,29.8836302655325,174.629623403593));
#34682=CARTESIAN_POINT('Ctrl Pts',(-33.6920269872744,30.7189115617574,174.518493614374));
#34683=CARTESIAN_POINT('Ctrl Pts',(-33.9940286234659,32.7266311038364,174.407363825154));
#34684=CARTESIAN_POINT('Ctrl Pts',(-32.4711168878014,34.0693457396704,174.296234035934));
#34685=CARTESIAN_POINT('Ctrl Pts',(-30.5170440854709,33.5182175956782,174.185104246715));
#34686=CARTESIAN_POINT('Ctrl Pts',(-29.9201564541303,31.5776331725056,174.073974457495));
#34687=CARTESIAN_POINT('Ctrl Pts',(-31.2267190810055,30.0235942894783,173.962844668275));
#34688=CARTESIAN_POINT('Ctrl Pts',(-33.2409800190622,30.278340479493,173.851714879055));
#34689=CARTESIAN_POINT('Ctrl Pts',(-34.119509501541,32.1087307920557,173.740585089836));
#34690=CARTESIAN_POINT('Ctrl Pts',(-33.058286873333,33.8396118628653,173.629455300616));
#34691=CARTESIAN_POINT('Ctrl Pts',(-31.0285315752938,33.8869001065405,173.518325511396));
#34692=CARTESIAN_POINT('Ctrl Pts',(-29.8878536444094,32.2073178352894,173.407195722176));
#34693=CARTESIAN_POINT('Ctrl Pts',(-30.680189152888,30.3380005294497,173.296065932957));
#34694=CARTESIAN_POINT('Ctrl Pts',(-32.680401235891,29.9897271154239,173.184936143737));
#34695=CARTESIAN_POINT('Ctrl Pts',(-34.0579174864506,31.4812336448605,173.073806354517));
#34696=CARTESIAN_POINT('Ctrl Pts',(-33.5520499705965,33.4475095167339,172.962676565297));
#34697=CARTESIAN_POINT('Ctrl Pts',(-31.6257631529336,34.0890403764795,172.851546776078));
#34698=CARTESIAN_POINT('Ctrl Pts',(-30.0419738392762,32.8187041383706,172.740416986858));
#34699=CARTESIAN_POINT('Ctrl Pts',(-30.2501488340038,30.7990987513016,172.629287197638));
#34700=CARTESIAN_POINT('Ctrl Pts',(-32.0597686395054,29.8785451638096,172.518157408419));
#34701=CARTESIAN_POINT('Ctrl Pts',(-33.8146888342956,30.8995240361794,172.407027619199));
#34702=CARTESIAN_POINT('Ctrl Pts',(-33.9088254874194,32.9276465764729,172.295897829979));
#34703=CARTESIAN_POINT('Ctrl Pts',(-32.2560257548074,34.1067970298866,172.184768040759));
#34704=CARTESIAN_POINT('Ctrl Pts',(-30.3689140278794,33.3578296888105,172.07363825154));
#34705=CARTESIAN_POINT('Ctrl Pts',(-29.9745544942453,31.3661913415849,171.96250846232));
#34706=CARTESIAN_POINT('Ctrl Pts',(-31.433860722436,29.954607805172,171.8513786731));
#34707=CARTESIAN_POINT('Ctrl Pts',(-33.4112914779285,30.4149450241111,171.740248883881));
#34708=CARTESIAN_POINT('Ctrl Pts',(-34.0971235776395,32.3259073677782,171.629119094661));
#34709=CARTESIAN_POINT('Ctrl Pts',(-32.8636909214531,33.938602822773,171.517989305441));
#34710=CARTESIAN_POINT('Ctrl Pts',(-30.8398177002908,33.7771099976381,171.406859516221));
#34711=CARTESIAN_POINT('Ctrl Pts',(-29.8777307381692,31.9892253746203,171.295729727002));
#34712=CARTESIAN_POINT('Ctrl Pts',(-30.8579215894234,30.211201571904,171.184599937782));
#34713=CARTESIAN_POINT('Ctrl Pts',(-32.8833302167127,30.0702666918701,171.073470148562));
#34714=CARTESIAN_POINT('Ctrl Pts',(-34.1003246089838,31.6954028083503,170.962340359342));
#34715=CARTESIAN_POINT('Ctrl Pts',(-33.3951246961849,33.5993029714094,170.851210570123));
#34716=CARTESIAN_POINT('Ctrl Pts',(-31.4131217909349,34.0395383987531,170.740080780903));
#34717=CARTESIAN_POINT('Ctrl Pts',(-29.9682234581922,32.6132104014309,170.628950991683));
#34718=CARTESIAN_POINT('Ctrl Pts',(-30.3827849828128,30.625678894709,170.517821202464));
#34719=CARTESIAN_POINT('Ctrl Pts',(-32.2774041531966,29.8959111596577,170.406691413244));
#34720=CARTESIAN_POINT('Ctrl Pts',(-33.9181460508977,31.0917827133943,170.295561624024));
#34721=CARTESIAN_POINT('Ctrl Pts',(-33.8034214842449,33.1188448786261,170.184431834804));
#34722=CARTESIAN_POINT('Ctrl Pts',(-32.0382251325028,34.1219523443068,170.073302045585));
#34723=CARTESIAN_POINT('Ctrl Pts',(-30.2380455540284,33.1830720360928,169.962172256365));
#34724=CARTESIAN_POINT('Ctrl Pts',(-30.050387576907,31.1614570303288,169.851042467145));
#34725=CARTESIAN_POINT('Ctrl Pts',(-31.6469937467338,29.9072674567879,169.739912677925));
#34726=CARTESIAN_POINT('Ctrl Pts',(-33.5666674113567,30.5683240120554,169.628782888706));
#34727=CARTESIAN_POINT('Ctrl Pts',(-34.052544050906,32.5396349056103,169.517653099486));
#34728=CARTESIAN_POINT('Ctrl Pts',(-32.6599546339806,34.0170777856472,169.406523310266));
#34729=CARTESIAN_POINT('Ctrl Pts',(-30.6633818929439,33.6485129505583,169.295393521047));
#34730=CARTESIAN_POINT('Ctrl Pts',(-29.8900675484697,31.7712469404953,169.184263731827));
#34731=CARTESIAN_POINT('Ctrl Pts',(-31.0477405023622,30.1033332497709,169.073133942607));
#34732=CARTESIAN_POINT('Ctrl Pts',(-33.0769110216873,30.1712284003545,168.962004153387));
#34733=CARTESIAN_POINT('Ctrl Pts',(-34.1205042525398,31.9127954867463,168.850874364168));
#34734=CARTESIAN_POINT('Ctrl Pts',(-33.2234349874565,33.734171197944,168.739744574948));
#34735=CARTESIAN_POINT('Ctrl Pts',(-31.2066912892952,33.9684522351487,168.628614785728));
#34736=CARTESIAN_POINT('Ctrl Pts',(-29.9159751204173,32.4012271335949,168.517484996508));
#34737=CARTESIAN_POINT('Ctrl Pts',(-30.5325359203711,30.4668033107586,168.406355207289));
#34738=CARTESIAN_POINT('Ctrl Pts',(-32.4921039333468,29.935544470568,168.295225418069));
#34739=CARTESIAN_POINT('Ctrl Pts',(-34.001303760459,31.2936529438889,168.184095628849));
#34740=CARTESIAN_POINT('Ctrl Pts',(-33.678932094751,33.298202580783,168.07296583963));
#34741=CARTESIAN_POINT('Ctrl Pts',(-31.8200199719562,34.1146512985726,167.96183605041));
#34742=CARTESIAN_POINT('Ctrl Pts',(-30.1258236418911,32.9957940713738,167.85070626119));
#34743=CARTESIAN_POINT('Ctrl Pts',(-30.1468531436163,30.9655969272596,167.73957647197));
#34744=CARTESIAN_POINT('Ctrl Pts',(-31.8638626465465,29.8820742204885,167.628446682751));
#34745=CARTESIAN_POINT('Ctrl Pts',(-33.7054633860338,30.7368542949046,167.517316893531));
#34746=CARTESIAN_POINT('Ctrl Pts',(-33.9862429224935,32.7476514662021,167.406187104311));
#34747=CARTESIAN_POINT('Ctrl Pts',(-32.4492336762855,34.0742064374725,167.295057315092));
#34748=CARTESIAN_POINT('Ctrl Pts',(-30.5010922698608,33.5024695319151,167.183927525872));
#34749=CARTESIAN_POINT('Ctrl Pts',(-29.9247316473505,31.5556901055047,167.072797736652));
#34750=CARTESIAN_POINT('Ctrl Pts',(-31.2476408665352,30.0155356271018,166.961667947432));
#34751=CARTESIAN_POINT('Ctrl Pts',(-33.2590872615167,30.2915468156069,166.850538158212));
#34752=CARTESIAN_POINT('Ctrl Pts',(-34.1182586315479,32.1311048502107,166.739408368993));
#34753=CARTESIAN_POINT('Ctrl Pts',(-33.0387657021605,33.8506995042649,166.628278579773));
#34754=CARTESIAN_POINT('Ctrl Pts',(-31.0087216586548,33.8765085247972,166.517148790553));
#34755=CARTESIAN_POINT('Ctrl Pts',(-29.8856486479917,32.1850499656236,166.406019001334));
#34756=CARTESIAN_POINT('Ctrl Pts',(-30.698087885242,30.324046984657,166.294889212114));
#34757=CARTESIAN_POINT('Ctrl Pts',(-32.7010438178903,29.9972424201992,166.183759422894));
#34758=CARTESIAN_POINT('Ctrl Pts',(-34.0644100869902,31.5025505265502,166.072629633674));
#34759=CARTESIAN_POINT('Ctrl Pts',(-33.5343356368844,33.4647503022726,165.961499844455));
#34760=CARTESIAN_POINT('Ctrl Pts',(-32.2512547397663,33.8754829148802,165.887413318308));
#34761=CARTESIAN_POINT('Ctrl Pts',(-31.6647242417504,33.7640038755271,165.850370055235));
#34762=CARTESIAN_POINT('Ctrl Pts',(-30.5335096305342,33.2472660865704,179.149629944765));
#34763=CARTESIAN_POINT('Ctrl Pts',(-30.1187942157532,32.7596586959793,179.112586681692));
#34764=CARTESIAN_POINT('Ctrl Pts',(-29.8217001224754,31.3460976946617,179.038500155545));
#34765=CARTESIAN_POINT('Ctrl Pts',(-31.36969455816,29.8122409152849,178.927370366325));
#34766=CARTESIAN_POINT('Ctrl Pts',(-33.4951978142385,30.2852973978806,178.816240577106));
#34767=CARTESIAN_POINT('Ctrl Pts',(-34.2519891787042,32.325350531755,178.705110787886));
#34768=CARTESIAN_POINT('Ctrl Pts',(-32.9479450587086,34.068762711237,178.593980998666));
#34769=CARTESIAN_POINT('Ctrl Pts',(-30.7762729880373,33.9183175447078,178.482851209447));
#34770=CARTESIAN_POINT('Ctrl Pts',(-29.7245813735608,32.01251818363,178.371721420227));
#34771=CARTESIAN_POINT('Ctrl Pts',(-30.7553091694349,30.095130085386,178.260591631007));
#34772=CARTESIAN_POINT('Ctrl Pts',(-32.9251738675385,29.9211232233429,178.149461841787));
#34773=CARTESIAN_POINT('Ctrl Pts',(-34.2483248816519,31.649649942495,178.038332052568));
#34774=CARTESIAN_POINT('Ctrl Pts',(-33.5138356023347,33.6988289033257,177.927202263348));
#34775=CARTESIAN_POINT('Ctrl Pts',(-31.3938992884549,34.1932503790191,177.816072474128));
#34776=CARTESIAN_POINT('Ctrl Pts',(-29.8286603171907,32.6804366726026,177.704942684909));
#34777=CARTESIAN_POINT('Ctrl Pts',(-30.2506076090931,30.5448928458515,177.593812895689));
#34778=CARTESIAN_POINT('Ctrl Pts',(-32.2735799770931,29.7410482184995,177.482683106469));
#34779=CARTESIAN_POINT('Ctrl Pts',(-34.0461748524134,31.0045713163668,177.371553317249));
#34780=CARTESIAN_POINT('Ctrl Pts',(-33.9461327243253,33.1791001705142,177.26042352803));
#34781=CARTESIAN_POINT('Ctrl Pts',(-32.065011016306,34.2745292273619,177.14929373881));
#34782=CARTESIAN_POINT('Ctrl Pts',(-30.1243919388208,33.2883338546431,177.03816394959));
#34783=CARTESIAN_POINT('Ctrl Pts',(-29.9003090150507,31.1230692834861,176.92703416037));
#34784=CARTESIAN_POINT('Ctrl Pts',(-31.5978405123493,29.7603622069686,176.815904371151));
#34785=CARTESIAN_POINT('Ctrl Pts',(-33.6634240106023,30.4473473444842,176.704774581931));
#34786=CARTESIAN_POINT('Ctrl Pts',(-34.206659893879,32.5553033575998,176.593644792711));
#34787=CARTESIAN_POINT('Ctrl Pts',(-32.7303845722893,34.155051758337,176.482515003492));
#34788=CARTESIAN_POINT('Ctrl Pts',(-30.5856692109386,33.7825201611525,176.371385214272));
#34789=CARTESIAN_POINT('Ctrl Pts',(-29.7353340499054,31.7786454427414,176.260255425052));
#34790=CARTESIAN_POINT('Ctrl Pts',(-30.9575966071452,29.9773520148229,176.149125635832));
#34791=CARTESIAN_POINT('Ctrl Pts',(-33.1338554451188,30.0271640881461,176.037995846612));
#34792=CARTESIAN_POINT('Ctrl Pts',(-34.2724220758763,31.8824941935268,175.926866057393));
#34793=CARTESIAN_POINT('Ctrl Pts',(-33.3312926661799,33.845364338673,175.815736268173));
#34794=CARTESIAN_POINT('Ctrl Pts',(-31.171778645665,34.1193770532191,175.704606478954));
#34795=CARTESIAN_POINT('Ctrl Pts',(-29.7702438269501,32.453758872341,175.593476689734));
#34796=CARTESIAN_POINT('Ctrl Pts',(-30.409357677112,30.372865492309,175.482346900514));
#34797=CARTESIAN_POINT('Ctrl Pts',(-32.5042101313832,29.7811079681756,175.371217111294));
#34798=CARTESIAN_POINT('Ctrl Pts',(-34.1376149413436,31.2200563686864,175.260087322074));
#34799=CARTESIAN_POINT('Ctrl Pts',(-33.8146977384552,33.3728007224386,175.148957532855));
#34800=CARTESIAN_POINT('Ctrl Pts',(-31.83098884491,34.269172742419,175.037827743635));
#34801=CARTESIAN_POINT('Ctrl Pts',(-30.0019571276536,33.0888224766912,174.926697954415));
#34802=CARTESIAN_POINT('Ctrl Pts',(-30.0015125792959,30.9119936880836,174.815568165196));
#34803=CARTESIAN_POINT('Ctrl Pts',(-31.830062045673,29.7308964772048,174.704438375976));
#34804=CARTESIAN_POINT('Ctrl Pts',(-33.8141368849498,30.6264582029851,174.593308586756));
#34805=CARTESIAN_POINT('Ctrl Pts',(-34.1379333206158,32.7790704859529,174.482178797536));
#34806=CARTESIAN_POINT('Ctrl Pts',(-32.5051163661757,34.2186859088442,174.371049008317));
#34807=CARTESIAN_POINT('Ctrl Pts',(-30.4100223911704,33.6277840486081,174.259919219097));
#34808=CARTESIAN_POINT('Ctrl Pts',(-29.7700586811768,31.5471518796688,174.148789429877));
#34809=CARTESIAN_POINT('Ctrl Pts',(-31.1709130834636,29.8809613995232,174.037659640658));
#34810=CARTESIAN_POINT('Ctrl Pts',(-33.3305388406912,30.1540920665173,173.926529851438));
#34811=CARTESIAN_POINT('Ctrl Pts',(-34.2724698800112,32.1165776561968,173.815400062218));
#34812=CARTESIAN_POINT('Ctrl Pts',(-33.1346611290545,33.9723726391569,173.704270272998));
#34813=CARTESIAN_POINT('Ctrl Pts',(-30.9584228176748,34.0230735722514,173.593140483779));
#34814=CARTESIAN_POINT('Ctrl Pts',(-29.7354246481248,32.2222795113406,173.482010694559));
#34815=CARTESIAN_POINT('Ctrl Pts',(-30.584941282314,30.2180576521719,173.370880905339));
#34816=CARTESIAN_POINT('Ctrl Pts',(-32.7295043092566,29.8446501053754,173.259751116119));
#34817=CARTESIAN_POINT('Ctrl Pts',(-34.2064329035124,31.443795408343,173.1486213269));
#34818=CARTESIAN_POINT('Ctrl Pts',(-33.6640580322421,33.5519731218075,173.03749153768));
#34819=CARTESIAN_POINT('Ctrl Pts',(-31.5987552958217,34.2398018646414,172.92636174846));
#34820=CARTESIAN_POINT('Ctrl Pts',(-29.9006673613477,32.8777882305953,172.81523195924));
#34821=CARTESIAN_POINT('Ctrl Pts',(-30.1238658914538,30.7124323271253,172.704102170021));
#34822=CARTESIAN_POINT('Ctrl Pts',(-32.0640820118742,29.7254443947803,172.592972380801));
#34823=CARTESIAN_POINT('Ctrl Pts',(-33.9456509699678,30.8201050858039,172.481842591581));
#34824=CARTESIAN_POINT('Ctrl Pts',(-34.046581260053,32.9945928068723,172.370712802362));
#34825=CARTESIAN_POINT('Ctrl Pts',(-32.2745025751873,34.258839977001,172.259583013142));
#34826=CARTESIAN_POINT('Ctrl Pts',(-30.2512021103666,33.4558212962779,172.148453223922));
#34827=CARTESIAN_POINT('Ctrl Pts',(-29.828382509215,31.3204507529258,172.037323434703));
#34828=CARTESIAN_POINT('Ctrl Pts',(-31.3930036854187,29.8069963110913,171.926193645483));
#34829=CARTESIAN_POINT('Ctrl Pts',(-33.5131413061263,30.3005550632113,171.815063856263));
#34830=CARTESIAN_POINT('Ctrl Pts',(-34.2484684128012,32.3494273917673,171.703934067043));
#34831=CARTESIAN_POINT('Ctrl Pts',(-32.9260216117051,34.0785075607603,171.592804277824));
#34832=CARTESIAN_POINT('Ctrl Pts',(-30.7560898738626,33.9053601506212,171.481674488604));
#34833=CARTESIAN_POINT('Ctrl Pts',(-29.7245711938175,31.9884477934041,171.370544699384));
#34834=CARTESIAN_POINT('Ctrl Pts',(-30.7755002811927,30.0821078903851,171.259414910164));
#34835=CARTESIAN_POINT('Ctrl Pts',(-32.9470782320738,29.9310020474118,171.148285120945));
#34836=CARTESIAN_POINT('Ctrl Pts',(-34.2519004555968,31.6734206932988,171.037155331725));
#34837=CARTESIAN_POINT('Ctrl Pts',(-33.4958078030011,33.7147211790736,170.926025542505));
#34838=CARTESIAN_POINT('Ctrl Pts',(-31.3707680704589,34.1867274371371,170.814895753285));
#34839=CARTESIAN_POINT('Ctrl Pts',(-29.8215945760967,32.6574644588044,170.703765964066));
#34840=CARTESIAN_POINT('Ctrl Pts',(-30.2660741018676,30.5264971376789,170.592636174846));
#34841=CARTESIAN_POINT('Ctrl Pts',(-32.297423805966,29.7440636566767,170.481506385626));
#34842=CARTESIAN_POINT('Ctrl Pts',(-34.0565744682711,31.0262386524729,170.370376596407));
#34843=CARTESIAN_POINT('Ctrl Pts',(-33.9335704798359,33.1995894735239,170.259246807187));
#34844=CARTESIAN_POINT('Ctrl Pts',(-32.0409837569536,34.2750890174119,170.148117017967));
#34845=CARTESIAN_POINT('Ctrl Pts',(-30.1108891441576,33.2684517648776,170.036987228747));
#34846=CARTESIAN_POINT('Ctrl Pts',(-29.9096883000745,31.1009412129138,169.925857439528));
#34847=CARTESIAN_POINT('Ctrl Pts',(-31.6215180552765,29.7562395130049,169.814727650308));
#34848=CARTESIAN_POINT('Ctrl Pts',(-33.679730381824,30.4650030782245,169.703597861088));
#34849=CARTESIAN_POINT('Ctrl Pts',(-34.200671678843,32.5785791799048,169.592468071868));
#34850=CARTESIAN_POINT('Ctrl Pts',(-32.7075821206767,34.1626458905658,169.481338282649));
#34851=CARTESIAN_POINT('Ctrl Pts',(-30.5669210790731,33.7674825350999,169.370208493429));
#34852=CARTESIAN_POINT('Ctrl Pts',(-29.7377983248131,31.7547383310587,169.259078704209));
#34853=CARTESIAN_POINT('Ctrl Pts',(-30.9790180111186,29.9664549466843,169.147948914989));
#34854=CARTESIAN_POINT('Ctrl Pts',(-33.1546293415798,30.0392499422189,169.03681912577));
#34855=CARTESIAN_POINT('Ctrl Pts',(-34.2735364200202,31.9065021272017,168.92568933655));
#34856=CARTESIAN_POINT('Ctrl Pts',(-33.311727622417,33.8593225513948,168.81455954733));
#34857=CARTESIAN_POINT('Ctrl Pts',(-31.1494399297024,34.1105111401311,168.703429758111));
#34858=CARTESIAN_POINT('Ctrl Pts',(-29.7655755897285,32.4301828208247,168.592299968891));
#34859=CARTESIAN_POINT('Ctrl Pts',(-30.4266322380106,30.3561558493129,168.481170179671));
#34860=CARTESIAN_POINT('Ctrl Pts',(-32.5276180010293,29.7865572172026,168.370040390452));
#34861=CARTESIAN_POINT('Ctrl Pts',(-34.14573348838,31.2426774172609,168.258910601232));
#34862=CARTESIAN_POINT('Ctrl Pts',(-33.8000969625905,33.3918910298997,168.147780812012));
#34863=CARTESIAN_POINT('Ctrl Pts',(-31.8070312058352,34.2672610711293,168.036651022792));
#34864=CARTESIAN_POINT('Ctrl Pts',(-29.9905684213565,33.0676583578632,167.925521233573));
#34865=CARTESIAN_POINT('Ctrl Pts',(-30.0131155763598,30.8909463133407,167.814391444353));
#34866=CARTESIAN_POINT('Ctrl Pts',(-31.8540379106381,29.7292281357834,167.703261655133));
#34867=CARTESIAN_POINT('Ctrl Pts',(-33.8285429593054,30.6456958240537,167.592131865914));
#34868=CARTESIAN_POINT('Ctrl Pts',(-34.1295857425834,32.801607842029,167.481002076694));
#34869=CARTESIAN_POINT('Ctrl Pts',(-32.481653891008,34.2238973926065,167.369872287474));
#34870=CARTESIAN_POINT('Ctrl Pts',(-30.3929193678157,33.6108994814268,167.258742498254));
#34871=CARTESIAN_POINT('Ctrl Pts',(-29.7749640561141,31.5236252293763,167.147612709035));
#34872=CARTESIAN_POINT('Ctrl Pts',(-31.1933447486284,29.8723211610575,167.036482919815));
#34873=CARTESIAN_POINT('Ctrl Pts',(-33.3499528433452,30.1682514751079,166.925353130595));
#34874=CARTESIAN_POINT('Ctrl Pts',(-34.2711287374585,32.1405664013351,166.814223341375));
#34875=CARTESIAN_POINT('Ctrl Pts',(-33.1137311575306,33.9842604514563,166.703093552156));
#34876=CARTESIAN_POINT('Ctrl Pts',(-30.9371832625537,34.0119320527157,166.591963762936));
#34877=CARTESIAN_POINT('Ctrl Pts',(-29.7330605219244,32.1984046180832,166.480833973716));
#34878=CARTESIAN_POINT('Ctrl Pts',(-30.6041317271482,30.2030971104815,166.369704184496));
#34879=CARTESIAN_POINT('Ctrl Pts',(-32.7516366213812,29.8527077733068,166.258574395277));
#34880=CARTESIAN_POINT('Ctrl Pts',(-34.2133940608738,31.4666506828962,166.147444606057));
#34881=CARTESIAN_POINT('Ctrl Pts',(-33.6450652936977,33.5704581372396,166.036314816837));
#34882=CARTESIAN_POINT('Ctrl Pts',(-32.2693872463954,34.0108324267676,165.962228290691));
#34883=CARTESIAN_POINT('Ctrl Pts',(-31.6405281214516,33.8913081882595,165.925185027618));
#34884=CARTESIAN_POINT('Ctrl Pts',(-30.4347998857278,33.3312198033316,179.224444917147));
#34885=CARTESIAN_POINT('Ctrl Pts',(-29.9921698977503,32.8107914668324,179.187401654074));
#34886=CARTESIAN_POINT('Ctrl Pts',(-29.6750783447267,31.3020834065134,179.113315127928));
#34887=CARTESIAN_POINT('Ctrl Pts',(-31.3272685793676,29.6649824365068,179.002185338708));
#34888=CARTESIAN_POINT('Ctrl Pts',(-33.5958398625953,30.1698804406347,178.891055549488));
#34889=CARTESIAN_POINT('Ctrl Pts',(-34.4035709972863,32.3472499377319,178.779925760269));
#34890=CARTESIAN_POINT('Ctrl Pts',(-33.0117514203349,34.2080115215553,178.668795971049));
#34891=CARTESIAN_POINT('Ctrl Pts',(-30.6939036908508,34.0474398623436,178.557666181829));
#34892=CARTESIAN_POINT('Ctrl Pts',(-29.5714225144095,32.0133607849434,178.446536392609));
#34893=CARTESIAN_POINT('Ctrl Pts',(-30.6715287936437,29.9669129302815,178.33540660339));
#34894=CARTESIAN_POINT('Ctrl Pts',(-32.9874474959699,29.7811936333636,178.22427681417));
#34895=CARTESIAN_POINT('Ctrl Pts',(-34.3996600557047,31.6260678137,178.11314702495));
#34896=CARTESIAN_POINT('Ctrl Pts',(-33.615732163742,33.8131773988963,178.002017235731));
#34897=CARTESIAN_POINT('Ctrl Pts',(-31.3531025346477,34.3408784778579,177.890887446511));
#34898=CARTESIAN_POINT('Ctrl Pts',(-29.6825070314679,32.7262369940422,177.779757657291));
#34899=CARTESIAN_POINT('Ctrl Pts',(-30.1328556755869,30.4469493074261,177.668627868071));
#34900=CARTESIAN_POINT('Ctrl Pts',(-32.2919946972204,29.588997745803,177.557498078852));
#34901=CARTESIAN_POINT('Ctrl Pts',(-34.1839032696717,30.9375688229442,177.446368289632));
#34902=CARTESIAN_POINT('Ctrl Pts',(-34.0771272869747,33.2584656265418,177.335238500412));
#34903=CARTESIAN_POINT('Ctrl Pts',(-32.0693869201392,34.4276282208927,177.224108711192));
#34904=CARTESIAN_POINT('Ctrl Pts',(-29.9981444046188,33.3750518506594,177.112978921973));
#34905=CARTESIAN_POINT('Ctrl Pts',(-29.758978416765,31.0640429106968,177.001849132753));
#34906=CARTESIAN_POINT('Ctrl Pts',(-31.5707710809886,29.6096117624978,176.890719343533));
#34907=CARTESIAN_POINT('Ctrl Pts',(-33.7753893961311,30.3428379998679,176.779589554313));
#34908=CARTESIAN_POINT('Ctrl Pts',(-34.3551905897055,32.592680931882,176.668459765094));
#34909=CARTESIAN_POINT('Ctrl Pts',(-32.7795468963266,34.3001087007756,176.557329975874));
#34910=CARTESIAN_POINT('Ctrl Pts',(-30.4904703373783,33.9025019311548,176.446200186654));
#34911=CARTESIAN_POINT('Ctrl Pts',(-29.5828989554375,31.7637460255249,176.335070397434));
#34912=CARTESIAN_POINT('Ctrl Pts',(-30.8874322371387,29.8412071954588,176.223940608215));
#34913=CARTESIAN_POINT('Ctrl Pts',(-33.210175470102,29.8943721288814,176.112810818995));
#34914=CARTESIAN_POINT('Ctrl Pts',(-34.425379236641,31.8745848554147,176.001681029775));
#34915=CARTESIAN_POINT('Ctrl Pts',(-33.4209022279456,33.969576162179,175.890551240556));
#34916=CARTESIAN_POINT('Ctrl Pts',(-31.1160309092789,34.2620327244924,175.779421451336));
#34917=CARTESIAN_POINT('Ctrl Pts',(-29.6201585161938,32.4843014680682,175.668291662116));
#34918=CARTESIAN_POINT('Ctrl Pts',(-30.3022912407822,30.2633427601015,175.557161872896));
#34919=CARTESIAN_POINT('Ctrl Pts',(-32.5381486109218,29.631753924825,175.446032083677));
#34920=CARTESIAN_POINT('Ctrl Pts',(-34.2814982083244,31.1675582149901,175.334902294457));
#34921=CARTESIAN_POINT('Ctrl Pts',(-33.9368453872864,33.4652041993407,175.223772505237));
#34922=CARTESIAN_POINT('Ctrl Pts',(-31.8196126720174,34.4219111899327,175.112642716018));
#34923=CARTESIAN_POINT('Ctrl Pts',(-29.867468483099,33.1621113240314,175.001512926798));
#34924=CARTESIAN_POINT('Ctrl Pts',(-29.8669940121071,30.8387597769491,174.890383137578));
#34925=CARTESIAN_POINT('Ctrl Pts',(-31.8186234897481,29.5781626888771,174.779253348358));
#34926=CARTESIAN_POINT('Ctrl Pts',(-33.9362467826252,30.5340048442128,174.668123559139));
#34927=CARTESIAN_POINT('Ctrl Pts',(-34.2818380177658,32.8315098680694,174.556993769919));
#34928=CARTESIAN_POINT('Ctrl Pts',(-32.53911584455,34.368026078018,174.445863980699));
#34929=CARTESIAN_POINT('Ctrl Pts',(-30.3030006968699,33.737350501538,174.33473419148));
#34930=CARTESIAN_POINT('Ctrl Pts',(-29.6199609082234,31.516670586832,174.22360440226));
#34931=CARTESIAN_POINT('Ctrl Pts',(-31.1151070859216,29.7383285095682,174.11247461304));
#34932=CARTESIAN_POINT('Ctrl Pts',(-33.4200976623203,30.0298436535415,174.00134482382));
#34933=CARTESIAN_POINT('Ctrl Pts',(-34.4254302584813,32.1244245203378,173.8902150346));
#34934=CARTESIAN_POINT('Ctrl Pts',(-33.2110353847761,34.1051334154486,173.779085245381));
#34935=CARTESIAN_POINT('Ctrl Pts',(-30.8883140600557,34.1592470379621,173.667955456161));
#34936=CARTESIAN_POINT('Ctrl Pts',(-29.5829956518403,32.2372411873918,173.556825666941));
#34937=CARTESIAN_POINT('Ctrl Pts',(-30.48969341174,30.098114774894,173.445695877722));
#34938=CARTESIAN_POINT('Ctrl Pts',(-32.7786073826223,29.6995730953269,173.334566088502));
#34939=CARTESIAN_POINT('Ctrl Pts',(-34.3549483205742,31.4063571718256,173.223436299282));
#34940=CARTESIAN_POINT('Ctrl Pts',(-33.7760660938876,33.6564367268812,173.112306510062));
#34941=CARTESIAN_POINT('Ctrl Pts',(-31.5717474387099,34.3905633528034,173.001176720843));
#34942=CARTESIAN_POINT('Ctrl Pts',(-29.7593608834192,32.93687232282,172.890046931623));
#34943=CARTESIAN_POINT('Ctrl Pts',(-29.9975829489038,30.625765902949,172.778917142403));
#34944=CARTESIAN_POINT('Ctrl Pts',(-32.068395384243,29.5723436257509,172.667787353184));
#34945=CARTESIAN_POINT('Ctrl Pts',(-34.07661310564,30.7406861354284,172.556657563964));
#34946=CARTESIAN_POINT('Ctrl Pts',(-34.1843370326867,33.0615390372716,172.445527774744));
#34947=CARTESIAN_POINT('Ctrl Pts',(-32.2929793955673,34.4108829241154,172.334397985524));
#34948=CARTESIAN_POINT('Ctrl Pts',(-30.1334901928539,33.5538129037453,172.223268196305));
#34949=CARTESIAN_POINT('Ctrl Pts',(-29.6822105241847,31.2747101642669,172.112138407085));
#34950=CARTESIAN_POINT('Ctrl Pts',(-31.3521466484014,29.6593848170106,172.001008617865));
#34951=CARTESIAN_POINT('Ctrl Pts',(-33.6149911343242,30.1861651023115,171.889878828645));
#34952=CARTESIAN_POINT('Ctrl Pts',(-34.399813247963,32.3729474157566,171.778749039426));
#34953=CARTESIAN_POINT('Ctrl Pts',(-32.9883523019571,34.2184122987475,171.667619250206));
#34954=CARTESIAN_POINT('Ctrl Pts',(-30.6723620474344,34.0336103036043,171.556489460986));
#34955=CARTESIAN_POINT('Ctrl Pts',(-29.5714116494658,31.9876702121879,171.445359671767));
#34956=CARTESIAN_POINT('Ctrl Pts',(-30.693078972962,29.9530142088661,171.334229882547));
#34957=CARTESIAN_POINT('Ctrl Pts',(-33.0108262474351,29.7917374029535,171.223100093327));
#34958=CARTESIAN_POINT('Ctrl Pts',(-34.4034763022098,31.6514385782472,171.111970304107));
#34959=CARTESIAN_POINT('Ctrl Pts',(-33.5964909098172,33.8301393867379,171.000840514888));
#34960=CARTESIAN_POINT('Ctrl Pts',(-31.3284143499829,34.3339164755211,170.889710725668));
#34961=CARTESIAN_POINT('Ctrl Pts',(-29.6749656940012,32.7017185161778,170.778580936448));
#34962=CARTESIAN_POINT('Ctrl Pts',(-30.1493632209224,30.4273153806489,170.667451147228));
#34963=CARTESIAN_POINT('Ctrl Pts',(-32.3174434587353,29.5922161536956,170.556321358009));
#34964=CARTESIAN_POINT('Ctrl Pts',(-34.1950028856446,30.9606945915516,170.445191568789));
#34965=CARTESIAN_POINT('Ctrl Pts',(-34.063719475427,33.2803340684217,170.334061779569));
#34966=CARTESIAN_POINT('Ctrl Pts',(-32.0437423814044,34.4282256905171,170.22293199035));
#34967=CARTESIAN_POINT('Ctrl Pts',(-29.9837327342869,33.3538314936623,170.11180220113));
#34968=CARTESIAN_POINT('Ctrl Pts',(-29.768989023242,31.0404253954989,170.00067241191));
#34969=CARTESIAN_POINT('Ctrl Pts',(-31.5960423638194,29.6052115692218,169.88954262269));
#34970=CARTESIAN_POINT('Ctrl Pts',(-33.7927933522913,30.3616821443936,169.778412833471));
#34971=CARTESIAN_POINT('Ctrl Pts',(-34.3487993067801,32.6175234541993,169.667283044251));
#34972=CARTESIAN_POINT('Ctrl Pts',(-32.7552096073727,34.3082139954844,169.556153255031));
#34973=CARTESIAN_POINT('Ctrl Pts',(-30.4704602652025,33.8864521196416,169.445023465811));
#34974=CARTESIAN_POINT('Ctrl Pts',(-29.5855291011564,31.7382297216221,169.333893676592));
#34975=CARTESIAN_POINT('Ctrl Pts',(-30.9102955198749,29.8295766435978,169.222763887372));
#34976=CARTESIAN_POINT('Ctrl Pts',(-33.2323476614723,29.9072714840831,169.111634098152));
#34977=CARTESIAN_POINT('Ctrl Pts',(-34.4265685875006,31.900208767657,169.000504308933));
#34978=CARTESIAN_POINT('Ctrl Pts',(-33.4000202573775,33.9844739048455,168.889374519713));
#34979=CARTESIAN_POINT('Ctrl Pts',(-31.0921885701096,34.2525700451136,168.778244730493));
#34980=CARTESIAN_POINT('Ctrl Pts',(-29.6151760590397,32.4591385080545,168.667114941274));
#34981=CARTESIAN_POINT('Ctrl Pts',(-30.32072855565,30.2455083878672,168.555985152054));
#34982=CARTESIAN_POINT('Ctrl Pts',(-32.5631320687118,29.637569963837,168.444855362834));
#34983=CARTESIAN_POINT('Ctrl Pts',(-34.290163216301,31.1917018906329,168.333725573614));
#34984=CARTESIAN_POINT('Ctrl Pts',(-33.92126183043,33.4855794790164,168.222595784395));
#34985=CARTESIAN_POINT('Ctrl Pts',(-31.7940424397143,34.4198708436861,168.111465995175));
#34986=CARTESIAN_POINT('Ctrl Pts',(-29.8553132008219,33.1395226443526,168.000336205955));
#34987=CARTESIAN_POINT('Ctrl Pts',(-29.8793780091033,30.8162956994218,167.889206416735));
#34988=CARTESIAN_POINT('Ctrl Pts',(-31.8442131747296,29.5763820510783,167.778076627516));
#34989=CARTESIAN_POINT('Ctrl Pts',(-33.951622532577,30.5545373532029,167.666946838296));
#34990=CARTESIAN_POINT('Ctrl Pts',(-34.2729285626733,32.8555642178561,167.555817049076));
#34991=CARTESIAN_POINT('Ctrl Pts',(-32.5140741057304,34.3735883477403,167.444687259856));
#34992=CARTESIAN_POINT('Ctrl Pts',(-30.2847464657706,33.7193294309385,167.333557470637));
#34993=CARTESIAN_POINT('Ctrl Pts',(-29.6251964648778,31.4915603532478,167.222427681417));
#34994=CARTESIAN_POINT('Ctrl Pts',(-31.1390486307216,29.7291066950132,167.111297892197));
#34995=CARTESIAN_POINT('Ctrl Pts',(-33.4408184251737,30.0449561346089,167.000168102977));
#34996=CARTESIAN_POINT('Ctrl Pts',(-34.4239988433692,32.1500279524596,166.889038313758));
#34997=CARTESIAN_POINT('Ctrl Pts',(-33.1886966129007,34.1178213986476,166.777908524538));
#34998=CARTESIAN_POINT('Ctrl Pts',(-30.8656448664525,34.1473555806342,166.666778735318));
#34999=CARTESIAN_POINT('Ctrl Pts',(-29.580472395857,32.2117592705426,166.555648946099));
#35000=CARTESIAN_POINT('Ctrl Pts',(-30.5101755690543,30.0821472363061,166.444519156879));
#35001=CARTESIAN_POINT('Ctrl Pts',(-32.8022294248721,29.7081731264144,166.333389367659));
#35002=CARTESIAN_POINT('Ctrl Pts',(-34.3623780347574,31.4307508392421,166.222259578439));
#35003=CARTESIAN_POINT('Ctrl Pts',(-33.7557949505109,33.6761659722066,166.11112978922));
#35004=CARTESIAN_POINT('Ctrl Pts',(-32.2875197530244,34.146181938655,166.037043263073));
#35005=CARTESIAN_POINT('Ctrl Pts',(-31.6163320011528,34.0186125009919,166.));
#35006=CARTESIAN_POINT('Ctrl Pts',(-30.7309291201472,33.079358653048,179.));
#35007=CARTESIAN_POINT('Ctrl Pts',(-30.6856061922837,33.0370771716178,179.));
#35008=CARTESIAN_POINT('Ctrl Pts',(-30.6430136212517,32.9922261022954,179.));
#35009=CARTESIAN_POINT('Ctrl Pts',(-30.6031496794869,32.945150589125,179.));
#35010=CARTESIAN_POINT('Ctrl Pts',(-30.560649505517,32.894961937153,179.));
#35011=CARTESIAN_POINT('Ctrl Pts',(-30.5212500616914,32.8422446724269,179.));
#35012=CARTESIAN_POINT('Ctrl Pts',(-30.48497810544,32.7873623072376,179.));
#35013=CARTESIAN_POINT('Ctrl Pts',(-30.45324014372,32.7393402376969,179.));
#35014=CARTESIAN_POINT('Ctrl Pts',(-30.4238969086718,32.6896592869444,179.));
#35015=CARTESIAN_POINT('Ctrl Pts',(-30.3969892258523,32.638535416209,179.));
#35016=CARTESIAN_POINT('Ctrl Pts',(-30.3834950561993,32.6128968582681,179.));
#35017=CARTESIAN_POINT('Ctrl Pts',(-30.3706137909742,32.5868950488164,179.));
#35018=CARTESIAN_POINT('Ctrl Pts',(-30.3583529184774,32.560555386827,179.));
#35019=CARTESIAN_POINT('Ctrl Pts',(-30.3527381009956,32.5484932440519,179.));
#35020=CARTESIAN_POINT('Ctrl Pts',(-30.3472527987053,32.5363585364383,179.));
#35021=CARTESIAN_POINT('Ctrl Pts',(-30.3419062704107,32.5241737280056,179.));
#35022=CARTESIAN_POINT('Ctrl Pts',(-30.3149946729871,32.462841842872,179.));
#35023=CARTESIAN_POINT('Ctrl Pts',(-30.2915438746221,32.4001344020816,179.));
#35024=CARTESIAN_POINT('Ctrl Pts',(-30.2715771012512,32.3364093590736,179.));
#35025=CARTESIAN_POINT('Ctrl Pts',(-30.2512550505768,32.2715504292317,179.));
#35026=CARTESIAN_POINT('Ctrl Pts',(-30.2345415564051,32.2056365202545,179.));
#35027=CARTESIAN_POINT('Ctrl Pts',(-30.221500425048,32.1390085160714,179.));
#35028=CARTESIAN_POINT('Ctrl Pts',(-30.210592737675,32.0832804185613,179.));
#35029=CARTESIAN_POINT('Ctrl Pts',(-30.2022547019689,32.0270518158213,179.));
#35030=CARTESIAN_POINT('Ctrl Pts',(-30.1965484750337,31.9705098819633,179.));
#35031=CARTESIAN_POINT('Ctrl Pts',(-30.1939213248785,31.9444779431711,179.));
#35032=CARTESIAN_POINT('Ctrl Pts',(-30.1918523706069,31.9183794749991,179.));
#35033=CARTESIAN_POINT('Ctrl Pts',(-30.1903494767592,31.8922323434201,179.));
#35034=CARTESIAN_POINT('Ctrl Pts',(-30.1896915558872,31.880785930464,179.));
#35035=CARTESIAN_POINT('Ctrl Pts',(-30.1891422311578,31.8693303524252,179.));
#35036=CARTESIAN_POINT('Ctrl Pts',(-30.1887025004782,31.8578813236233,179.));
#35037=CARTESIAN_POINT('Ctrl Pts',(-30.1860088953412,31.7877493900974,179.));
#35038=CARTESIAN_POINT('Ctrl Pts',(-30.1874154015388,31.7177317874487,179.));
#35039=CARTESIAN_POINT('Ctrl Pts',(-30.1929763607359,31.6481896277696,179.));
#35040=CARTESIAN_POINT('Ctrl Pts',(-30.1979465359268,31.5860354733315,179.));
#35041=CARTESIAN_POINT('Ctrl Pts',(-30.2062356846863,31.5242601439434,179.));
#35042=CARTESIAN_POINT('Ctrl Pts',(-30.2179157014571,31.4631093275663,179.));
#35043=CARTESIAN_POINT('Ctrl Pts',(-30.2306454337487,31.39646271762,179.));
#35044=CARTESIAN_POINT('Ctrl Pts',(-30.2474018272177,31.3305570843581,179.));
#35045=CARTESIAN_POINT('Ctrl Pts',(-30.26793982867,31.2656058366414,179.));
#35046=CARTESIAN_POINT('Ctrl Pts',(-30.2758705976169,31.2405248500787,179.));
#35047=CARTESIAN_POINT('Ctrl Pts',(-30.2843658062738,31.2155862217279,179.));
#35048=CARTESIAN_POINT('Ctrl Pts',(-30.2934133562222,31.1908025609492,179.));
#35049=CARTESIAN_POINT('Ctrl Pts',(-30.2973810315899,31.1799340362157,179.));
#35050=CARTESIAN_POINT('Ctrl Pts',(-30.3014548316538,31.1690958722154,179.));
#35051=CARTESIAN_POINT('Ctrl Pts',(-30.3056286457748,31.1583016836734,179.));
#35052=CARTESIAN_POINT('Ctrl Pts',(-30.3308501602472,31.0930745857145,179.));
#35053=CARTESIAN_POINT('Ctrl Pts',(-30.3597620928403,31.0293339906667,179.));
#35054=CARTESIAN_POINT('Ctrl Pts',(-30.3920519767111,30.9672985237551,179.));
#35055=CARTESIAN_POINT('Ctrl Pts',(-30.4250886868533,30.9038282509261,179.));
#35056=CARTESIAN_POINT('Ctrl Pts',(-30.461661713349,30.8421420744079,179.));
#35057=CARTESIAN_POINT('Ctrl Pts',(-30.5014925323278,30.7824778732566,179.));
#35058=CARTESIAN_POINT('Ctrl Pts',(-30.5319853636164,30.7368014230525,179.));
#35059=CARTESIAN_POINT('Ctrl Pts',(-30.5643887377804,30.6923099804802,179.));
#35060=CARTESIAN_POINT('Ctrl Pts',(-30.5985972405943,30.6491163876609,179.));
#35061=CARTESIAN_POINT('Ctrl Pts',(-30.6198995701376,30.6222188600665,179.));
#35062=CARTESIAN_POINT('Ctrl Pts',(-30.6419022174088,30.5958247363827,179.));
#35063=CARTESIAN_POINT('Ctrl Pts',(-30.6645826385146,30.569962958019,179.));
#35064=CARTESIAN_POINT('Ctrl Pts',(-30.6772410040684,30.555529017711,179.));
#35065=CARTESIAN_POINT('Ctrl Pts',(-30.6901149391436,30.5412563906713,179.));
#35066=CARTESIAN_POINT('Ctrl Pts',(-30.7031769103107,30.5271754384393,179.));
#35067=CARTESIAN_POINT('Ctrl Pts',(-30.7540414015774,30.4723429432007,179.));
#35068=CARTESIAN_POINT('Ctrl Pts',(-30.807802406251,30.4203555265443,179.));
#35069=CARTESIAN_POINT('Ctrl Pts',(-30.8641752460904,30.3714768709713,179.));
#35070=CARTESIAN_POINT('Ctrl Pts',(-30.9063225488272,30.3349326149134,179.));
#35071=CARTESIAN_POINT('Ctrl Pts',(-30.9499309830963,30.3001263070555,179.));
#35072=CARTESIAN_POINT('Ctrl Pts',(-30.9948979518231,30.2671778872202,179.));
#35073=CARTESIAN_POINT('Ctrl Pts',(-31.0089817993794,30.2568583007477,179.));
#35074=CARTESIAN_POINT('Ctrl Pts',(-31.0231990077974,30.2467210444674,179.));
#35075=CARTESIAN_POINT('Ctrl Pts',(-31.0375466674535,30.2367700313995,179.));
#35076=CARTESIAN_POINT('Ctrl Pts',(-31.0513256752561,30.2272134145022,179.));
#35077=CARTESIAN_POINT('Ctrl Pts',(-31.0652179378318,30.217833529893,179.));
#35078=CARTESIAN_POINT('Ctrl Pts',(-31.079215554219,30.2086365513038,179.));
#35079=CARTESIAN_POINT('Ctrl Pts',(-31.14216376158,30.1672771298632,179.));
#35080=CARTESIAN_POINT('Ctrl Pts',(-31.2072699777245,30.1295929755988,179.));
#35081=CARTESIAN_POINT('Ctrl Pts',(-31.2742731900079,30.095863022087,179.));
#35082=CARTESIAN_POINT('Ctrl Pts',(-31.325457897845,30.0700962303613,179.));
#35083=CARTESIAN_POINT('Ctrl Pts',(-31.377750599829,30.0466373808211,179.));
#35084=CARTESIAN_POINT('Ctrl Pts',(-31.4310487708202,30.0256260323555,179.));
#35085=CARTESIAN_POINT('Ctrl Pts',(-31.4435331822408,30.0207043940728,179.));
#35086=CARTESIAN_POINT('Ctrl Pts',(-31.4560728052128,30.0159171103945,179.));
#35087=CARTESIAN_POINT('Ctrl Pts',(-31.4686656825472,30.0112635882184,179.));
#35088=CARTESIAN_POINT('Ctrl Pts',(-33.6673324606655,31.9986966424362,177.87148036339));
#35089=CARTESIAN_POINT('Ctrl Pts',(-33.6680686829516,31.9130455012085,177.877220944861));
#35090=CARTESIAN_POINT('Ctrl Pts',(-33.662038537116,31.8274983445442,177.882961526332));
#35091=CARTESIAN_POINT('Ctrl Pts',(-33.6488812040635,31.7430618526376,177.888702107803));
#35092=CARTESIAN_POINT('Ctrl Pts',(-33.5639785592561,31.1982036011571,177.925745370876));
#35093=CARTESIAN_POINT('Ctrl Pts',(-33.1823025849659,30.6995930022293,177.962788633949));
#35094=CARTESIAN_POINT('Ctrl Pts',(-32.6785051495444,30.475384701481,177.999831897022));
#35095=CARTESIAN_POINT('Ctrl Pts',(-32.1747077141229,30.2511764007327,178.036875160096));
#35096=CARTESIAN_POINT('Ctrl Pts',(-31.5487888175701,30.3013703981639,178.073918423169));
#35097=CARTESIAN_POINT('Ctrl Pts',(-31.0871675644347,30.6030121611142,178.110961686242));
#35098=CARTESIAN_POINT('Ctrl Pts',(-30.6255463112993,30.9046539240644,178.148004949315));
#35099=CARTESIAN_POINT('Ctrl Pts',(-30.3282227015813,31.4577434525337,178.185048212389));
#35100=CARTESIAN_POINT('Ctrl Pts',(-30.3312463118135,32.0091615381739,178.222091475462));
#35101=CARTESIAN_POINT('Ctrl Pts',(-30.3342699220457,32.5605796238141,178.259134738535));
#35102=CARTESIAN_POINT('Ctrl Pts',(-30.637640752228,33.1103262666252,178.296178001608));
#35103=CARTESIAN_POINT('Ctrl Pts',(-31.1025462928267,33.4068982848914,178.333221264682));
#35104=CARTESIAN_POINT('Ctrl Pts',(-31.5674518334255,33.7034703031577,178.370264527755));
#35105=CARTESIAN_POINT('Ctrl Pts',(-32.1938920844407,33.746867696879,178.407307790828));
#35106=CARTESIAN_POINT('Ctrl Pts',(-32.6951944109623,33.5171141652731,178.444351053901));
#35107=CARTESIAN_POINT('Ctrl Pts',(-33.1964967374839,33.2873606336673,178.481394316975));
#35108=CARTESIAN_POINT('Ctrl Pts',(-33.5726611395119,32.7844561767342,178.518437580048));
#35109=CARTESIAN_POINT('Ctrl Pts',(-33.6515913698567,32.2387672136962,178.555480843121));
#35110=CARTESIAN_POINT('Ctrl Pts',(-33.6629550719668,32.1602035658563,178.560814016544));
#35111=CARTESIAN_POINT('Ctrl Pts',(-33.668157767428,32.08075308988,178.566147189967));
#35112=CARTESIAN_POINT('Ctrl Pts',(-33.6674973548511,32.0012179185931,178.57148036339));
#35113=CARTESIAN_POINT('Ctrl Pts',(-32.5301702171895,30.0148256743285,179.));
#35114=CARTESIAN_POINT('Ctrl Pts',(-33.1902397907536,30.1911070339307,178.962956736927));
#35115=CARTESIAN_POINT('Ctrl Pts',(-34.3091777184327,31.251637720013,178.88887021078));
#35116=CARTESIAN_POINT('Ctrl Pts',(-33.8814411350113,33.5378731234361,178.77774042156));
#35117=CARTESIAN_POINT('Ctrl Pts',(-31.7283973209264,34.4129390290683,178.666610632341));
#35118=CARTESIAN_POINT('Ctrl Pts',(-29.8255894209646,33.0815150230766,178.555480843121));
#35119=CARTESIAN_POINT('Ctrl Pts',(-29.9119598436444,30.7594178093493,178.444351053902));
#35120=CARTESIAN_POINT('Ctrl Pts',(-31.9096840054244,29.5731212000867,178.333221264681));
#35121=CARTESIAN_POINT('Ctrl Pts',(-33.9898669259929,30.6076649759035,178.222091475462));
#35122=CARTESIAN_POINT('Ctrl Pts',(-34.249042199873,32.9165631725329,178.110961686242));
#35123=CARTESIAN_POINT('Ctrl Pts',(-32.4498708069788,34.3865813639729,177.999831897023));
#35124=CARTESIAN_POINT('Ctrl Pts',(-30.239005926868,33.6724513835904,177.888702107803));
#35125=CARTESIAN_POINT('Ctrl Pts',(-29.6397722337213,31.4276996511778,177.777572318583));
#35126=CARTESIAN_POINT('Ctrl Pts',(-31.2005990409054,29.7067170736135,177.666442529363));
#35127=CARTESIAN_POINT('Ctrl Pts',(-33.4930261644715,30.0845191734353,177.555312740144));
#35128=CARTESIAN_POINT('Ctrl Pts',(-34.4190532951284,32.2153500204183,177.444182950924));
#35129=CARTESIAN_POINT('Ctrl Pts',(-33.1311884148471,34.1490941434474,177.333053161704));
#35130=CARTESIAN_POINT('Ctrl Pts',(-30.8080724930038,34.1160109663009,177.221923372484));
#35131=CARTESIAN_POINT('Ctrl Pts',(-29.5757955383114,32.1463773261312,177.110793583265));
#35132=CARTESIAN_POINT('Ctrl Pts',(-30.5621242967963,30.0427808298698,176.999663794045));
#35133=CARTESIAN_POINT('Ctrl Pts',(-32.8643812668194,29.7304100510143,176.888534004825));
#35134=CARTESIAN_POINT('Ctrl Pts',(-34.3755658943906,31.4951434013914,176.777404215606));
#35135=CARTESIAN_POINT('Ctrl Pts',(-33.7126583679654,33.7219160257557,176.666274426386));
#35136=CARTESIAN_POINT('Ctrl Pts',(-31.4823444807967,34.3728097817195,176.555144637166));
#35137=CARTESIAN_POINT('Ctrl Pts',(-29.7257833087973,32.8521337550634,176.444014847946));
#35138=CARTESIAN_POINT('Ctrl Pts',(-30.0505605908462,30.5515941579779,176.332885058727));
#35139=CARTESIAN_POINT('Ctrl Pts',(-32.1594436788161,29.5766198796149,176.221755269507));
#35140=CARTESIAN_POINT('Ctrl Pts',(-34.1224056412966,30.8194968072545,176.110625480287));
#35141=CARTESIAN_POINT('Ctrl Pts',(-34.1429649772614,33.1427574547287,175.999495691067));
#35142=CARTESIAN_POINT('Ctrl Pts',(-32.2023060055888,34.4201788723936,175.888365901848));
#35143=CARTESIAN_POINT('Ctrl Pts',(-30.0764987714868,33.4826788317565,175.777236112628));
#35144=CARTESIAN_POINT('Ctrl Pts',(-29.7110590022335,31.1882472032951,175.666106323408));
#35145=CARTESIAN_POINT('Ctrl Pts',(-31.4404332115969,29.6367229312773,175.554976534189));
#35146=CARTESIAN_POINT('Ctrl Pts',(-33.6819168774615,30.2480442038859,175.443846744969));
#35147=CARTESIAN_POINT('Ctrl Pts',(-34.3841284567005,32.4627364219267,175.332716955749));
#35148=CARTESIAN_POINT('Ctrl Pts',(-32.9044115271646,34.2539372847887,175.221587166529));
#35149=CARTESIAN_POINT('Ctrl Pts',(-30.5969869759018,33.9823591875437,175.11045737731));
#35150=CARTESIAN_POINT('Ctrl Pts',(-29.5735847292512,31.8965474596491,174.99932758809));
#35151=CARTESIAN_POINT('Ctrl Pts',(-30.7708114250119,29.9054143747875,174.88819779887));
#35152=CARTESIAN_POINT('Ctrl Pts',(-33.0929781746067,29.8312233392852,174.77706800965));
#35153=CARTESIAN_POINT('Ctrl Pts',(-34.4148631516561,31.7418731842655,174.665938220431));
#35154=CARTESIAN_POINT('Ctrl Pts',(-33.5266915604102,33.8887578917373,174.554808431211));
#35155=CARTESIAN_POINT('Ctrl Pts',(-31.2413084093575,34.3070718594175,174.443678641991));
#35156=CARTESIAN_POINT('Ctrl Pts',(-29.650271574393,32.6139786805113,174.332548852772));
#35157=CARTESIAN_POINT('Ctrl Pts',(-30.2096807128004,30.3589788715227,174.221419063552));
#35158=CARTESIAN_POINT('Ctrl Pts',(-32.4075706476486,29.6058238031834,174.110289274332));
#35159=CARTESIAN_POINT('Ctrl Pts',(-34.2324563456884,31.0437928264109,173.999159485112));
#35160=CARTESIAN_POINT('Ctrl Pts',(-34.0142222061352,33.3568722852722,173.888029695893));
#35161=CARTESIAN_POINT('Ctrl Pts',(-31.9525937468572,34.4281569433195,173.776899906673));
#35162=CARTESIAN_POINT('Ctrl Pts',(-29.9343509763561,33.2772186991064,173.665770117453));
#35163=CARTESIAN_POINT('Ctrl Pts',(-29.8065677912631,30.9573837523311,173.554640328233));
#35164=CARTESIAN_POINT('Ctrl Pts',(-31.6861899768242,29.59173988872,173.443510539014));
#35165=CARTESIAN_POINT('Ctrl Pts',(-33.8530076924679,30.430109562459,173.332380749794));
#35166=CARTESIAN_POINT('Ctrl Pts',(-34.3239728629966,32.7052259398826,173.221250960574));
#35167=CARTESIAN_POINT('Ctrl Pts',(-32.6680632717471,34.3349271849826,173.110121171355));
#35168=CARTESIAN_POINT('Ctrl Pts',(-30.4007494190391,33.8277283916173,172.998991382135));
#35169=CARTESIAN_POINT('Ctrl Pts',(-29.5970523548762,31.6478123951331,172.887861592915));
#35170=CARTESIAN_POINT('Ctrl Pts',(-30.9925069166485,29.7902146753074,172.776731803695));
#35171=CARTESIAN_POINT('Ctrl Pts',(-33.3100082224966,29.9549885205165,172.665602014476));
#35172=CARTESIAN_POINT('Ctrl Pts',(-34.4286042095633,31.9913346945228,172.554472225256));
#35173=CARTESIAN_POINT('Ctrl Pts',(-33.3245679611538,34.0356112621306,172.443342436036));
#35174=CARTESIAN_POINT('Ctrl Pts',(-31.0083014790376,34.2169184779213,172.332212646816));
#35175=CARTESIAN_POINT('Ctrl Pts',(-29.5996267287836,32.3693259441983,172.221082857597));
#35176=CARTESIAN_POINT('Ctrl Pts',(-30.3877475653827,30.183730311518,172.109953068377));
#35177=CARTESIAN_POINT('Ctrl Pts',(-32.6513843459939,29.660365001112,171.998823279157));
#35178=CARTESIAN_POINT('Ctrl Pts',(-34.3188812371206,31.2782082694031,171.887693489938));
#35179=CARTESIAN_POINT('Ctrl Pts',(-33.8641631672544,33.5566275020312,171.776563700718));
#35180=CARTESIAN_POINT('Ctrl Pts',(-31.7033831827247,34.4104381257226,171.665433911498));
#35181=CARTESIAN_POINT('Ctrl Pts',(-29.81406369269,33.0582419168657,171.554304122278));
#35182=CARTESIAN_POINT('Ctrl Pts',(-29.9252894056131,30.7375541818489,171.443174333058));
#35183=CARTESIAN_POINT('Ctrl Pts',(-31.9352677552198,29.5722431689493,171.332044543839));
#35184=CARTESIAN_POINT('Ctrl Pts',(-34.0044883532572,30.6287888799007,171.220914754619));
#35185=CARTESIAN_POINT('Ctrl Pts',(-34.2392229481647,32.9402521378016,171.1097849654));
#35186=CARTESIAN_POINT('Ctrl Pts',(-32.4246449842735,34.3912068357963,170.99865517618));
#35187=CARTESIAN_POINT('Ctrl Pts',(-30.2214365358583,33.6537549692286,170.88752538696));
#35188=CARTESIAN_POINT('Ctrl Pts',(-29.645950082108,31.4028044890487,170.77639559774));
#35189=CARTESIAN_POINT('Ctrl Pts',(-31.224864584604,29.6984008641758,170.665265808521));
#35190=CARTESIAN_POINT('Ctrl Pts',(-33.513174613277,30.1003958086059,170.554136019301));
#35191=CARTESIAN_POINT('Ctrl Pts',(-34.4166436455741,32.2408879086503,170.443006230081));
#35192=CARTESIAN_POINT('Ctrl Pts',(-33.1084266208509,34.1609220070185,170.331876440861));
#35193=CARTESIAN_POINT('Ctrl Pts',(-30.7857895731111,34.1033037187868,170.220746651641));
#35194=CARTESIAN_POINT('Ctrl Pts',(-29.5743847404962,32.1207646765004,170.109616862422));
#35195=CARTESIAN_POINT('Ctrl Pts',(-30.582876688677,30.0277031119193,169.998487073202));
#35196=CARTESIAN_POINT('Ctrl Pts',(-32.8883045233183,29.7396662706405,169.887357283983));
#35197=CARTESIAN_POINT('Ctrl Pts',(-34.38076569148,31.520262346173,169.776227494762));
#35198=CARTESIAN_POINT('Ctrl Pts',(-33.6943759171282,33.7399091199497,169.665097705543));
#35199=CARTESIAN_POINT('Ctrl Pts',(-31.4573116781621,34.3672099356773,169.553967916323));
#35200=CARTESIAN_POINT('Ctrl Pts',(-29.7169099061327,32.8280658895954,169.442838127104));
#35201=CARTESIAN_POINT('Ctrl Pts',(-30.0659674289288,30.5310849213574,169.331708337884));
#35202=CARTESIAN_POINT('Ctrl Pts',(-32.1850305870609,29.5784391033703,169.220578548664));
#35203=CARTESIAN_POINT('Ctrl Pts',(-34.134755758485,30.8419795572488,169.109448759444));
#35204=CARTESIAN_POINT('Ctrl Pts',(-34.130775610212,33.1653277621151,168.998318970225));
#35205=CARTESIAN_POINT('Ctrl Pts',(-32.1767327307596,34.4221806365661,168.887189181005));
#35206=CARTESIAN_POINT('Ctrl Pts',(-30.0609459727286,33.4622800598482,168.776059391785));
#35207=CARTESIAN_POINT('Ctrl Pts',(-29.7197604322381,31.1641166302031,168.664929602565));
#35208=CARTESIAN_POINT('Ctrl Pts',(-31.4654254161029,29.6309445956577,168.553799813346));
#35209=CARTESIAN_POINT('Ctrl Pts',(-33.7003272617103,30.2659063761577,168.442670024126));
#35210=CARTESIAN_POINT('Ctrl Pts',(-34.3791080371299,32.4878918350693,168.331540234906));
#35211=CARTESIAN_POINT('Ctrl Pts',(-32.880554936408,34.2633639788494,168.220410445686));
#35212=CARTESIAN_POINT('Ctrl Pts',(-30.5761275089639,33.9674299515833,168.109280656467));
#35213=CARTESIAN_POINT('Ctrl Pts',(-29.5748127402796,31.870925374144,167.998150867247));
#35214=CARTESIAN_POINT('Ctrl Pts',(-30.7930030593313,29.8925484830768,167.887021078027));
#35215=CARTESIAN_POINT('Ctrl Pts',(-33.1158238734678,29.8428883892604,167.775891288808));
#35216=CARTESIAN_POINT('Ctrl Pts',(-34.4174548111338,31.7673934012069,167.664761499588));
#35217=CARTESIAN_POINT('Ctrl Pts',(-33.5066572568647,33.9047775465331,167.553631710368));
#35218=CARTESIAN_POINT('Ctrl Pts',(-31.2169834524517,34.2989297408903,167.442501921148));
#35219=CARTESIAN_POINT('Ctrl Pts',(-29.6439176314904,32.5891267679911,167.331372131929));
#35220=CARTESIAN_POINT('Ctrl Pts',(-30.2271133920415,30.3401605499161,167.220242342709));
#35221=CARTESIAN_POINT('Ctrl Pts',(-32.4328346333002,29.6102630575578,167.109112553489));
#35222=CARTESIAN_POINT('Ctrl Pts',(-34.2424325857273,31.0674235171078,166.997982764269));
#35223=CARTESIAN_POINT('Ctrl Pts',(-33.9997759247107,33.3780747465314,166.88685297505));
#35224=CARTESIAN_POINT('Ctrl Pts',(-31.9269554489549,34.4275128925295,166.77572318583));
#35225=CARTESIAN_POINT('Ctrl Pts',(-29.9209653652486,33.2553461090702,166.66459339661));
#35226=CARTESIAN_POINT('Ctrl Pts',(-29.8177243014505,30.9342420640658,166.553463607391));
#35227=CARTESIAN_POINT('Ctrl Pts',(-31.7115987485412,29.5886264481624,166.442333818171));
#35228=CARTESIAN_POINT('Ctrl Pts',(-33.8695768412099,30.4496328495725,166.331204028951));
#35229=CARTESIAN_POINT('Ctrl Pts',(-34.3162087590077,32.7300089698471,166.220074239731));
#35230=CARTESIAN_POINT('Ctrl Pts',(-32.6437429291296,34.3412897758451,166.108944450512));
#35231=CARTESIAN_POINT('Ctrl Pts',(-30.3807637468038,33.811890847881,165.997814661292));
#35232=CARTESIAN_POINT('Ctrl Pts',(-29.6025033676946,31.6200556152572,165.886684872072));
#35233=CARTESIAN_POINT('Ctrl Pts',(-30.5427968191108,30.398337297745,165.812598345926));
#35234=CARTESIAN_POINT('Ctrl Pts',(-31.1673980508617,30.1214975228147,165.775555082853));
#35235=CARTESIAN_POINT('Ctrl Pts',(-32.4967348970886,30.1400211999975,179.074814972382));
#35236=CARTESIAN_POINT('Ctrl Pts',(-33.1151770144782,30.3051853306512,179.037771709309));
#35237=CARTESIAN_POINT('Ctrl Pts',(-34.1635488360803,31.2988333782593,178.963685183163));
#35238=CARTESIAN_POINT('Ctrl Pts',(-33.7627875694947,33.4408867622834,178.852555393943));
#35239=CARTESIAN_POINT('Ctrl Pts',(-31.7455260132231,34.2607664131702,178.741425604723));
#35240=CARTESIAN_POINT('Ctrl Pts',(-29.9627191792645,33.0133090020325,178.630295815503));
#35241=CARTESIAN_POINT('Ctrl Pts',(-30.0436426291873,30.8376554419268,178.519166026284));
#35242=CARTESIAN_POINT('Ctrl Pts',(-31.9153798066803,29.7261729311921,178.408036237064));
#35243=CARTESIAN_POINT('Ctrl Pts',(-33.8643754602866,30.6954729396651,178.296906447845));
#35244=CARTESIAN_POINT('Ctrl Pts',(-34.1072057793514,32.858759882056,178.185776658625));
#35245=CARTESIAN_POINT('Ctrl Pts',(-32.4214995896834,34.2360710009532,178.074646869405));
#35246=CARTESIAN_POINT('Ctrl Pts',(-30.3500634676767,33.5669778101029,177.963517080185));
#35247=CARTESIAN_POINT('Ctrl Pts',(-29.7886206003743,31.4637919187861,177.852387290965));
#35248=CARTESIAN_POINT('Ctrl Pts',(-31.25101346648,29.8513435468475,177.741257501746));
#35249=CARTESIAN_POINT('Ctrl Pts',(-33.3988680882353,30.2053194607901,177.630127712526));
#35250=CARTESIAN_POINT('Ctrl Pts',(-34.2664950814802,32.2017689164012,177.518997923306));
#35251=CARTESIAN_POINT('Ctrl Pts',(-33.0598497286692,34.0135609726213,177.407868134087));
#35252=CARTESIAN_POINT('Ctrl Pts',(-30.8832417055349,33.9825641944877,177.296738344867));
#35253=CARTESIAN_POINT('Ctrl Pts',(-29.7286786115939,32.1371460026882,177.185608555647));
#35254=CARTESIAN_POINT('Ctrl Pts',(-30.6528042951125,30.1662133565176,177.074478766427));
#35255=CARTESIAN_POINT('Ctrl Pts',(-32.8098688415486,29.8735423205797,176.963348977208));
#35256=CARTESIAN_POINT('Ctrl Pts',(-34.2257502247723,31.5269823116739,176.852219187988));
#35257=CARTESIAN_POINT('Ctrl Pts',(-33.6046491307433,33.6133229519815,176.741089398768));
#35258=CARTESIAN_POINT('Ctrl Pts',(-31.5149905582741,34.2231679270505,176.629959609549));
#35259=CARTESIAN_POINT('Ctrl Pts',(-29.8692073650418,32.7983937222482,176.518829820329));
#35260=CARTESIAN_POINT('Ctrl Pts',(-30.1735024848817,30.642938242187,176.407700031109));
#35261=CARTESIAN_POINT('Ctrl Pts',(-32.1493883225051,29.7294509656026,176.296570241889));
#35262=CARTESIAN_POINT('Ctrl Pts',(-33.9885555876722,30.8939455424907,176.18544045267));
#35263=CARTESIAN_POINT('Ctrl Pts',(-34.0078183438655,33.0706891640971,176.07431066345));
#35264=CARTESIAN_POINT('Ctrl Pts',(-32.1895475256971,34.2675496739277,175.96318087423));
#35265=CARTESIAN_POINT('Ctrl Pts',(-30.1978048675381,33.3891733126998,175.85205108501));
#35266=CARTESIAN_POINT('Ctrl Pts',(-29.8554116506306,31.2394406006621,175.740921295791));
#35267=CARTESIAN_POINT('Ctrl Pts',(-31.4757224339665,29.7857636029674,175.629791506571));
#35268=CARTESIAN_POINT('Ctrl Pts',(-33.5758463601864,30.358531743447,175.518661717351));
#35269=CARTESIAN_POINT('Ctrl Pts',(-34.2337727869041,32.43355383134,175.407531928131));
#35270=CARTESIAN_POINT('Ctrl Pts',(-32.8473745833052,34.1117921544871,175.296402138912));
#35271=CARTESIAN_POINT('Ctrl Pts',(-30.6854683504597,33.8573411992795,175.185272349692));
#35272=CARTESIAN_POINT('Ctrl Pts',(-29.7266072277715,31.903071720518,175.074142560472));
#35273=CARTESIAN_POINT('Ctrl Pts',(-30.8483305163088,30.037509951995,174.963012771253));
#35274=CARTESIAN_POINT('Ctrl Pts',(-33.0240492269848,29.9679977930878,174.851882982033));
#35275=CARTESIAN_POINT('Ctrl Pts',(-34.2625691904757,31.7581520178003,174.740753192813));
#35276=CARTESIAN_POINT('Ctrl Pts',(-33.4304103673845,33.7696428930898,174.629623403593));
#35277=CARTESIAN_POINT('Ctrl Pts',(-31.2891554882174,34.1615757836016,174.518493614374));
#35278=CARTESIAN_POINT('Ctrl Pts',(-29.7984577974461,32.5752579582744,174.407363825154));
#35279=CARTESIAN_POINT('Ctrl Pts',(-30.3225876557211,30.4624702879473,174.296234035934));
#35280=CARTESIAN_POINT('Ctrl Pts',(-32.3818671007008,29.7568131362754,174.185104246715));
#35281=CARTESIAN_POINT('Ctrl Pts',(-34.0916659162954,31.1040962759357,174.073974457495));
#35282=CARTESIAN_POINT('Ctrl Pts',(-33.8871947684688,33.2713007881883,173.962844668275));
#35283=CARTESIAN_POINT('Ctrl Pts',(-31.9555834343146,34.275024605774,173.851714879055));
#35284=CARTESIAN_POINT('Ctrl Pts',(-30.0646216593981,33.1966705757697,173.740585089835));
#35285=CARTESIAN_POINT('Ctrl Pts',(-29.9448971534963,31.0231366121732,173.629455300616));
#35286=CARTESIAN_POINT('Ctrl Pts',(-31.7059804860523,29.7436174274733,173.518325511396));
#35287=CARTESIAN_POINT('Ctrl Pts',(-33.7361472892644,30.5291151036999,173.407195722177));
#35288=CARTESIAN_POINT('Ctrl Pts',(-34.177410921075,32.6607506859378,173.296065932956));
#35289=CARTESIAN_POINT('Ctrl Pts',(-32.625931690956,34.1876744059483,173.184936143737));
#35290=CARTESIAN_POINT('Ctrl Pts',(-30.5016065652205,33.7124622339759,173.073806354517));
#35291=CARTESIAN_POINT('Ctrl Pts',(-29.7485948615951,31.6700231963484,172.962676565298));
#35292=CARTESIAN_POINT('Ctrl Pts',(-31.0560447251658,29.9295753509734,172.851546776078));
#35293=CARTESIAN_POINT('Ctrl Pts',(-33.2273922194961,30.0839576915672,172.740416986858));
#35294=CARTESIAN_POINT('Ctrl Pts',(-34.2754436650579,31.991881174225,172.629287197638));
#35295=CARTESIAN_POINT('Ctrl Pts',(-33.2410337445178,33.9072349181872,172.518157408419));
#35296=CARTESIAN_POINT('Ctrl Pts',(-31.0708431994455,34.0771079481258,172.407027619199));
#35297=CARTESIAN_POINT('Ctrl Pts',(-29.7510068819548,32.3460343092375,172.295897829979));
#35298=CARTESIAN_POINT('Ctrl Pts',(-30.4894246767843,30.2982738231208,172.184768040759));
#35299=CARTESIAN_POINT('Ctrl Pts',(-32.6103046259136,29.8079146796321,172.07363825154));
#35300=CARTESIAN_POINT('Ctrl Pts',(-34.1726403998848,31.3237282491686,171.96250846232));
#35301=CARTESIAN_POINT('Ctrl Pts',(-33.7465992411855,33.4584583912043,171.8513786731));
#35302=CARTESIAN_POINT('Ctrl Pts',(-31.7220893980333,34.2584232299324,171.74024888388));
#35303=CARTESIAN_POINT('Ctrl Pts',(-29.951920323986,32.9915036202065,171.629119094661));
#35304=CARTESIAN_POINT('Ctrl Pts',(-30.0561315589275,30.8171706496765,171.517989305441));
#35305=CARTESIAN_POINT('Ctrl Pts',(-31.9393501107632,29.7253502733125,171.406859516221));
#35306=CARTESIAN_POINT('Ctrl Pts',(-33.8780747835076,30.7152646592637,171.295729727002));
#35307=CARTESIAN_POINT('Ctrl Pts',(-34.0980057812589,32.8809548966822,171.184599937782));
#35308=CARTESIAN_POINT('Ctrl Pts',(-32.3978646399272,34.2404047662152,171.073470148562));
#35309=CARTESIAN_POINT('Ctrl Pts',(-30.3336020947966,33.549460489886,170.962340359342));
#35310=CARTESIAN_POINT('Ctrl Pts',(-29.7944088411753,31.4404667764125,170.851210570123));
#35311=CARTESIAN_POINT('Ctrl Pts',(-31.2737486974702,29.8435518012811,170.740080780903));
#35312=CARTESIAN_POINT('Ctrl Pts',(-33.417745869973,30.2201948319103,170.628950991683));
#35313=CARTESIAN_POINT('Ctrl Pts',(-34.2642373970902,32.2256962511919,170.517821202463));
#35314=CARTESIAN_POINT('Ctrl Pts',(-33.0385234130226,34.0246429089565,170.406691413244));
#35315=CARTESIAN_POINT('Ctrl Pts',(-30.8623640636741,33.9706583327822,170.295561624024));
#35316=CARTESIAN_POINT('Ctrl Pts',(-29.7273567861031,32.1131486213453,170.184431834805));
#35317=CARTESIAN_POINT('Ctrl Pts',(-30.6722479321011,30.1520865186989,170.073302045584));
#35318=CARTESIAN_POINT('Ctrl Pts',(-32.8322833717686,29.882214794352,169.962172256365));
#35319=CARTESIAN_POINT('Ctrl Pts',(-34.2306220953308,31.55051712379,169.851042467145));
#35320=CARTESIAN_POINT('Ctrl Pts',(-33.5875196673356,33.6301813070964,169.739912677925));
#35321=CARTESIAN_POINT('Ctrl Pts',(-31.4915364557286,34.2179212367286,169.628782888706));
#35322=CARTESIAN_POINT('Ctrl Pts',(-29.8608935657816,32.7758437028605,169.517653099486));
#35323=CARTESIAN_POINT('Ctrl Pts',(-30.1879376867873,30.6237224258101,169.406523310266));
#35324=CARTESIAN_POINT('Ctrl Pts',(-32.1733615858492,29.7311554595474,169.295393521047));
#35325=CARTESIAN_POINT('Ctrl Pts',(-34.0001268415671,30.9150104121167,169.184263731827));
#35326=CARTESIAN_POINT('Ctrl Pts',(-33.9963977023611,33.0918360692859,169.073133942607));
#35327=CARTESIAN_POINT('Ctrl Pts',(-32.1655870359738,34.2694251963316,168.962004153387));
#35328=CARTESIAN_POINT('Ctrl Pts',(-30.1832329100044,33.3700609945497,168.850874364168));
#35329=CARTESIAN_POINT('Ctrl Pts',(-29.8635643227304,31.2168318283228,168.739744574948));
#35330=CARTESIAN_POINT('Ctrl Pts',(-31.4991384987148,29.7803496795589,168.628614785728));
#35331=CARTESIAN_POINT('Ctrl Pts',(-33.5930956888523,30.3752674332642,168.517484996508));
#35332=CARTESIAN_POINT('Ctrl Pts',(-34.2290689813755,32.4571228119305,168.406355207289));
#35333=CARTESIAN_POINT('Ctrl Pts',(-32.8250225145353,34.1206243516802,168.295225418069));
#35334=CARTESIAN_POINT('Ctrl Pts',(-30.6659243911297,33.8433534793964,168.184095628849));
#35335=CARTESIAN_POINT('Ctrl Pts',(-29.7277577939708,31.8790654983767,168.07296583963));
#35336=CARTESIAN_POINT('Ctrl Pts',(-30.8691226295443,30.0254554510298,167.96183605041));
#35337=CARTESIAN_POINT('Ctrl Pts',(-33.0454541560146,29.9789271837081,167.85070626119));
#35338=CARTESIAN_POINT('Ctrl Pts',(-34.2649974062867,31.782062795745,167.73957647197));
#35339=CARTESIAN_POINT('Ctrl Pts',(-33.4116395323068,33.7846522642661,167.628446682751));
#35340=CARTESIAN_POINT('Ctrl Pts',(-31.2663645909291,34.1539471498579,167.517316893531));
#35341=CARTESIAN_POINT('Ctrl Pts',(-29.7925045675747,32.5519733379621,167.406187104311));
#35342=CARTESIAN_POINT('Ctrl Pts',(-30.3389209385952,30.4448387485972,167.295057315091));
#35343=CARTESIAN_POINT('Ctrl Pts',(-32.4055378066472,29.7609724279394,167.183927525872));
#35344=CARTESIAN_POINT('Ctrl Pts',(-34.1010130022092,31.1262366910907,167.072797736652));
#35345=CARTESIAN_POINT('Ctrl Pts',(-33.8736595454705,33.2911661108151,166.961667947432));
#35346=CARTESIAN_POINT('Ctrl Pts',(-31.9315620222151,34.2744211722114,166.850538158213));
#35347=CARTESIAN_POINT('Ctrl Pts',(-30.0520802152725,33.1761773862083,166.739408368993));
#35348=CARTESIAN_POINT('Ctrl Pts',(-29.9553500755206,31.0014543603864,166.628278579773));
#35349=CARTESIAN_POINT('Ctrl Pts',(-31.729786847094,29.7407003368394,166.517148790553));
#35350=CARTESIAN_POINT('Ctrl Pts',(-33.7516715004109,30.5474071497272,166.406019001334));
#35351=CARTESIAN_POINT('Ctrl Pts',(-34.1701364622864,32.6839707677904,166.294889212114));
#35352=CARTESIAN_POINT('Ctrl Pts',(-32.6031451169547,34.1936357383937,166.183759422894));
#35353=CARTESIAN_POINT('Ctrl Pts',(-30.4828812945072,33.6976234889787,166.072629633674));
#35354=CARTESIAN_POINT('Ctrl Pts',(-29.7537021048984,31.6440169048818,165.961499844455));
#35355=CARTESIAN_POINT('Ctrl Pts',(-30.6346957097416,30.4993465649716,165.887413318308));
#35356=CARTESIAN_POINT('Ctrl Pts',(-31.2199063053497,30.2399657611253,165.850370055235));
#35357=CARTESIAN_POINT('Ctrl Pts',(-32.4632995769876,30.2652167256664,179.149629944765));
#35358=CARTESIAN_POINT('Ctrl Pts',(-33.0401142382028,30.4192636273717,179.112586681692));
#35359=CARTESIAN_POINT('Ctrl Pts',(-34.0179199537279,31.3460290365056,179.038500155545));
#35360=CARTESIAN_POINT('Ctrl Pts',(-33.6441340039781,33.3439004011306,178.927370366325));
#35361=CARTESIAN_POINT('Ctrl Pts',(-31.7626547055198,34.108593797272,178.816240577106));
#35362=CARTESIAN_POINT('Ctrl Pts',(-30.0998489375644,32.9451029809884,178.705110787886));
#35363=CARTESIAN_POINT('Ctrl Pts',(-30.1753254147303,30.9158930745042,178.593980998666));
#35364=CARTESIAN_POINT('Ctrl Pts',(-31.9210756079361,29.8792246622974,178.482851209446));
#35365=CARTESIAN_POINT('Ctrl Pts',(-33.7388839945804,30.7832809034267,178.371721420227));
#35366=CARTESIAN_POINT('Ctrl Pts',(-33.9653693588297,32.8009565915792,178.260591631007));
#35367=CARTESIAN_POINT('Ctrl Pts',(-32.393128372388,34.0855606379334,178.149461841787));
#35368=CARTESIAN_POINT('Ctrl Pts',(-30.4611210084854,33.4615042366153,178.038332052568));
#35369=CARTESIAN_POINT('Ctrl Pts',(-29.9374689670273,31.4998841863944,177.927202263348));
#35370=CARTESIAN_POINT('Ctrl Pts',(-31.3014278920546,29.9959700200815,177.816072474128));
#35371=CARTESIAN_POINT('Ctrl Pts',(-33.3047100119993,30.3261197481449,177.704942684909));
#35372=CARTESIAN_POINT('Ctrl Pts',(-34.1139368678319,32.188187812384,177.593812895689));
#35373=CARTESIAN_POINT('Ctrl Pts',(-32.9885110424914,33.8780278017951,177.482683106469));
#35374=CARTESIAN_POINT('Ctrl Pts',(-30.958410918066,33.8491174226745,177.371553317249));
#35375=CARTESIAN_POINT('Ctrl Pts',(-29.8815616848764,32.1279146792452,177.26042352803));
#35376=CARTESIAN_POINT('Ctrl Pts',(-30.7434842934286,30.2896458831653,177.14929373881));
#35377=CARTESIAN_POINT('Ctrl Pts',(-32.7553564162777,30.016674590145,177.03816394959));
#35378=CARTESIAN_POINT('Ctrl Pts',(-34.075934555154,31.5588212219564,176.927034160371));
#35379=CARTESIAN_POINT('Ctrl Pts',(-33.4966398935211,33.5047298782074,176.815904371151));
#35380=CARTESIAN_POINT('Ctrl Pts',(-31.5476366357516,34.0735260723815,176.704774581931));
#35381=CARTESIAN_POINT('Ctrl Pts',(-30.0126314212863,32.7446536894331,176.593644792711));
#35382=CARTESIAN_POINT('Ctrl Pts',(-30.2964443789173,30.7342823263961,176.482515003492));
#35383=CARTESIAN_POINT('Ctrl Pts',(-32.1393329661942,29.8822820515903,176.371385214272));
#35384=CARTESIAN_POINT('Ctrl Pts',(-33.8547055340479,30.9683942777269,176.260255425052));
#35385=CARTESIAN_POINT('Ctrl Pts',(-33.8726717104697,32.9986208734656,176.149125635832));
#35386=CARTESIAN_POINT('Ctrl Pts',(-32.1767890458053,34.1149204754619,176.037995846613));
#35387=CARTESIAN_POINT('Ctrl Pts',(-30.3191109635895,33.2956677936431,175.926866057393));
#35388=CARTESIAN_POINT('Ctrl Pts',(-29.9997642990276,31.290633998029,175.815736268173));
#35389=CARTESIAN_POINT('Ctrl Pts',(-31.5110116563361,29.9348042746576,175.704606478953));
#35390=CARTESIAN_POINT('Ctrl Pts',(-33.4697758429112,30.4690192830081,175.593476689734));
#35391=CARTESIAN_POINT('Ctrl Pts',(-34.0834171171077,32.4043712407533,175.482346900514));
#35392=CARTESIAN_POINT('Ctrl Pts',(-32.7903376394458,33.9696470241855,175.371217111294));
#35393=CARTESIAN_POINT('Ctrl Pts',(-30.7739497250175,33.7323232110152,175.260087322075));
#35394=CARTESIAN_POINT('Ctrl Pts',(-29.8796297262918,31.909595981387,175.148957532855));
#35395=CARTESIAN_POINT('Ctrl Pts',(-30.9258496076056,30.1696055292025,175.037827743635));
#35396=CARTESIAN_POINT('Ctrl Pts',(-32.9551202793629,30.1047722468905,174.926697954415));
#35397=CARTESIAN_POINT('Ctrl Pts',(-34.1102752292953,31.7744308513351,174.815568165196));
#35398=CARTESIAN_POINT('Ctrl Pts',(-33.3341291743586,33.6505278944423,174.704438375976));
#35399=CARTESIAN_POINT('Ctrl Pts',(-31.3370025670773,34.0160797077856,174.593308586756));
#35400=CARTESIAN_POINT('Ctrl Pts',(-29.9466440204991,32.5365372360375,174.482178797537));
#35401=CARTESIAN_POINT('Ctrl Pts',(-30.4354945986418,30.5659617043719,174.371049008317));
#35402=CARTESIAN_POINT('Ctrl Pts',(-32.3561635537529,29.9078024693675,174.259919219097));
#35403=CARTESIAN_POINT('Ctrl Pts',(-33.9508754869023,31.1643997254604,174.148789429877));
#35404=CARTESIAN_POINT('Ctrl Pts',(-33.7601673308024,33.1857292911044,174.037659640658));
#35405=CARTESIAN_POINT('Ctrl Pts',(-31.9585731217721,34.1218922682283,173.926529851438));
#35406=CARTESIAN_POINT('Ctrl Pts',(-30.19489234244,33.1161224524332,173.815400062218));
#35407=CARTESIAN_POINT('Ctrl Pts',(-30.0832265157296,31.0888894720152,173.704270272998));
#35408=CARTESIAN_POINT('Ctrl Pts',(-31.7257709952805,29.8954949662266,173.593140483779));
#35409=CARTESIAN_POINT('Ctrl Pts',(-33.619286886061,30.6281206449407,173.482010694559));
#35410=CARTESIAN_POINT('Ctrl Pts',(-34.0308489791535,32.6162754319929,173.370880905339));
#35411=CARTESIAN_POINT('Ctrl Pts',(-32.5838001101648,34.040421626914,173.25975111612));
#35412=CARTESIAN_POINT('Ctrl Pts',(-30.6024637114019,33.5971960763345,173.1486213269));
#35413=CARTESIAN_POINT('Ctrl Pts',(-29.900137368314,31.6922339975638,173.03749153768));
#35414=CARTESIAN_POINT('Ctrl Pts',(-31.1195825336831,30.0689360266394,172.92636174846));
#35415=CARTESIAN_POINT('Ctrl Pts',(-33.1447762164956,30.2129268626179,172.815231959241));
#35416=CARTESIAN_POINT('Ctrl Pts',(-34.1222831205525,31.9924276539272,172.704102170021));
#35417=CARTESIAN_POINT('Ctrl Pts',(-33.1574995278817,33.7788585742437,172.592972380801));
#35418=CARTESIAN_POINT('Ctrl Pts',(-31.1333849198533,33.9372974183303,172.481842591581));
#35419=CARTESIAN_POINT('Ctrl Pts',(-29.902387035126,32.3227426742766,172.370712802361));
#35420=CARTESIAN_POINT('Ctrl Pts',(-30.5911017881859,30.4128173347236,172.259583013142));
#35421=CARTESIAN_POINT('Ctrl Pts',(-32.5692249058332,29.9554643581522,172.148453223922));
#35422=CARTESIAN_POINT('Ctrl Pts',(-34.026399562649,31.3692482289342,172.037323434703));
#35423=CARTESIAN_POINT('Ctrl Pts',(-33.6290353151166,33.3602892803774,171.926193645483));
#35424=CARTESIAN_POINT('Ctrl Pts',(-31.7407956133418,34.1064083341423,171.815063856263));
#35425=CARTESIAN_POINT('Ctrl Pts',(-30.0897769552821,32.9247653235473,171.703934067043));
#35426=CARTESIAN_POINT('Ctrl Pts',(-30.1869737122419,30.8967871175041,171.592804277824));
#35427=CARTESIAN_POINT('Ctrl Pts',(-31.9434324663065,29.8784573776757,171.481674488604));
#35428=CARTESIAN_POINT('Ctrl Pts',(-33.7516612137581,30.8017404386267,171.370544699384));
#35429=CARTESIAN_POINT('Ctrl Pts',(-33.9567886143531,32.8216576555628,171.259414910164));
#35430=CARTESIAN_POINT('Ctrl Pts',(-32.371084295581,34.089602696634,171.148285120945));
#35431=CARTESIAN_POINT('Ctrl Pts',(-30.4457676537348,33.4451660105434,171.037155331725));
#35432=CARTESIAN_POINT('Ctrl Pts',(-29.9428676002425,31.4781290637763,170.926025542505));
#35433=CARTESIAN_POINT('Ctrl Pts',(-31.3226328103364,29.9887027383865,170.814895753285));
#35434=CARTESIAN_POINT('Ctrl Pts',(-33.322317126669,30.3399938552148,170.703765964066));
#35435=CARTESIAN_POINT('Ctrl Pts',(-34.1118311486063,32.2105045937335,170.592636174846));
#35436=CARTESIAN_POINT('Ctrl Pts',(-32.9686202051942,33.8883638108946,170.481506385626));
#35437=CARTESIAN_POINT('Ctrl Pts',(-30.9389385542372,33.8380129467777,170.370376596406));
#35438=CARTESIAN_POINT('Ctrl Pts',(-29.8803288317099,32.1055325661903,170.259246807187));
#35439=CARTESIAN_POINT('Ctrl Pts',(-30.7616191755252,30.2764699254786,170.148117017967));
#35440=CARTESIAN_POINT('Ctrl Pts',(-32.776262220219,30.0247633180635,170.036987228747));
#35441=CARTESIAN_POINT('Ctrl Pts',(-34.0804784991816,31.5807719014069,169.925857439528));
#35442=CARTESIAN_POINT('Ctrl Pts',(-33.4806634175431,33.5204534942432,169.814727650308));
#35443=CARTESIAN_POINT('Ctrl Pts',(-31.5257612332951,34.0686325377799,169.703597861088));
#35444=CARTESIAN_POINT('Ctrl Pts',(-30.0048772254305,32.7236215161257,169.592468071868));
#35445=CARTESIAN_POINT('Ctrl Pts',(-30.3099079446457,30.7163599302627,169.481338282649));
#35446=CARTESIAN_POINT('Ctrl Pts',(-32.1616925846373,29.8838718157245,169.370208493429));
#35447=CARTESIAN_POINT('Ctrl Pts',(-33.8654979246492,30.9880412669846,169.259078704209));
#35448=CARTESIAN_POINT('Ctrl Pts',(-33.8620197945103,33.0183443764568,169.14794891499));
#35449=CARTESIAN_POINT('Ctrl Pts',(-32.1544413411881,34.1166697560972,169.03681912577));
#35450=CARTESIAN_POINT('Ctrl Pts',(-30.3055198472801,33.2778419292513,168.92568933655));
#35451=CARTESIAN_POINT('Ctrl Pts',(-30.0073682132228,31.2695470264423,168.81455954733));
#35452=CARTESIAN_POINT('Ctrl Pts',(-31.5328515813266,29.9297547634601,168.703429758111));
#35453=CARTESIAN_POINT('Ctrl Pts',(-33.4858641159943,30.4846284903707,168.592299968891));
#35454=CARTESIAN_POINT('Ctrl Pts',(-34.0790299256211,32.4263537887917,168.481170179671));
#35455=CARTESIAN_POINT('Ctrl Pts',(-32.7694900926627,33.977884724511,168.370040390452));
#35456=CARTESIAN_POINT('Ctrl Pts',(-30.7557212732955,33.7192770072096,168.258910601232));
#35457=CARTESIAN_POINT('Ctrl Pts',(-29.880702847662,31.8872056226094,168.147780812012));
#35458=CARTESIAN_POINT('Ctrl Pts',(-30.9452421997572,30.1583624189827,168.036651022792));
#35459=CARTESIAN_POINT('Ctrl Pts',(-32.9750844385614,30.114965978156,167.925521233572));
#35460=CARTESIAN_POINT('Ctrl Pts',(-34.1125400014398,31.796732190283,167.814391444353));
#35461=CARTESIAN_POINT('Ctrl Pts',(-33.3166218077489,33.664526981999,167.703261655133));
#35462=CARTESIAN_POINT('Ctrl Pts',(-31.3157457294065,34.0089645588256,167.592131865914));
#35463=CARTESIAN_POINT('Ctrl Pts',(-29.9410915036591,32.514819907933,167.481002076694));
#35464=CARTESIAN_POINT('Ctrl Pts',(-30.4507284851489,30.5495169472784,167.369872287474));
#35465=CARTESIAN_POINT('Ctrl Pts',(-32.3782409799943,29.9116817983209,167.258742498254));
#35466=CARTESIAN_POINT('Ctrl Pts',(-33.9595934186911,31.1850498650737,167.147612709035));
#35467=CARTESIAN_POINT('Ctrl Pts',(-33.7475431662303,33.2042574750988,167.036482919815));
#35468=CARTESIAN_POINT('Ctrl Pts',(-31.9361685954752,34.1213294518934,166.925353130595));
#35469=CARTESIAN_POINT('Ctrl Pts',(-30.1831950652964,33.0970086633465,166.814223341375));
#35470=CARTESIAN_POINT('Ctrl Pts',(-30.0929758495906,31.0686666567071,166.703093552155));
#35471=CARTESIAN_POINT('Ctrl Pts',(-31.7479749456469,29.8927742255163,166.591963762936));
#35472=CARTESIAN_POINT('Ctrl Pts',(-33.6337661596119,30.6451814498819,166.480833973716));
#35473=CARTESIAN_POINT('Ctrl Pts',(-34.0240641655651,32.6379325657337,166.369704184496));
#35474=CARTESIAN_POINT('Ctrl Pts',(-32.5625473047798,34.0459817009423,166.258574395277));
#35475=CARTESIAN_POINT('Ctrl Pts',(-30.5849988422104,33.5833561300764,166.147444606057));
#35476=CARTESIAN_POINT('Ctrl Pts',(-29.9049008421022,31.6679781945065,166.036314816837));
#35477=CARTESIAN_POINT('Ctrl Pts',(-30.7265946003723,30.6003558321983,165.962228290691));
#35478=CARTESIAN_POINT('Ctrl Pts',(-31.2724145598377,30.3584339994358,165.925185027618));
#35479=CARTESIAN_POINT('Ctrl Pts',(-32.4298642568866,30.3904122513353,179.224444917147));
#35480=CARTESIAN_POINT('Ctrl Pts',(-32.9650514619275,30.5333419240922,179.187401654074));
#35481=CARTESIAN_POINT('Ctrl Pts',(-33.8722910713755,31.393224694752,179.113315127928));
#35482=CARTESIAN_POINT('Ctrl Pts',(-33.5254804384615,33.2469140399779,179.002185338708));
#35483=CARTESIAN_POINT('Ctrl Pts',(-31.7797833978164,33.9564211813738,178.891055549489));
#35484=CARTESIAN_POINT('Ctrl Pts',(-30.2369786958643,32.8768969599443,178.779925760268));
#35485=CARTESIAN_POINT('Ctrl Pts',(-30.3070082002733,30.9941307070816,178.668795971049));
#35486=CARTESIAN_POINT('Ctrl Pts',(-31.9267714091919,30.0322763934028,178.557666181829));
#35487=CARTESIAN_POINT('Ctrl Pts',(-33.6133925288741,30.8710888671883,178.44653639261));
#35488=CARTESIAN_POINT('Ctrl Pts',(-33.8235329383081,32.7431533011022,178.335406603389));
#35489=CARTESIAN_POINT('Ctrl Pts',(-32.3647571550926,33.9350502749137,178.22427681417));
#35490=CARTESIAN_POINT('Ctrl Pts',(-30.5721785492941,33.3560306631277,178.11314702495));
#35491=CARTESIAN_POINT('Ctrl Pts',(-30.0863173336803,31.5359764540028,178.002017235731));
#35492=CARTESIAN_POINT('Ctrl Pts',(-31.3518423176291,30.1405964933155,177.890887446511));
#35493=CARTESIAN_POINT('Ctrl Pts',(-33.2105519357631,30.4469200354998,177.779757657291));
#35494=CARTESIAN_POINT('Ctrl Pts',(-33.9613786541837,32.1746067083669,177.668627868071));
#35495=CARTESIAN_POINT('Ctrl Pts',(-32.9171723563135,33.742494630969,177.557498078851));
#35496=CARTESIAN_POINT('Ctrl Pts',(-31.0335801305971,33.7156706508613,177.446368289632));
#35497=CARTESIAN_POINT('Ctrl Pts',(-30.0344447581588,32.1186833558022,177.335238500412));
#35498=CARTESIAN_POINT('Ctrl Pts',(-30.8341642917448,30.4130784098129,177.224108711193));
#35499=CARTESIAN_POINT('Ctrl Pts',(-32.7008439910068,30.1598068597104,177.112978921972));
#35500=CARTESIAN_POINT('Ctrl Pts',(-33.9261188855358,31.590660132239,177.001849132753));
#35501=CARTESIAN_POINT('Ctrl Pts',(-33.388630656299,33.3961368044331,176.890719343533));
#35502=CARTESIAN_POINT('Ctrl Pts',(-31.580282713229,33.9238842177125,176.779589554314));
#35503=CARTESIAN_POINT('Ctrl Pts',(-30.1560554775308,32.6909136566179,176.668459765094));
#35504=CARTESIAN_POINT('Ctrl Pts',(-30.4193862729528,30.8256264106052,176.557329975874));
#35505=CARTESIAN_POINT('Ctrl Pts',(-32.1292776098832,30.035113137578,176.446200186654));
#35506=CARTESIAN_POINT('Ctrl Pts',(-33.7208554804235,31.0428430129631,176.335070397435));
#35507=CARTESIAN_POINT('Ctrl Pts',(-33.7375250770738,32.9265525828339,176.223940608215));
#35508=CARTESIAN_POINT('Ctrl Pts',(-32.1640305659136,33.962291276996,176.112810818995));
#35509=CARTESIAN_POINT('Ctrl Pts',(-30.4404170596408,33.2021622745864,176.001681029775));
#35510=CARTESIAN_POINT('Ctrl Pts',(-30.1441169474248,31.3418273953959,175.890551240556));
#35511=CARTESIAN_POINT('Ctrl Pts',(-31.5463008787057,30.0838449463477,175.779421451336));
#35512=CARTESIAN_POINT('Ctrl Pts',(-33.3637053256361,30.5795068225691,175.668291662116));
#35513=CARTESIAN_POINT('Ctrl Pts',(-33.9330614473113,32.3751886501666,175.557161872897));
#35514=CARTESIAN_POINT('Ctrl Pts',(-32.7333006955864,33.8275018938839,175.446032083677));
#35515=CARTESIAN_POINT('Ctrl Pts',(-30.8624310995753,33.607305222751,175.334902294457));
#35516=CARTESIAN_POINT('Ctrl Pts',(-30.0326522248121,31.9161202422559,175.223772505237));
#35517=CARTESIAN_POINT('Ctrl Pts',(-31.0033686989025,30.30170110641,175.112642716018));
#35518=CARTESIAN_POINT('Ctrl Pts',(-32.886191331741,30.2415467006931,175.001512926798));
#35519=CARTESIAN_POINT('Ctrl Pts',(-33.9579812681149,31.7907096848698,174.890383137578));
#35520=CARTESIAN_POINT('Ctrl Pts',(-33.2378479813328,33.5314128957948,174.779253348358));
#35521=CARTESIAN_POINT('Ctrl Pts',(-31.3848496459372,33.8705836319696,174.668123559139));
#35522=CARTESIAN_POINT('Ctrl Pts',(-30.0948302435522,32.4978165138007,174.556993769919));
#35523=CARTESIAN_POINT('Ctrl Pts',(-30.5484015415624,30.6694531207966,174.445863980699));
#35524=CARTESIAN_POINT('Ctrl Pts',(-32.3304600068051,30.0587918024595,174.334734191479));
#35525=CARTESIAN_POINT('Ctrl Pts',(-33.8100850575091,31.2247031749851,174.22360440226));
#35526=CARTESIAN_POINT('Ctrl Pts',(-33.633139893136,33.1001577940204,174.11247461304));
#35527=CARTESIAN_POINT('Ctrl Pts',(-31.9615628092294,33.9687599306827,174.00134482382));
#35528=CARTESIAN_POINT('Ctrl Pts',(-30.3251630254821,33.0355743290966,173.8902150346));
#35529=CARTESIAN_POINT('Ctrl Pts',(-30.2215558779629,31.1546423318572,173.779085245381));
#35530=CARTESIAN_POINT('Ctrl Pts',(-31.7455615045087,30.0473725049799,173.667955456161));
#35531=CARTESIAN_POINT('Ctrl Pts',(-33.5024264828575,30.7271261861816,173.556825666941));
#35532=CARTESIAN_POINT('Ctrl Pts',(-33.8842870372319,32.5718001780481,173.445695877722));
#35533=CARTESIAN_POINT('Ctrl Pts',(-32.5416685293737,33.8931688478798,173.334566088502));
#35534=CARTESIAN_POINT('Ctrl Pts',(-30.7033208575832,33.481929918693,173.223436299282));
#35535=CARTESIAN_POINT('Ctrl Pts',(-30.0516798750329,31.7144447987793,173.112306510063));
#35536=CARTESIAN_POINT('Ctrl Pts',(-31.1831203422005,30.2082967023054,173.001176720843));
#35537=CARTESIAN_POINT('Ctrl Pts',(-33.0621602134952,30.3418960336686,172.890046931623));
#35538=CARTESIAN_POINT('Ctrl Pts',(-33.969122576047,31.9929741336294,172.778917142403));
#35539=CARTESIAN_POINT('Ctrl Pts',(-33.0739653112457,33.6504822303003,172.667787353184));
#35540=CARTESIAN_POINT('Ctrl Pts',(-31.1959266402612,33.7974868885348,172.556657563964));
#35541=CARTESIAN_POINT('Ctrl Pts',(-30.0537671882971,32.2994510393159,172.445527774744));
#35542=CARTESIAN_POINT('Ctrl Pts',(-30.6927788995876,30.5273608463263,172.334397985524));
#35543=CARTESIAN_POINT('Ctrl Pts',(-32.5281451857529,30.1030140366724,172.223268196305));
#35544=CARTESIAN_POINT('Ctrl Pts',(-33.8801587254133,31.4147682086997,172.112138407085));
#35545=CARTESIAN_POINT('Ctrl Pts',(-33.5114713890477,33.2621201695506,172.001008617865));
#35546=CARTESIAN_POINT('Ctrl Pts',(-31.7595018286504,33.9543934383521,171.889878828646));
#35547=CARTESIAN_POINT('Ctrl Pts',(-30.2276335865782,32.8580270268881,171.778749039426));
#35548=CARTESIAN_POINT('Ctrl Pts',(-30.3178158655562,30.9764035853317,171.667619250206));
#35549=CARTESIAN_POINT('Ctrl Pts',(-31.9475148218499,30.0315644820389,171.556489460986));
#35550=CARTESIAN_POINT('Ctrl Pts',(-33.6252476440085,30.8882162179898,171.445359671767));
#35551=CARTESIAN_POINT('Ctrl Pts',(-33.8155714474473,32.7623604144434,171.334229882547));
#35552=CARTESIAN_POINT('Ctrl Pts',(-32.3443039512348,33.9388006270528,171.223100093327));
#35553=CARTESIAN_POINT('Ctrl Pts',(-30.5579332126731,33.3408715312008,171.111970304107));
#35554=CARTESIAN_POINT('Ctrl Pts',(-30.0913263593098,31.51579135114,171.000840514888));
#35555=CARTESIAN_POINT('Ctrl Pts',(-31.3715169232025,30.1338536754918,170.889710725668));
#35556=CARTESIAN_POINT('Ctrl Pts',(-33.2268883833651,30.4597928785192,170.778580936448));
#35557=CARTESIAN_POINT('Ctrl Pts',(-33.9594249001224,32.1953129362752,170.667451147229));
#35558=CARTESIAN_POINT('Ctrl Pts',(-32.8987169973659,33.7520847128326,170.556321358009));
#35559=CARTESIAN_POINT('Ctrl Pts',(-31.0155130448001,33.7053675607732,170.445191568789));
#35560=CARTESIAN_POINT('Ctrl Pts',(-30.0333008773168,32.0979165110352,170.334061779569));
#35561=CARTESIAN_POINT('Ctrl Pts',(-30.8509904189492,30.4008533322582,170.22293199035));
#35562=CARTESIAN_POINT('Ctrl Pts',(-32.7202410686693,30.167311841775,170.11180220113));
#35563=CARTESIAN_POINT('Ctrl Pts',(-33.9303349030323,31.6110266790238,170.00067241191));
#35564=CARTESIAN_POINT('Ctrl Pts',(-33.3738071677506,33.41072568139,169.88954262269));
#35565=CARTESIAN_POINT('Ctrl Pts',(-31.5599860108617,33.9193438388312,169.778412833471));
#35566=CARTESIAN_POINT('Ctrl Pts',(-30.1488608850795,32.6713993293909,169.667283044251));
#35567=CARTESIAN_POINT('Ctrl Pts',(-30.4318782025041,30.8089974347154,169.556153255031));
#35568=CARTESIAN_POINT('Ctrl Pts',(-32.1500235834255,30.0365881719016,169.445023465812));
#35569=CARTESIAN_POINT('Ctrl Pts',(-33.7308690077313,31.0610721218525,169.333893676592));
#35570=CARTESIAN_POINT('Ctrl Pts',(-33.7276418866593,32.9448526836276,169.222763887372));
#35571=CARTESIAN_POINT('Ctrl Pts',(-32.1432956464024,33.9639143158628,169.111634098152));
#35572=CARTESIAN_POINT('Ctrl Pts',(-30.4278067845557,33.1856228639528,169.000504308933));
#35573=CARTESIAN_POINT('Ctrl Pts',(-30.1511721037151,31.3222622245619,168.889374519713));
#35574=CARTESIAN_POINT('Ctrl Pts',(-31.5665646639384,30.0791598473613,168.778244730493));
#35575=CARTESIAN_POINT('Ctrl Pts',(-33.3786325431363,30.5939895474772,168.667114941273));
#35576=CARTESIAN_POINT('Ctrl Pts',(-33.9289908698666,32.3955847656529,168.555985152054));
#35577=CARTESIAN_POINT('Ctrl Pts',(-32.71395767079,33.8351450973418,168.444855362834));
#35578=CARTESIAN_POINT('Ctrl Pts',(-30.8455181554612,33.5952005350227,168.333725573614));
#35579=CARTESIAN_POINT('Ctrl Pts',(-30.0336479013533,31.8953457468421,168.222595784395));
#35580=CARTESIAN_POINT('Ctrl Pts',(-31.0213617699701,30.2912693869356,168.111465995175));
#35581=CARTESIAN_POINT('Ctrl Pts',(-32.9047147211083,30.2510047726038,168.000336205955));
#35582=CARTESIAN_POINT('Ctrl Pts',(-33.9600825965927,31.8114015848209,167.889206416735));
#35583=CARTESIAN_POINT('Ctrl Pts',(-33.221604083191,33.5444016997319,167.778076627516));
#35584=CARTESIAN_POINT('Ctrl Pts',(-31.3651268678839,33.8639819677932,167.666946838296));
#35585=CARTESIAN_POINT('Ctrl Pts',(-30.0896784397435,32.477666477904,167.555817049076));
#35586=CARTESIAN_POINT('Ctrl Pts',(-30.5625360317027,30.6541951459594,167.444687259856));
#35587=CARTESIAN_POINT('Ctrl Pts',(-32.3509441533413,30.0623911687024,167.333557470637));
#35588=CARTESIAN_POINT('Ctrl Pts',(-33.8181738351729,31.2438630390566,167.222427681417));
#35589=CARTESIAN_POINT('Ctrl Pts',(-33.6214267869902,33.1173488393825,167.111297892197));
#35590=CARTESIAN_POINT('Ctrl Pts',(-31.9407751687353,33.9682377315752,167.000168102977));
#35591=CARTESIAN_POINT('Ctrl Pts',(-30.3143099153202,33.0178399404847,166.889038313758));
#35592=CARTESIAN_POINT('Ctrl Pts',(-30.2306016236606,31.1358789530277,166.777908524538));
#35593=CARTESIAN_POINT('Ctrl Pts',(-31.7661630441998,30.0448481141933,166.666778735318));
#35594=CARTESIAN_POINT('Ctrl Pts',(-33.5158608188129,30.7429557500367,166.555648946099));
#35595=CARTESIAN_POINT('Ctrl Pts',(-33.8779918688439,32.591894363677,166.444519156879));
#35596=CARTESIAN_POINT('Ctrl Pts',(-32.5219494926048,33.8983276634909,166.333389367659));
#35597=CARTESIAN_POINT('Ctrl Pts',(-30.6871163899137,33.469088771174,166.222259578439));
#35598=CARTESIAN_POINT('Ctrl Pts',(-30.0560995793061,31.6919394841311,166.11112978922));
#35599=CARTESIAN_POINT('Ctrl Pts',(-30.8184934910031,30.7013650994249,166.037043263073));
#35600=CARTESIAN_POINT('Ctrl Pts',(-31.3249228143257,30.4769022377464,166.));
#35601=CARTESIAN_POINT('Ctrl Pts',(-33.6638666530066,32.0009462971081,178.37851963661));
#35602=CARTESIAN_POINT('Ctrl Pts',(-33.6649865931316,32.2165070141075,178.364148625536));
#35603=CARTESIAN_POINT('Ctrl Pts',(-33.6261153552445,32.4316803559838,178.349777614463));
#35604=CARTESIAN_POINT('Ctrl Pts',(-33.5453802395332,32.6297920577518,178.33540660339));
#35605=CARTESIAN_POINT('Ctrl Pts',(-33.3372743439029,33.1404522923727,178.298363340316));
#35606=CARTESIAN_POINT('Ctrl Pts',(-32.8510157494978,33.5377512836432,178.261320077243));
#35607=CARTESIAN_POINT('Ctrl Pts',(-32.3091233513288,33.6398975106474,178.22427681417));
#35608=CARTESIAN_POINT('Ctrl Pts',(-31.7672309531598,33.7420437376517,178.187233551097));
#35609=CARTESIAN_POINT('Ctrl Pts',(-31.169704751227,33.5490372003897,178.150190288023));
#35610=CARTESIAN_POINT('Ctrl Pts',(-30.7899647809916,33.1491915635712,178.11314702495));
#35611=CARTESIAN_POINT('Ctrl Pts',(-30.4102248107562,32.7493459267527,178.076103761877));
#35612=CARTESIAN_POINT('Ctrl Pts',(-30.2482710722182,32.1426611903778,178.039060498804));
#35613=CARTESIAN_POINT('Ctrl Pts',(-30.3782150336074,31.6067554954091,178.002017235731));
#35614=CARTESIAN_POINT('Ctrl Pts',(-30.5081589949966,31.0708498004404,177.964973972657));
#35615=CARTESIAN_POINT('Ctrl Pts',(-30.9300006563129,30.605723146878,177.927930709584));
#35616=CARTESIAN_POINT('Ctrl Pts',(-31.4507064233267,30.4242137437941,177.890887446511));
#35617=CARTESIAN_POINT('Ctrl Pts',(-31.9714121903405,30.2427043407103,177.853844183437));
#35618=CARTESIAN_POINT('Ctrl Pts',(-32.5909820630518,30.344812188105,177.816800920364));
#35619=CARTESIAN_POINT('Ctrl Pts',(-33.0259047858109,30.6838138906136,177.779757657291));
#35620=CARTESIAN_POINT('Ctrl Pts',(-33.4221146221702,30.9926407282283,177.746011650397));
#35621=CARTESIAN_POINT('Ctrl Pts',(-33.6650855963408,31.498066023098,177.712265643504));
#35622=CARTESIAN_POINT('Ctrl Pts',(-33.6682332709748,32.0008552724336,177.67851963661));
#35623=CARTESIAN_POINT('Ctrl Pts',(-32.5301702171895,30.0148256743285,179.));
#35624=CARTESIAN_POINT('Ctrl Pts',(-32.5988282278053,30.0402471901995,179.));
#35625=CARTESIAN_POINT('Ctrl Pts',(-32.6657829561446,30.0695594583225,179.));
#35626=CARTESIAN_POINT('Ctrl Pts',(-32.7308455855381,30.1024681354669,179.));
#35627=CARTESIAN_POINT('Ctrl Pts',(-32.7977248765802,30.1362956800508,179.));
#35628=CARTESIAN_POINT('Ctrl Pts',(-32.8626057038917,30.1739239621406,179.));
#35629=CARTESIAN_POINT('Ctrl Pts',(-32.9252517745416,30.2150779475002,179.));
#35630=CARTESIAN_POINT('Ctrl Pts',(-32.9781830386928,30.2498500001979,179.));
#35631=CARTESIAN_POINT('Ctrl Pts',(-33.0295185776569,30.2871401009452,179.));
#35632=CARTESIAN_POINT('Ctrl Pts',(-33.0790931240667,30.3268003652989,179.));
#35633=CARTESIAN_POINT('Ctrl Pts',(-33.1011284990253,30.3444289440612,179.));
#35634=CARTESIAN_POINT('Ctrl Pts',(-33.1228156494507,30.3625259776201,179.));
#35635=CARTESIAN_POINT('Ctrl Pts',(-33.1441385070898,30.381079203383,179.));
#35636=CARTESIAN_POINT('Ctrl Pts',(-33.15585001073,30.3912694965762,179.));
#35637=CARTESIAN_POINT('Ctrl Pts',(-33.1674515998752,30.4015974166315,179.));
#35638=CARTESIAN_POINT('Ctrl Pts',(-33.1789404779192,30.4120609733578,179.));
#35639=CARTESIAN_POINT('Ctrl Pts',(-33.1895353442403,30.4217103041569,179.));
#35640=CARTESIAN_POINT('Ctrl Pts',(-33.200035794986,30.4314765021164,179.));
#35641=CARTESIAN_POINT('Ctrl Pts',(-33.2104237431777,30.4413425424031,179.));
#35642=CARTESIAN_POINT('Ctrl Pts',(-33.2635074513343,30.4917592362081,179.));
#35643=CARTESIAN_POINT('Ctrl Pts',(-33.3137511250316,30.5448646877623,179.));
#35644=CARTESIAN_POINT('Ctrl Pts',(-33.3609361600621,30.6003990312448,179.));
#35645=CARTESIAN_POINT('Ctrl Pts',(-33.4077563508377,30.6555039719272,179.));
#35646=CARTESIAN_POINT('Ctrl Pts',(-33.4515655286,30.7130012726339,179.));
#35647=CARTESIAN_POINT('Ctrl Pts',(-33.4921053256574,30.7726612868285,179.));
#35648=CARTESIAN_POINT('Ctrl Pts',(-33.5257899877866,30.8222330056491,179.));
#35649=CARTESIAN_POINT('Ctrl Pts',(-33.5572168227446,30.8732985153182,179.));
#35650=CARTESIAN_POINT('Ctrl Pts',(-33.5862100224613,30.9257325420638,179.));
#35651=CARTESIAN_POINT('Ctrl Pts',(-33.5983167001639,30.9476273956384,179.));
#35652=CARTESIAN_POINT('Ctrl Pts',(-33.6099987169878,30.9697609087471,179.));
#35653=CARTESIAN_POINT('Ctrl Pts',(-33.6212418309088,30.9921240426179,179.));
#35654=CARTESIAN_POINT('Ctrl Pts',(-33.6264400720312,31.0024636125031,179.));
#35655=CARTESIAN_POINT('Ctrl Pts',(-33.6315444780314,31.0128522675599,179.));
#35656=CARTESIAN_POINT('Ctrl Pts',(-33.6365535761887,31.0232891124341,179.));
#35657=CARTESIAN_POINT('Ctrl Pts',(-33.6417882688336,31.0341960009366,179.));
#35658=CARTESIAN_POINT('Ctrl Pts',(-33.6469152729676,31.045148079228,179.));
#35659=CARTESIAN_POINT('Ctrl Pts',(-33.6519315110627,31.0561399991255,179.));
#35660=CARTESIAN_POINT('Ctrl Pts',(-33.6804723862136,31.1186806934698,179.));
#35661=CARTESIAN_POINT('Ctrl Pts',(-33.7054522348945,31.1825535423868,179.));
#35662=CARTESIAN_POINT('Ctrl Pts',(-33.726647631831,31.2475537174627,179.));
#35663=CARTESIAN_POINT('Ctrl Pts',(-33.7458439217222,31.3064232072617,179.));
#35664=CARTESIAN_POINT('Ctrl Pts',(-33.7619356534367,31.3662179954612,179.));
#35665=CARTESIAN_POINT('Ctrl Pts',(-33.7747201888406,31.4267907213557,179.));
#35666=CARTESIAN_POINT('Ctrl Pts',(-33.7898549143372,31.4984985738528,179.));
#35667=CARTESIAN_POINT('Ctrl Pts',(-33.8003553587734,31.5712981878921,179.));
#35668=CARTESIAN_POINT('Ctrl Pts',(-33.8062965723339,31.6447668899705,179.));
#35669=CARTESIAN_POINT('Ctrl Pts',(-33.8076038696773,31.6609328530473,179.));
#35670=CARTESIAN_POINT('Ctrl Pts',(-33.808690198748,31.6771311296592,179.));
#35671=CARTESIAN_POINT('Ctrl Pts',(-33.8095559901045,31.693357052552,179.));
#35672=CARTESIAN_POINT('Ctrl Pts',(-33.8104539226022,31.7101853372883,179.));
#35673=CARTESIAN_POINT('Ctrl Pts',(-33.8111146496093,31.7270495855728,179.));
#35674=CARTESIAN_POINT('Ctrl Pts',(-33.8115380877234,31.7439101956095,179.));
#35675=CARTESIAN_POINT('Ctrl Pts',(-33.8132598142794,31.8124665184444,179.));
#35676=CARTESIAN_POINT('Ctrl Pts',(-33.8110702262932,31.8810491791819,179.));
#35677=CARTESIAN_POINT('Ctrl Pts',(-33.8050898165763,31.9493201958655,179.));
#35678=CARTESIAN_POINT('Ctrl Pts',(-33.7991106222926,32.0175773374357,179.));
#35679=CARTESIAN_POINT('Ctrl Pts',(-33.7893416935654,32.0855240323565,179.));
#35680=CARTESIAN_POINT('Ctrl Pts',(-33.775853846591,32.1528074626958,179.));
#35681=CARTESIAN_POINT('Ctrl Pts',(-33.7660959099765,32.2014844272037,179.));
#35682=CARTESIAN_POINT('Ctrl Pts',(-33.7543904550383,32.2498139755358,179.));
#35683=CARTESIAN_POINT('Ctrl Pts',(-33.7407500992357,32.297652865938,179.));
#35684=CARTESIAN_POINT('Ctrl Pts',(-33.7305146132391,32.3335503381076,179.));
#35685=CARTESIAN_POINT('Ctrl Pts',(-33.7191893856383,32.3691713787597,179.));
#35686=CARTESIAN_POINT('Ctrl Pts',(-33.7067758322136,32.4044512901247,179.));
#35687=CARTESIAN_POINT('Ctrl Pts',(-33.7026466735928,32.4161865560207,179.));
#35688=CARTESIAN_POINT('Ctrl Pts',(-33.6984002925461,32.4278748826704,179.));
#35689=CARTESIAN_POINT('Ctrl Pts',(-33.6940373319631,32.4395137156836,179.));
#35690=CARTESIAN_POINT('Ctrl Pts',(-33.6709143171744,32.5011977265218,179.));
#35691=CARTESIAN_POINT('Ctrl Pts',(-33.6445184296985,32.5614980986713,179.));
#35692=CARTESIAN_POINT('Ctrl Pts',(-33.614899590325,32.62008101209,179.));
#35693=CARTESIAN_POINT('Ctrl Pts',(-33.5940729934507,32.6612738051671,179.));
#35694=CARTESIAN_POINT('Ctrl Pts',(-33.5716520331781,32.7016169140623,179.));
#35695=CARTESIAN_POINT('Ctrl Pts',(-33.5476436704819,32.740982949098,179.));
#35696=CARTESIAN_POINT('Ctrl Pts',(-33.539930599968,32.7536299174867,179.));
#35697=CARTESIAN_POINT('Ctrl Pts',(-33.5320525371695,32.7661776411531,179.));
#35698=CARTESIAN_POINT('Ctrl Pts',(-33.5240130248193,32.7786162809476,179.));
#35699=CARTESIAN_POINT('Ctrl Pts',(-33.4897680826177,32.8315996563409,179.));
#35700=CARTESIAN_POINT('Ctrl Pts',(-33.452666792504,32.8824995744465,179.));
#35701=CARTESIAN_POINT('Ctrl Pts',(-33.4127433280241,32.9310010385965,179.));
#35702=CARTESIAN_POINT('Ctrl Pts',(-33.3759774129278,32.9756665188152,179.));
#35703=CARTESIAN_POINT('Ctrl Pts',(-33.3368174942332,33.0182980198448,179.));
#35704=CARTESIAN_POINT('Ctrl Pts',(-33.2952688571158,33.0586167092817,179.));
#35705=CARTESIAN_POINT('Ctrl Pts',(-33.2874271595047,33.066226272256,179.));
#35706=CARTESIAN_POINT('Ctrl Pts',(-33.2795003199355,33.0737533467491,179.));
#35707=CARTESIAN_POINT('Ctrl Pts',(-33.2714899453066,33.081197259553,179.));
#35708=CARTESIAN_POINT('Origin',(-32.,32.,172.));
#35709=CARTESIAN_POINT('Origin',(32.,-32.,166.));
#35710=CARTESIAN_POINT('Ctrl Pts',(32.6750771856743,-33.5230977622536,166.));
#35711=CARTESIAN_POINT('Ctrl Pts',(32.7347503760542,-33.5045146947429,166.));
#35712=CARTESIAN_POINT('Ctrl Pts',(32.7931108063168,-33.4823562006339,166.));
#35713=CARTESIAN_POINT('Ctrl Pts',(32.8500021569922,-33.4569214580247,166.));
#35714=CARTESIAN_POINT('Ctrl Pts',(32.8860693067434,-33.4407967104194,166.));
#35715=CARTESIAN_POINT('Ctrl Pts',(32.9215460658915,-33.4233540969668,166.));
#35716=CARTESIAN_POINT('Ctrl Pts',(32.9563917054758,-33.404659418548,166.));
#35717=CARTESIAN_POINT('Ctrl Pts',(32.9799640056803,-33.3920128843712,166.));
#35718=CARTESIAN_POINT('Ctrl Pts',(33.0032474732066,-33.3787932129342,166.));
#35719=CARTESIAN_POINT('Ctrl Pts',(33.0262290482675,-33.3650188685718,166.));
#35720=CARTESIAN_POINT('Ctrl Pts',(33.0386995738435,-33.3575444760113,166.));
#35721=CARTESIAN_POINT('Ctrl Pts',(33.0510812979663,-33.349906528008,166.));
#35722=CARTESIAN_POINT('Ctrl Pts',(33.0633595552273,-33.3421161734122,166.));
#35723=CARTESIAN_POINT('Ctrl Pts',(33.1190572993812,-33.3067768603548,166.));
#35724=CARTESIAN_POINT('Ctrl Pts',(33.1726918020315,-33.2682673761069,166.));
#35725=CARTESIAN_POINT('Ctrl Pts',(33.2240815027149,-33.2268906436069,166.));
#35726=CARTESIAN_POINT('Ctrl Pts',(33.2611649249809,-33.1970326988656,166.));
#35727=CARTESIAN_POINT('Ctrl Pts',(33.2970793407966,-33.1656804905069,166.));
#35728=CARTESIAN_POINT('Ctrl Pts',(33.331751239224,-33.1329319505001,166.));
#35729=CARTESIAN_POINT('Ctrl Pts',(33.341130169451,-33.1240732988055,166.));
#35730=CARTESIAN_POINT('Ctrl Pts',(33.3504181471357,-33.1151124046011,166.));
#35731=CARTESIAN_POINT('Ctrl Pts',(33.3596136357983,-33.1060510586182,166.));
#35732=CARTESIAN_POINT('Ctrl Pts',(33.3693217679516,-33.0964845475258,166.));
#35733=CARTESIAN_POINT('Ctrl Pts',(33.3789213806408,-33.0868113554555,166.));
#35734=CARTESIAN_POINT('Ctrl Pts',(33.3884064304342,-33.0770387717059,166.));
#35735=CARTESIAN_POINT('Ctrl Pts',(33.4356624727154,-33.0283501890489,166.));
#35736=CARTESIAN_POINT('Ctrl Pts',(33.4801123153581,-32.9771629903732,166.));
#35737=CARTESIAN_POINT('Ctrl Pts',(33.5215724871592,-32.9237846837232,166.));
#35738=CARTESIAN_POINT('Ctrl Pts',(33.5636370688758,-32.8696282235729,166.));
#35739=CARTESIAN_POINT('Ctrl Pts',(33.6026250676343,-32.8132157239265,166.));
#35740=CARTESIAN_POINT('Ctrl Pts',(33.6383205150387,-32.7548214096818,166.));
#35741=CARTESIAN_POINT('Ctrl Pts',(33.6604358000209,-32.7186429333,166.));
#35742=CARTESIAN_POINT('Ctrl Pts',(33.6812867156679,-32.6817028484279,166.));
#35743=CARTESIAN_POINT('Ctrl Pts',(33.7008149846047,-32.6440590906012,166.));
#35744=CARTESIAN_POINT('Ctrl Pts',(33.7167940378195,-32.6132569948568,166.));
#35745=CARTESIAN_POINT('Ctrl Pts',(33.7318874487696,-32.5819836481081,166.));
#35746=CARTESIAN_POINT('Ctrl Pts',(33.7460599702932,-32.5502685810769,166.));
#35747=CARTESIAN_POINT('Ctrl Pts',(33.7518825626391,-32.5372388667638,166.));
#35748=CARTESIAN_POINT('Ctrl Pts',(33.7575505941886,-32.5241320517516,166.));
#35749=CARTESIAN_POINT('Ctrl Pts',(33.7630524074403,-32.5109727747132,166.));
#35750=CARTESIAN_POINT('Ctrl Pts',(33.7902429447907,-32.4459382492855,166.));
#35751=CARTESIAN_POINT('Ctrl Pts',(33.8134283639949,-32.3795135323734,166.));
#35752=CARTESIAN_POINT('Ctrl Pts',(33.8323972661765,-32.3119942831838,166.));
#35753=CARTESIAN_POINT('Ctrl Pts',(33.8345003970993,-32.3045082505449,166.));
#35754=CARTESIAN_POINT('Ctrl Pts',(33.8365516597232,-32.2970087243888,166.));
#35755=CARTESIAN_POINT('Ctrl Pts',(33.8385507377717,-32.289496079926,166.));
#35756=CARTESIAN_POINT('Ctrl Pts',(33.8558907757732,-32.2243312702931,166.));
#35757=CARTESIAN_POINT('Ctrl Pts',(33.8693084131536,-32.1581815103793,166.));
#35758=CARTESIAN_POINT('Ctrl Pts',(33.8789576017747,-32.0913509620122,166.));
#35759=CARTESIAN_POINT('Ctrl Pts',(33.8893365621853,-32.0194659939633,166.));
#35760=CARTESIAN_POINT('Ctrl Pts',(33.8953561186344,-31.9467925747811,166.));
#35761=CARTESIAN_POINT('Ctrl Pts',(33.8971477275179,-31.8736867160727,166.));
#35762=CARTESIAN_POINT('Ctrl Pts',(33.8974690086716,-31.860576971616,166.));
#35763=CARTESIAN_POINT('Ctrl Pts',(33.8976541694756,-31.8474532863635,166.));
#35764=CARTESIAN_POINT('Ctrl Pts',(33.8977037596136,-31.8343176784703,166.));
#35765=CARTESIAN_POINT('Ctrl Pts',(33.8977482919681,-31.822521793821,166.));
#35766=CARTESIAN_POINT('Ctrl Pts',(33.8976834443603,-31.8107249832838,166.));
#35767=CARTESIAN_POINT('Ctrl Pts',(33.8975101603586,-31.7989319884199,166.));
#35768=CARTESIAN_POINT('Ctrl Pts',(33.8964660328365,-31.7278729732675,166.));
#35769=CARTESIAN_POINT('Ctrl Pts',(33.8914891212925,-31.6569173776407,166.));
#35770=CARTESIAN_POINT('Ctrl Pts',(33.8827594412152,-31.5864004570563,166.));
#35771=CARTESIAN_POINT('Ctrl Pts',(33.8738459764261,-31.5143989537815,166.));
#35772=CARTESIAN_POINT('Ctrl Pts',(33.8610201205185,-31.4428538557896,166.));
#35773=CARTESIAN_POINT('Ctrl Pts',(33.8444208017163,-31.372105876886,166.));
#35774=CARTESIAN_POINT('Ctrl Pts',(33.8277211663871,-31.3009303387787,166.));
#35775=CARTESIAN_POINT('Ctrl Pts',(33.8072022424601,-31.230560513906,166.));
#35776=CARTESIAN_POINT('Ctrl Pts',(33.7829530935618,-31.1613424178325,166.));
#35777=CARTESIAN_POINT('Ctrl Pts',(33.776968914429,-31.1442608498207,166.));
#35778=CARTESIAN_POINT('Ctrl Pts',(33.7707573200257,-31.1272494615429,166.));
#35779=CARTESIAN_POINT('Ctrl Pts',(33.7643191706925,-31.1103135634024,166.));
#35780=CARTESIAN_POINT('Ctrl Pts',(33.7592568095487,-31.0969967501004,166.));
#35781=CARTESIAN_POINT('Ctrl Pts',(33.7540536136439,-31.0837250447109,166.));
#35782=CARTESIAN_POINT('Ctrl Pts',(33.7487184107884,-31.0705211529768,166.));
#35783=CARTESIAN_POINT('Ctrl Pts',(33.7204961745858,-31.0006750081532,166.));
#35784=CARTESIAN_POINT('Ctrl Pts',(33.6885374879799,-30.9325996700734,166.));
#35785=CARTESIAN_POINT('Ctrl Pts',(33.6530002982109,-30.8666520485507,166.));
#35786=CARTESIAN_POINT('Ctrl Pts',(33.6174247937608,-30.8006333251176,166.));
#35787=CARTESIAN_POINT('Ctrl Pts',(33.5782628944527,-30.7367457943838,166.));
#35788=CARTESIAN_POINT('Ctrl Pts',(33.535621294945,-30.6753519547081,166.));
#35789=CARTESIAN_POINT('Ctrl Pts',(33.493948975091,-30.6153536489791,166.));
#35790=CARTESIAN_POINT('Ctrl Pts',(33.4489530121136,-30.5577359733306,166.));
#35791=CARTESIAN_POINT('Ctrl Pts',(33.4006876492858,-30.5028568787942,166.));
#35792=CARTESIAN_POINT('Ctrl Pts',(33.3903602016106,-30.4911142761474,166.));
#35793=CARTESIAN_POINT('Ctrl Pts',(33.3798829091455,-30.4794971604396,166.));
#35794=CARTESIAN_POINT('Ctrl Pts',(33.3692560474651,-30.4680092249008,166.));
#35795=CARTESIAN_POINT('Ctrl Pts',(33.3601453511699,-30.4581603066688,166.));
#35796=CARTESIAN_POINT('Ctrl Pts',(33.3509247182145,-30.4484063385474,166.));
#35797=CARTESIAN_POINT('Ctrl Pts',(33.3415960097258,-30.4387477375165,166.));
#35798=CARTESIAN_POINT('Ctrl Pts',(32.3836679988471,-29.9813874990081,166.));
#35799=CARTESIAN_POINT('Ctrl Pts',(32.3093572584666,-29.9743675638755,166.));
#35800=CARTESIAN_POINT('Ctrl Pts',(32.2347977196974,-29.9717511907948,166.));
#35801=CARTESIAN_POINT('Ctrl Pts',(32.1603115654658,-29.9733742904635,166.));
#35802=CARTESIAN_POINT('Ctrl Pts',(32.087775690845,-29.9749548923253,166.));
#35803=CARTESIAN_POINT('Ctrl Pts',(32.0153086251354,-29.9805565182174,166.));
#35804=CARTESIAN_POINT('Ctrl Pts',(31.9432210973507,-29.9900715015274,166.));
#35805=CARTESIAN_POINT('Ctrl Pts',(31.927131309006,-29.9921952262863,166.));
#35806=CARTESIAN_POINT('Ctrl Pts',(31.9110583819063,-29.9945143961476,166.));
#35807=CARTESIAN_POINT('Ctrl Pts',(31.8950127157556,-29.9970270004263,166.));
#35808=CARTESIAN_POINT('Ctrl Pts',(31.8213764435297,-30.0085577658633,166.));
#35809=CARTESIAN_POINT('Ctrl Pts',(31.7484593964697,-30.0241343107327,166.));
#35810=CARTESIAN_POINT('Ctrl Pts',(31.6765936635792,-30.0436165987319,166.));
#35811=CARTESIAN_POINT('Ctrl Pts',(31.6261432264039,-30.0572933526897,166.));
#35812=CARTESIAN_POINT('Ctrl Pts',(31.5762111690267,-30.0728960169528,166.));
#35813=CARTESIAN_POINT('Ctrl Pts',(31.5269203206072,-30.0903892863566,166.));
#35814=CARTESIAN_POINT('Ctrl Pts',(31.5081989792638,-30.097033470383,166.));
#35815=CARTESIAN_POINT('Ctrl Pts',(31.4895702208887,-30.103950492905,166.));
#35816=CARTESIAN_POINT('Ctrl Pts',(31.4710411087259,-30.1111387813751,166.));
#35817=CARTESIAN_POINT('Ctrl Pts',(31.4533390621205,-30.1180062133595,166.));
#35818=CARTESIAN_POINT('Ctrl Pts',(31.4357224886101,-30.1251236957699,166.));
#35819=CARTESIAN_POINT('Ctrl Pts',(31.4182285084939,-30.1324766056846,166.));
#35820=CARTESIAN_POINT('Ctrl Pts',(31.3512969653627,-30.1606086604728,166.));
#35821=CARTESIAN_POINT('Ctrl Pts',(31.2860855769426,-30.1922088519133,166.));
#35822=CARTESIAN_POINT('Ctrl Pts',(31.2229027128029,-30.2271495142053,166.));
#35823=CARTESIAN_POINT('Ctrl Pts',(31.1610753343667,-30.2613405813522,166.));
#35824=CARTESIAN_POINT('Ctrl Pts',(31.101189679297,-30.2987309556031,166.));
#35825=CARTESIAN_POINT('Ctrl Pts',(31.0435670658395,-30.3392378236749,166.));
#35826=CARTESIAN_POINT('Ctrl Pts',(30.9872087901503,-30.3788559024312,166.));
#35827=CARTESIAN_POINT('Ctrl Pts',(30.9330147735939,-30.4214557401947,166.));
#35828=CARTESIAN_POINT('Ctrl Pts',(30.8813260918099,-30.4669870571697,166.));
#35829=CARTESIAN_POINT('Ctrl Pts',(30.8645071656146,-30.4818024448589,166.));
#35830=CARTESIAN_POINT('Ctrl Pts',(30.847953859026,-30.4969283974564,166.));
#35831=CARTESIAN_POINT('Ctrl Pts',(30.8316790249109,-30.5123636843746,166.));
#35832=CARTESIAN_POINT('Ctrl Pts',(30.8225443903146,-30.5210271033005,166.));
#35833=CARTESIAN_POINT('Ctrl Pts',(30.8134966581499,-30.5297889376287,166.));
#35834=CARTESIAN_POINT('Ctrl Pts',(30.8045505687119,-30.5386363394549,166.));
#35835=CARTESIAN_POINT('Ctrl Pts',(30.7559814459807,-30.5866696782818,166.));
#35836=CARTESIAN_POINT('Ctrl Pts',(30.7103173349291,-30.6373041034516,166.));
#35837=CARTESIAN_POINT('Ctrl Pts',(30.6678507708474,-30.6904581549245,166.));
#35838=CARTESIAN_POINT('Ctrl Pts',(30.661746870727,-30.6980982131255,166.));
#35839=CARTESIAN_POINT('Ctrl Pts',(30.655709102983,-30.7057903755372,166.));
#35840=CARTESIAN_POINT('Ctrl Pts',(30.6497384120877,-30.7135344486893,166.));
#35841=CARTESIAN_POINT('Ctrl Pts',(30.6073794462891,-30.7684746449824,166.));
#35842=CARTESIAN_POINT('Ctrl Pts',(30.5683925078902,-30.8260262206115,166.));
#35843=CARTESIAN_POINT('Ctrl Pts',(30.5328447155065,-30.885827412865,166.));
#35844=CARTESIAN_POINT('Ctrl Pts',(30.4996835114472,-30.9416137052429,166.));
#35845=CARTESIAN_POINT('Ctrl Pts',(30.4695155660164,-30.9993586633756,166.));
#35846=CARTESIAN_POINT('Ctrl Pts',(30.4424350809432,-31.0587740427515,166.));
#35847=CARTESIAN_POINT('Ctrl Pts',(30.4365397345137,-31.0717086059145,166.));
#35848=CARTESIAN_POINT('Ctrl Pts',(30.4307908557492,-31.0847223260546,166.));
#35849=CARTESIAN_POINT('Ctrl Pts',(30.4251896623469,-31.0978122019056,166.));
#35850=CARTESIAN_POINT('Ctrl Pts',(30.4206631621282,-31.1083905414929,166.));
#35851=CARTESIAN_POINT('Ctrl Pts',(30.4162333388954,-31.1190183106247,166.));
#35852=CARTESIAN_POINT('Ctrl Pts',(30.4119058547031,-31.1296809021722,166.));
#35853=CARTESIAN_POINT('Ctrl Pts',(30.386195392612,-31.1930295231227,166.));
#35854=CARTESIAN_POINT('Ctrl Pts',(30.3640425170158,-31.2577226660332,166.));
#35855=CARTESIAN_POINT('Ctrl Pts',(30.3454933793611,-31.3234107110985,166.));
#35856=CARTESIAN_POINT('Ctrl Pts',(30.3270295327823,-31.3887967149504,166.));
#35857=CARTESIAN_POINT('Ctrl Pts',(30.312136352138,-31.4551696274359,166.));
#35858=CARTESIAN_POINT('Ctrl Pts',(30.3009104203693,-31.5221872556072,166.));
#35859=CARTESIAN_POINT('Ctrl Pts',(30.2899245304527,-31.5877718592491,166.));
#35860=CARTESIAN_POINT('Ctrl Pts',(30.282450863886,-31.6539748650791,166.));
#35861=CARTESIAN_POINT('Ctrl Pts',(30.278627835107,-31.7204626904435,166.));
#35862=CARTESIAN_POINT('Ctrl Pts',(30.2778239865627,-31.7344427425749,166.));
#35863=CARTESIAN_POINT('Ctrl Pts',(30.2771817056382,-31.7484353120607,166.));
#35864=CARTESIAN_POINT('Ctrl Pts',(30.2767025483352,-31.7624371631597,166.));
#35865=CARTESIAN_POINT('Ctrl Pts',(30.2762461598509,-31.7757736678089,166.));
#35866=CARTESIAN_POINT('Ctrl Pts',(30.2759378587872,-31.7891204534951,166.));
#35867=CARTESIAN_POINT('Ctrl Pts',(30.2757789675672,-31.8024530389158,166.));
#35868=CARTESIAN_POINT('Ctrl Pts',(30.2750003669087,-31.8677855336075,166.));
#35869=CARTESIAN_POINT('Ctrl Pts',(30.2778001326965,-31.9328938376842,166.));
#35870=CARTESIAN_POINT('Ctrl Pts',(30.2842564554748,-31.9974683500875,166.));
#35871=CARTESIAN_POINT('Ctrl Pts',(30.2905902024686,-32.060816890404,166.));
#35872=CARTESIAN_POINT('Ctrl Pts',(30.3004431366813,-32.1236525831547,166.));
#35873=CARTESIAN_POINT('Ctrl Pts',(30.3139357387833,-32.1856659637692,166.));
#35874=CARTESIAN_POINT('Ctrl Pts',(30.3269907260027,-32.2456680215814,166.));
#35875=CARTESIAN_POINT('Ctrl Pts',(30.3434533492307,-32.3049008673228,166.));
#35876=CARTESIAN_POINT('Ctrl Pts',(30.363473861685,-32.3630572891802,166.));
#35877=CARTESIAN_POINT('Ctrl Pts',(30.3667806503312,-32.3726629871331,166.));
#35878=CARTESIAN_POINT('Ctrl Pts',(30.3701845915591,-32.3822392460162,166.));
#35879=CARTESIAN_POINT('Ctrl Pts',(30.3736864683761,-32.3917845902246,166.));
#35880=CARTESIAN_POINT('Ctrl Pts',(30.3774493182508,-32.4020412894562,166.));
#35881=CARTESIAN_POINT('Ctrl Pts',(30.3813252458597,-32.4122622947181,166.));
#35882=CARTESIAN_POINT('Ctrl Pts',(30.3853131952719,-32.4224462418484,166.));
#35883=CARTESIAN_POINT('Origin',(32.,-32.,180.545925280538));
#35884=CARTESIAN_POINT('Ctrl Pts',(29.9434031644741,-31.9984978685597,178.795925280538));
#35885=CARTESIAN_POINT('Ctrl Pts',(29.9425886530065,-31.900403685169,178.790592107115));
#35886=CARTESIAN_POINT('Ctrl Pts',(29.9935747042563,-31.1217949684998,178.748215670618));
#35887=CARTESIAN_POINT('Ctrl Pts',(30.988248508056,-29.7919884506806,178.668795971049));
#35888=CARTESIAN_POINT('Ctrl Pts',(33.3060963778469,-29.9525600136615,178.557666181829));
#35889=CARTESIAN_POINT('Ctrl Pts',(34.4285775821774,-31.9866392352977,178.446536392609));
#35890=CARTESIAN_POINT('Ctrl Pts',(33.3284712654795,-34.033087144352,178.33540660339));
#35891=CARTESIAN_POINT('Ctrl Pts',(31.0125524608971,-34.2188064667841,178.22427681417));
#35892=CARTESIAN_POINT('Ctrl Pts',(29.9981273513597,-32.8935904489542,178.144449706553));
#35893=CARTESIAN_POINT('Ctrl Pts',(29.9426985167512,-32.1072447552094,178.101665862009));
#35894=CARTESIAN_POINT('Ctrl Pts',(29.943606531648,-32.0016074863584,178.095925280538));
#35895=CARTESIAN_POINT('Ctrl Pts',(29.9473399238087,-32.0021821257033,178.854074719462));
#35896=CARTESIAN_POINT('Ctrl Pts',(29.950876284898,-31.5321178460643,178.828629953495));
#35897=CARTESIAN_POINT('Ctrl Pts',(30.3432698790764,-30.3707968848796,178.766141924455));
#35898=CARTESIAN_POINT('Ctrl Pts',(32.2716026642884,-29.5870613462295,178.666610632341));
#35899=CARTESIAN_POINT('Ctrl Pts',(34.1744104601116,-30.9184848843002,178.555480843121));
#35900=CARTESIAN_POINT('Ctrl Pts',(34.0880400722661,-33.2405822108959,178.444351053901));
#35901=CARTESIAN_POINT('Ctrl Pts',(32.0903159787745,-34.4268786410256,178.333221264682));
#35902=CARTESIAN_POINT('Ctrl Pts',(30.2791369268827,-33.526119436994,178.236462486535));
#35903=CARTESIAN_POINT('Ctrl Pts',(29.9500603938313,-32.4182642842386,178.176746971462));
#35904=CARTESIAN_POINT('Ctrl Pts',(29.9478812476528,-31.9988328933335,178.154074719462));
#35905=CARTESIAN_POINT('Ctrl Pts',(33.2690708798528,-30.920641346952,179.));
#35906=CARTESIAN_POINT('Ctrl Pts',(33.6279571482409,-31.3426068457268,178.962956736927));
#35907=CARTESIAN_POINT('Ctrl Pts',(33.8850557275035,-32.5658743636166,178.88887021078));
#35908=CARTESIAN_POINT('Ctrl Pts',(32.5454537305004,-33.893241966271,178.777740421561));
#35909=CARTESIAN_POINT('Ctrl Pts',(30.7060861201286,-33.483868903691,178.666610632341));
#35910=CARTESIAN_POINT('Ctrl Pts',(30.0511744258997,-31.7184481767343,178.555480843121));
#35911=CARTESIAN_POINT('Ctrl Pts',(31.1796676064832,-30.2097348868884,178.444351053901));
#35912=CARTESIAN_POINT('Ctrl Pts',(33.0589884732901,-30.339926990028,178.333221264682));
#35913=CARTESIAN_POINT('Ctrl Pts',(33.9691009864497,-31.9891670354087,178.222091475462));
#35914=CARTESIAN_POINT('Ctrl Pts',(33.07713012692,-33.6484356649181,178.110961686242));
#35915=CARTESIAN_POINT('Ctrl Pts',(31.1993733543519,-33.7990176778987,177.999831897022));
#35916=CARTESIAN_POINT('Ctrl Pts',(30.0543453845802,-32.3031858100374,177.888702107803));
#35917=CARTESIAN_POINT('Ctrl Pts',(30.6899574647931,-30.5298680270273,177.777572318583));
#35918=CARTESIAN_POINT('Ctrl Pts',(32.5245072262386,-30.102005737538,177.666442529363));
#35919=CARTESIAN_POINT('Ctrl Pts',(33.8790331908656,-31.4111639457544,177.555312740143));
#35920=CARTESIAN_POINT('Ctrl Pts',(33.5138885880054,-33.2592201303934,177.444182950924));
#35921=CARTESIAN_POINT('Ctrl Pts',(31.7632494531294,-33.9548509189774,177.333053161704));
#35922=CARTESIAN_POINT('Ctrl Pts',(30.2292819071445,-32.8614237331979,177.221923372484));
#35923=CARTESIAN_POINT('Ctrl Pts',(30.3158563296739,-30.9796306983742,177.110793583265));
#35924=CARTESIAN_POINT('Ctrl Pts',(31.9437407889795,-30.0316686763551,176.999663794045));
#35925=CARTESIAN_POINT('Ctrl Pts',(33.6231130614891,-30.8851020901988,176.888534004825));
#35926=CARTESIAN_POINT('Ctrl Pts',(33.8170298653015,-32.758878003058,176.777404215605));
#35927=CARTESIAN_POINT('Ctrl Pts',(32.3480206396625,-33.9381369861425,176.666274426386));
#35928=CARTESIAN_POINT('Ctrl Pts',(30.5605066995148,-33.3436340231644,176.555144637166));
#35929=CARTESIAN_POINT('Ctrl Pts',(30.0904014169314,-31.5194517706213,176.444014847946));
#35930=CARTESIAN_POINT('Ctrl Pts',(31.3679400490272,-30.135062047588,176.332885058727));
#35931=CARTESIAN_POINT('Ctrl Pts',(33.2239330937557,-30.4574433135484,176.221755269507));
#35932=CARTESIAN_POINT('Ctrl Pts',(33.9597958441263,-32.1915557309348,176.110625480287));
#35933=CARTESIAN_POINT('Ctrl Pts',(32.9020746910311,-33.7503584205498,175.999495691067));
#35934=CARTESIAN_POINT('Ctrl Pts',(31.0187845633079,-33.7072520656006,175.888365901848));
#35935=CARTESIAN_POINT('Ctrl Pts',(30.0334921624016,-32.1016871345539,175.777236112628));
#35936=CARTESIAN_POINT('Ctrl Pts',(30.8479264085786,-30.403059240733,175.666106323408));
#35937=CARTESIAN_POINT('Ctrl Pts',(32.7167259119053,-30.1659342116828,175.554976534189));
#35938=CARTESIAN_POINT('Ctrl Pts',(33.9295856332257,-31.6073263024897,175.443846744969));
#35939=CARTESIAN_POINT('Ctrl Pts',(33.3765095085026,-33.4080891028869,175.332716955749));
#35940=CARTESIAN_POINT('Ctrl Pts',(31.563666809222,-33.9201840264136,175.221587166529));
#35941=CARTESIAN_POINT('Ctrl Pts',(30.150151514305,-32.6749473524947,175.11045737731));
#35942=CARTESIAN_POINT('Ctrl Pts',(30.4295974927246,-30.8120061810721,174.99932758809));
#35943=CARTESIAN_POINT('Ctrl Pts',(32.1462588154966,-30.0363040694758,174.88819779887));
#35944=CARTESIAN_POINT('Ctrl Pts',(33.729065656437,-31.0577551780996,174.77706800965));
#35945=CARTESIAN_POINT('Ctrl Pts',(33.7294503595424,-32.9415385295071,174.665938220431));
#35946=CARTESIAN_POINT('Ctrl Pts',(32.1470608487029,-33.9636360292698,174.554808431211));
#35947=CARTESIAN_POINT('Ctrl Pts',(30.4300828439389,-33.1886351297909,174.443678641991));
#35948=CARTESIAN_POINT('Ctrl Pts',(30.1498759953595,-31.3258082497385,174.332548852772));
#35949=CARTESIAN_POINT('Ctrl Pts',(31.5628825720676,-30.0799943482204,174.221419063552));
#35950=CARTESIAN_POINT('Ctrl Pts',(33.3759342784784,-30.5913487976167,174.110289274332));
#35951=CARTESIAN_POINT('Ctrl Pts',(33.9297458546116,-32.391885551248,173.999159485112));
#35952=CARTESIAN_POINT('Ctrl Pts',(32.7174749518267,-33.833772898199,173.888029695892));
#35953=CARTESIAN_POINT('Ctrl Pts',(30.8485787538218,-33.5974111751572,173.776899906673));
#35954=CARTESIAN_POINT('Ctrl Pts',(30.0334507936758,-31.8991160678144,173.665770117453));
#35955=CARTESIAN_POINT('Ctrl Pts',(31.0180873408195,-30.2931488411672,173.554640328233));
#35956=CARTESIAN_POINT('Ctrl Pts',(32.901359705246,-30.2492732850537,173.443510539014));
#35957=CARTESIAN_POINT('Ctrl Pts',(33.9597174422702,-31.8076438326184,173.332380749794));
#35958=CARTESIAN_POINT('Ctrl Pts',(33.2245630283795,-33.542056658555,173.221250960574));
#35959=CARTESIAN_POINT('Ctrl Pts',(31.3687018107489,-33.8651959534902,173.110121171354));
#35960=CARTESIAN_POINT('Ctrl Pts',(30.0905978497772,-32.4813281389989,172.998991382135));
#35961=CARTESIAN_POINT('Ctrl Pts',(30.5599580300852,-30.6569540314822,172.887861592915));
#35962=CARTESIAN_POINT('Ctrl Pts',(32.3472290046545,-30.0617210296259,172.776731803695));
#35963=CARTESIAN_POINT('Ctrl Pts',(33.8167197597056,-31.2403799216958,172.665602014475));
#35964=CARTESIAN_POINT('Ctrl Pts',(33.6235682921796,-33.114234871693,172.554472225256));
#35965=CARTESIAN_POINT('Ctrl Pts',(31.9445447305158,-33.9683541504908,172.443342436036));
#35966=CARTESIAN_POINT('Ctrl Pts',(30.3162732300965,-33.0210570566713,172.332212646816));
#35967=CARTESIAN_POINT('Ctrl Pts',(30.2289302102365,-31.139299617489,172.221082857597));
#35968=CARTESIAN_POINT('Ctrl Pts',(31.7624510555159,-30.0452458344737,172.109953068377));
#35969=CARTESIAN_POINT('Ctrl Pts',(33.5133741186761,-30.740161865322,171.998823279157));
#35970=CARTESIAN_POINT('Ctrl Pts',(33.8792736002829,-32.5880680946519,171.887693489937));
#35971=CARTESIAN_POINT('Ctrl Pts',(32.5252822627843,-33.8977807810893,171.776563700718));
#35972=CARTESIAN_POINT('Ctrl Pts',(30.6905582948345,-33.4706650772494,171.665433911498));
#35973=CARTESIAN_POINT('Ctrl Pts',(30.0542211751481,-31.6976126434095,171.554304122278));
#35974=CARTESIAN_POINT('Ctrl Pts',(31.1986397348735,-30.2013018390669,171.443174333059));
#35975=CARTESIAN_POINT('Ctrl Pts',(33.0764545188525,-30.3511400855409,171.332044543839));
#35976=CARTESIAN_POINT('Ctrl Pts',(33.9691098008408,-32.0099970445868,171.220914754619));
#35977=CARTESIAN_POINT('Ctrl Pts',(33.0596571472062,-33.6597048168402,171.1097849654));
#35978=CARTESIAN_POINT('Ctrl Pts',(31.1804177639518,-33.7904687394708,170.99865517618));
#35979=CARTESIAN_POINT('Ctrl Pts',(30.0512511551294,-32.2826150885626,170.88752538696));
#35980=CARTESIAN_POINT('Ctrl Pts',(30.7055583558314,-30.516115173435,170.77639559774));
#35981=CARTESIAN_POINT('Ctrl Pts',(32.5445245116414,-30.1076505595188,170.665265808521));
#35982=CARTESIAN_POINT('Ctrl Pts',(33.8851477395197,-31.4310436318559,170.554136019301));
#35983=CARTESIAN_POINT('Ctrl Pts',(33.5005041997655,-33.2751394022435,170.443006230081));
#35984=CARTESIAN_POINT('Ctrl Pts',(31.7426154886764,-33.952241420009,170.331876440861));
#35985=CARTESIAN_POINT('Ctrl Pts',(30.2202822911319,-32.8426732613587,170.220746651642));
#35986=CARTESIAN_POINT('Ctrl Pts',(30.3267274405086,-30.9618996723241,170.109616862422));
#35987=CARTESIAN_POINT('Ctrl Pts',(31.9645334904465,-30.0311842454491,169.998487073202));
#35988=CARTESIAN_POINT('Ctrl Pts',(33.6347981053096,-30.9023076462213,169.887357283982));
#35989=CARTESIAN_POINT('Ctrl Pts',(33.8089132228404,-32.7780271851939,169.776227494763));
#35990=CARTESIAN_POINT('Ctrl Pts',(32.3275305756749,-33.9417046816305,169.665097705543));
#35991=CARTESIAN_POINT('Ctrl Pts',(30.5463954975727,-33.3283551103494,169.553967916323));
#35992=CARTESIAN_POINT('Ctrl Pts',(30.095583496408,-31.4993093474876,169.442838127103));
#35993=CARTESIAN_POINT('Ctrl Pts',(31.3876728267927,-30.1284902400415,169.331708337884));
#35994=CARTESIAN_POINT('Ctrl Pts',(33.2401573456871,-30.4704565692305,169.220578548664));
#35995=CARTESIAN_POINT('Ctrl Pts',(33.9576633107509,-32.2122444590535,169.109448759444));
#35996=CARTESIAN_POINT('Ctrl Pts',(32.8835370437985,-33.7597885216428,168.998318970225));
#35997=CARTESIAN_POINT('Ctrl Pts',(31.0008072559047,-33.6967932133432,168.887189181005));
#35998=CARTESIAN_POINT('Ctrl Pts',(30.032527831648,-32.0809111571343,168.776059391785));
#35999=CARTESIAN_POINT('Ctrl Pts',(30.8648575994482,-30.3909800873892,168.664929602566));
#36000=CARTESIAN_POINT('Ctrl Pts',(32.7360573822727,-30.1736065925138,168.553799813346));
#36001=CARTESIAN_POINT('Ctrl Pts',(33.9336254307537,-31.6277285378747,168.442670024126));
#36002=CARTESIAN_POINT('Ctrl Pts',(33.3615604549092,-33.4225492880192,168.331540234906));
#36003=CARTESIAN_POINT('Ctrl Pts',(31.543410115007,-33.9154683571568,168.220410445686));
#36004=CARTESIAN_POINT('Ctrl Pts',(30.1431258888499,-32.6553715572293,168.109280656467));
#36005=CARTESIAN_POINT('Ctrl Pts',(30.4422327071443,-30.7954858173387,167.998150867247));
#36006=CARTESIAN_POINT('Ctrl Pts',(32.1669912689855,-30.0379583909259,167.887021078027));
#36007=CARTESIAN_POINT('Ctrl Pts',(33.7389212112043,-31.0760701759928,167.775891288808));
#36008=CARTESIAN_POINT('Ctrl Pts',(33.7194093618925,-32.9597524994687,167.664761499588));
#36009=CARTESIAN_POINT('Ctrl Pts',(32.1263126229409,-33.9650797779653,167.553631710368));
#36010=CARTESIAN_POINT('Ctrl Pts',(30.4176161201555,-33.1719872839235,167.442501921148));
#36011=CARTESIAN_POINT('Ctrl Pts',(30.1570998197528,-31.306304880134,167.331372131929));
#36012=CARTESIAN_POINT('Ctrl Pts',(31.5831865204611,-30.0754844364286,167.220242342709));
#36013=CARTESIAN_POINT('Ctrl Pts',(33.3907348875884,-30.6059603581105,167.109112553489));
#36014=CARTESIAN_POINT('Ctrl Pts',(33.9255008417806,-32.4122450367323,166.997982764269));
#36015=CARTESIAN_POINT('Ctrl Pts',(32.6980630472242,-33.8412499830313,166.88685297505));
#36016=CARTESIAN_POINT('Ctrl Pts',(30.8317782670075,-33.5851579144293,166.77572318583));
#36017=CARTESIAN_POINT('Ctrl Pts',(30.0346113980645,-31.878356689149,166.664593396611));
#36018=CARTESIAN_POINT('Ctrl Pts',(31.0361997002367,-30.2828613829585,166.55346360739));
#36019=CARTESIAN_POINT('Ctrl Pts',(32.9197400051123,-30.2589149050105,166.442333818171));
#36020=CARTESIAN_POINT('Ctrl Pts',(33.9617632742068,-31.8283047261835,166.331204028951));
#36021=CARTESIAN_POINT('Ctrl Pts',(33.2079560627009,-33.5550031183362,166.220074239732));
#36022=CARTESIAN_POINT('Ctrl Pts',(31.3495488780108,-33.8582231808284,166.108944450512));
#36023=CARTESIAN_POINT('Ctrl Pts',(30.0845739050515,-32.4615493362111,165.997814661292));
#36024=CARTESIAN_POINT('Ctrl Pts',(30.5763937621187,-30.6409583631627,165.886684872072));
#36025=CARTESIAN_POINT('Ctrl Pts',(31.7668777668628,-30.2598665970073,165.812598345926));
#36026=CARTESIAN_POINT('Ctrl Pts',(32.3110796379508,-30.3633004372053,165.775555082853));
#36027=CARTESIAN_POINT('Ctrl Pts',(33.3677806246593,-30.8366876301908,179.074814972382));
#36028=CARTESIAN_POINT('Ctrl Pts',(33.7545814662438,-31.2914740748737,179.037771709309));
#36029=CARTESIAN_POINT('Ctrl Pts',(34.0316774590095,-32.6098887011227,178.963685183163));
#36030=CARTESIAN_POINT('Ctrl Pts',(32.587879728446,-34.0405004325351,178.852555393943));
#36031=CARTESIAN_POINT('Ctrl Pts',(30.6054440591442,-33.5992858777425,178.741425604723));
#36032=CARTESIAN_POINT('Ctrl Pts',(29.899592604785,-31.6965487627099,178.630295815504));
#36033=CARTESIAN_POINT('Ctrl Pts',(31.1158612403408,-30.0704860748191,178.519166026284));
#36034=CARTESIAN_POINT('Ctrl Pts',(33.141357774809,-30.2108046645725,178.408036237064));
#36035=CARTESIAN_POINT('Ctrl Pts',(34.1222598516922,-31.9883244353717,178.296906447844));
#36036=CARTESIAN_POINT('Ctrl Pts',(33.1609105064398,-33.7766528247294,178.185776658625));
#36037=CARTESIAN_POINT('Ctrl Pts',(31.1370997232003,-33.9389472741939,178.074646869405));
#36038=CARTESIAN_POINT('Ctrl Pts',(29.9030102041591,-32.3267679396196,177.963517080185));
#36039=CARTESIAN_POINT('Ctrl Pts',(30.5880608990545,-30.4155195267286,177.852387290966));
#36040=CARTESIAN_POINT('Ctrl Pts',(32.565303981781,-29.9543776323896,177.741257501746));
#36041=CARTESIAN_POINT('Ctrl Pts',(34.0251864827721,-31.3653636224075,177.630127712526));
#36042=CARTESIAN_POINT('Ctrl Pts',(33.6316405264983,-33.3571636729485,177.518997923307));
#36043=CARTESIAN_POINT('Ctrl Pts',(31.7448347322218,-34.1069013981196,177.407868134086));
#36044=CARTESIAN_POINT('Ctrl Pts',(30.0915534840557,-32.9284262294525,177.296738344867));
#36045=CARTESIAN_POINT('Ctrl Pts',(30.1848617614787,-30.900265238989,177.185608555647));
#36046=CARTESIAN_POINT('Ctrl Pts',(31.9393648849611,-29.8785696763417,177.074478766427));
#36047=CARTESIAN_POINT('Ctrl Pts',(33.7493606010357,-30.7983840905119,176.963348977208));
#36048=CARTESIAN_POINT('Ctrl Pts',(33.9583604695705,-32.8179043783459,176.852219187988));
#36049=CARTESIAN_POINT('Ctrl Pts',(32.3750900721692,-34.0888874369954,176.741089398768));
#36050=CARTESIAN_POINT('Ctrl Pts',(30.448541309246,-33.448143372205,176.629959609548));
#36051=CARTESIAN_POINT('Ctrl Pts',(29.941870714817,-31.4820741947568,176.518829820329));
#36052=CARTESIAN_POINT('Ctrl Pts',(31.3187777229086,-29.9900050990085,176.407700031109));
#36053=CARTESIAN_POINT('Ctrl Pts',(33.3191319713462,-30.3374615384667,176.296570241889));
#36054=CARTESIAN_POINT('Ctrl Pts',(34.1122309450475,-32.2064551487821,176.18544045267));
#36055=CARTESIAN_POINT('Ctrl Pts',(32.9722390640079,-33.8865032456776,176.07431066345));
#36056=CARTESIAN_POINT('Ctrl Pts',(30.9424645350938,-33.8400440304869,175.96318087423));
#36057=CARTESIAN_POINT('Ctrl Pts',(29.8805349951614,-32.1095964730009,175.85205108501));
#36058=CARTESIAN_POINT('Ctrl Pts',(30.7583168430193,-30.2788474119684,175.740921295791));
#36059=CARTESIAN_POINT('Ctrl Pts',(32.7724736506514,-30.0232785343702,175.629791506571));
#36060=CARTESIAN_POINT('Ctrl Pts',(34.0796709503359,-31.5767837054694,175.518661717351));
#36061=CARTESIAN_POINT('Ctrl Pts',(33.483575949365,-33.5176118397311,175.407531928131));
#36062=CARTESIAN_POINT('Ctrl Pts',(31.5297283282466,-34.0695380760871,175.296402138912));
#36063=CARTESIAN_POINT('Ctrl Pts',(30.006268241233,-32.7274455084135,175.185272349692));
#36064=CARTESIAN_POINT('Ctrl Pts',(30.3074498387223,-30.7196027002582,175.074142560473));
#36065=CARTESIAN_POINT('Ctrl Pts',(32.1576349888708,-29.8835656154959,174.963012771252));
#36066=CARTESIAN_POINT('Ctrl Pts',(33.863554306685,-30.9844663276567,174.851882982033));
#36067=CARTESIAN_POINT('Ctrl Pts',(33.863968932426,-33.014772443742,174.740753192813));
#36068=CARTESIAN_POINT('Ctrl Pts',(32.1584994051121,-34.1163698240635,174.629623403594));
#36069=CARTESIAN_POINT('Ctrl Pts',(30.307972941094,-33.2810884924772,174.518493614374));
#36070=CARTESIAN_POINT('Ctrl Pts',(30.0059712921174,-31.273368865402,174.407363825154));
#36071=CARTESIAN_POINT('Ctrl Pts',(31.528883092254,-29.9306541727243,174.296234035934));
#36072=CARTESIAN_POINT('Ctrl Pts',(33.4829559773097,-30.4817823400484,174.185104246715));
#36073=CARTESIAN_POINT('Ctrl Pts',(34.0798436339194,-32.4223668453752,174.073974457495));
#36074=CARTESIAN_POINT('Ctrl Pts',(32.7732809517312,-33.9764057941924,173.962844668275));
#36075=CARTESIAN_POINT('Ctrl Pts',(30.7590199284013,-33.721659593393,173.851714879055));
#36076=CARTESIAN_POINT('Ctrl Pts',(29.88049040873,-31.8912692033412,173.740585089836));
#36077=CARTESIAN_POINT('Ctrl Pts',(30.9417130818647,-30.1603880592551,173.629455300616));
#36078=CARTESIAN_POINT('Ctrl Pts',(32.971468465833,-30.113099813578,173.518325511396));
#36079=CARTESIAN_POINT('Ctrl Pts',(34.1121464450078,-31.7926821559338,173.407195722176));
#36080=CARTESIAN_POINT('Ctrl Pts',(33.3198109029858,-33.6619995409107,173.296065932957));
#36081=CARTESIAN_POINT('Ctrl Pts',(31.3195987353044,-34.0102729696805,173.184936143737));
#36082=CARTESIAN_POINT('Ctrl Pts',(29.942082426428,-32.5187663771014,173.073806354517));
#36083=CARTESIAN_POINT('Ctrl Pts',(30.4479499636978,-30.5524904219861,172.962676565298));
#36084=CARTESIAN_POINT('Ctrl Pts',(32.3742368629097,-29.9109595350815,172.851546776078));
#36085=CARTESIAN_POINT('Ctrl Pts',(33.9580262436163,-31.1812958269698,172.740416986858));
#36086=CARTESIAN_POINT('Ctrl Pts',(33.7498512400758,-33.2009012995383,172.629287197638));
#36087=CARTESIAN_POINT('Ctrl Pts',(31.9402313579644,-34.1214549260016,172.518157408419));
#36088=CARTESIAN_POINT('Ctrl Pts',(30.18531108888,-33.100476010409,172.407027619199));
#36089=CARTESIAN_POINT('Ctrl Pts',(30.0911744317709,-31.0723533842554,172.295897829979));
#36090=CARTESIAN_POINT('Ctrl Pts',(31.7439742343537,-29.8932028809226,172.184768040759));
#36091=CARTESIAN_POINT('Ctrl Pts',(33.6310860411722,-30.6421702537061,172.07363825154));
#36092=CARTESIAN_POINT('Ctrl Pts',(34.0254455915014,-32.6338086852473,171.96250846232));
#36093=CARTESIAN_POINT('Ctrl Pts',(32.5661393015313,-34.0453922814192,171.8513786731));
#36094=CARTESIAN_POINT('Ctrl Pts',(30.5887084623249,-33.5850550429918,171.74024888388));
#36095=CARTESIAN_POINT('Ctrl Pts',(29.9028763335792,-31.6740926184246,171.629119094661));
#36096=CARTESIAN_POINT('Ctrl Pts',(31.1363090419827,-30.0613970951568,171.517989305441));
#36097=CARTESIAN_POINT('Ctrl Pts',(33.1601823488252,-30.2228899271284,171.406859516221));
#36098=CARTESIAN_POINT('Ctrl Pts',(34.1222693516765,-32.0107746258359,171.295729727002));
#36099=CARTESIAN_POINT('Ctrl Pts',(33.1420784589262,-33.7887985038243,171.184599937782));
#36100=CARTESIAN_POINT('Ctrl Pts',(31.1166697458918,-33.9297333898248,171.073470148562));
#36101=CARTESIAN_POINT('Ctrl Pts',(29.8996753020995,-32.3045972045447,170.962340359342));
#36102=CARTESIAN_POINT('Ctrl Pts',(30.6048752447529,-30.4006969608846,170.851210570123));
#36103=CARTESIAN_POINT('Ctrl Pts',(32.5868782339104,-29.9604615149035,170.740080780903));
#36104=CARTESIAN_POINT('Ctrl Pts',(34.0317766278226,-31.386789572609,170.628950991683));
#36105=CARTESIAN_POINT('Ctrl Pts',(33.6172150856516,-33.3743211634725,170.517821202464));
#36106=CARTESIAN_POINT('Ctrl Pts',(31.7225958350595,-34.1040889294184,170.406691413244));
#36107=CARTESIAN_POINT('Ctrl Pts',(30.0818538678981,-32.9082173250549,170.295561624024));
#36108=CARTESIAN_POINT('Ctrl Pts',(30.1965784394077,-30.8811550740079,170.184431834804));
#36109=CARTESIAN_POINT('Ctrl Pts',(31.961774865879,-29.8780475658609,170.073302045585));
#36110=CARTESIAN_POINT('Ctrl Pts',(33.7619545205635,-30.8169279138221,169.962172256365));
#36111=CARTESIAN_POINT('Ctrl Pts',(33.9496125056294,-32.8385430051708,169.851042467145));
#36112=CARTESIAN_POINT('Ctrl Pts',(32.3530062682106,-34.0927326318073,169.739912677925));
#36113=CARTESIAN_POINT('Ctrl Pts',(30.4333325223188,-33.4316760485543,169.628782888706));
#36114=CARTESIAN_POINT('Ctrl Pts',(29.9474558622,-31.4603650715444,169.517653099486));
#36115=CARTESIAN_POINT('Ctrl Pts',(31.3400453380804,-29.9829221289604,169.406523310266));
#36116=CARTESIAN_POINT('Ctrl Pts',(33.3366181636415,-30.3514869796523,169.295393521046));
#36117=CARTESIAN_POINT('Ctrl Pts',(34.1099325408538,-32.228753069189,169.184263731827));
#36118=CARTESIAN_POINT('Ctrl Pts',(32.9522595379514,-33.896666830524,169.073133942607));
#36119=CARTESIAN_POINT('Ctrl Pts',(30.923088932722,-33.8287716770662,168.962004153387));
#36120=CARTESIAN_POINT('Ctrl Pts',(29.8794956576891,-32.0872045169454,168.850874364168));
#36121=CARTESIAN_POINT('Ctrl Pts',(30.7765649607498,-30.2658287286403,168.739744574948));
#36122=CARTESIAN_POINT('Ctrl Pts',(32.7933087442892,-30.0315476815174,168.628614785728));
#36123=CARTESIAN_POINT('Ctrl Pts',(34.0840249678096,-31.5987728494191,168.517484996508));
#36124=CARTESIAN_POINT('Ctrl Pts',(33.4674641417531,-33.5331967541492,168.406355207289));
#36125=CARTESIAN_POINT('Ctrl Pts',(31.5078960458211,-34.0644556168296,168.295225418069));
#36126=CARTESIAN_POINT('Ctrl Pts',(29.9986961548143,-32.7063470860153,168.184095628849));
#36127=CARTESIAN_POINT('Ctrl Pts',(30.3210678341756,-30.7017973642556,168.07296583963));
#36128=CARTESIAN_POINT('Ctrl Pts',(32.1799800356558,-29.8853486119087,167.96183605041));
#36129=CARTESIAN_POINT('Ctrl Pts',(33.8741764374659,-31.0042058864605,167.85070626119));
#36130=CARTESIAN_POINT('Ctrl Pts',(33.8531469348088,-33.0344031165493,167.73957647197));
#36131=CARTESIAN_POINT('Ctrl Pts',(32.1361373592691,-34.1179258691386,167.628446682751));
#36132=CARTESIAN_POINT('Ctrl Pts',(30.2945365416662,-33.2631457586385,167.517316893531));
#36133=CARTESIAN_POINT('Ctrl Pts',(30.0137569936081,-31.2523485020131,167.406187104311));
#36134=CARTESIAN_POINT('Ctrl Pts',(31.5507663043405,-29.9257934749763,167.295057315091));
#36135=CARTESIAN_POINT('Ctrl Pts',(33.4989077942611,-30.4975304039719,167.183927525872));
#36136=CARTESIAN_POINT('Ctrl Pts',(34.075268439268,-32.4443099142892,167.072797736652));
#36137=CARTESIAN_POINT('Ctrl Pts',(32.752359167594,-33.9844644550008,166.961667947433));
#36138=CARTESIAN_POINT('Ctrl Pts',(30.740912681033,-33.7084532604145,166.850538158212));
#36139=CARTESIAN_POINT('Ctrl Pts',(29.8817412862193,-31.8688951371095,166.739408368993));
#36140=CARTESIAN_POINT('Ctrl Pts',(30.9612342407464,-30.1493004311028,166.628278579773));
#36141=CARTESIAN_POINT('Ctrl Pts',(32.9912784058701,-30.1234913694608,166.517148790553));
#36142=CARTESIAN_POINT('Ctrl Pts',(34.1143514040283,-31.8149500767845,166.406019001334));
#36143=CARTESIAN_POINT('Ctrl Pts',(33.3019122290424,-33.6759529907359,166.294889212114));
#36144=CARTESIAN_POINT('Ctrl Pts',(31.2989560661514,-34.0027578470042,166.183759422894));
#36145=CARTESIAN_POINT('Ctrl Pts',(29.9355899325803,-32.4974491570299,166.072629633675));
#36146=CARTESIAN_POINT('Ctrl Pts',(30.4656640852527,-30.5352505927904,165.961499844455));
#36147=CARTESIAN_POINT('Ctrl Pts',(31.7487452602337,-30.1245170851199,165.887413318308));
#36148=CARTESIAN_POINT('Ctrl Pts',(32.3352757582496,-30.2359961244729,165.850370055235));
#36149=CARTESIAN_POINT('Ctrl Pts',(33.4664903694657,-30.7527339134296,179.149629944765));
#36150=CARTESIAN_POINT('Ctrl Pts',(33.8812057842467,-31.2403413040207,179.112586681692));
#36151=CARTESIAN_POINT('Ctrl Pts',(34.1782991905155,-32.653903038629,179.038500155545));
#36152=CARTESIAN_POINT('Ctrl Pts',(32.6303057263916,-34.1877588987991,178.927370366325));
#36153=CARTESIAN_POINT('Ctrl Pts',(30.5048019981598,-33.7147028517942,178.816240577106));
#36154=CARTESIAN_POINT('Ctrl Pts',(29.7480107836703,-31.6746493486853,178.705110787886));
#36155=CARTESIAN_POINT('Ctrl Pts',(31.0520548741984,-29.9312372627499,178.593980998666));
#36156=CARTESIAN_POINT('Ctrl Pts',(33.223727076328,-30.081682339117,178.482851209447));
#36157=CARTESIAN_POINT('Ctrl Pts',(34.2754187169348,-31.9874818353347,178.371721420227));
#36158=CARTESIAN_POINT('Ctrl Pts',(33.2446908859597,-33.9048699845407,178.260591631007));
#36159=CARTESIAN_POINT('Ctrl Pts',(31.0748260920487,-34.0788768704889,178.149461841788));
#36160=CARTESIAN_POINT('Ctrl Pts',(29.751675023738,-32.3503500692018,178.038332052568));
#36161=CARTESIAN_POINT('Ctrl Pts',(30.4861643333158,-30.3011710264298,177.927202263348));
#36162=CARTESIAN_POINT('Ctrl Pts',(32.6061007373232,-29.8067495272411,177.816072474128));
#36163=CARTESIAN_POINT('Ctrl Pts',(34.1713397746787,-31.3195632990606,177.704942684908));
#36164=CARTESIAN_POINT('Ctrl Pts',(33.7493924649911,-33.4551072155036,177.593812895689));
#36165=CARTESIAN_POINT('Ctrl Pts',(31.7264200113143,-34.2589518772617,177.482683106469));
#36166=CARTESIAN_POINT('Ctrl Pts',(29.953825060967,-32.9954287257072,177.371553317249));
#36167=CARTESIAN_POINT('Ctrl Pts',(30.0538671932836,-30.8208997796038,177.26042352803));
#36168=CARTESIAN_POINT('Ctrl Pts',(31.9349889809426,-29.7254706763283,177.14929373881));
#36169=CARTESIAN_POINT('Ctrl Pts',(33.8756081405823,-30.7116660908249,177.03816394959));
#36170=CARTESIAN_POINT('Ctrl Pts',(34.0996910738393,-32.8769307536337,176.92703416037));
#36171=CARTESIAN_POINT('Ctrl Pts',(32.402159504676,-34.2396378878484,176.815904371151));
#36172=CARTESIAN_POINT('Ctrl Pts',(30.3365759189771,-33.5526527212457,176.704774581931));
#36173=CARTESIAN_POINT('Ctrl Pts',(29.7933400127026,-31.4446966188922,176.593644792711));
#36174=CARTESIAN_POINT('Ctrl Pts',(31.26961539679,-29.844948150429,176.482515003491));
#36175=CARTESIAN_POINT('Ctrl Pts',(33.4143308489367,-30.2174797633851,176.371385214272));
#36176=CARTESIAN_POINT('Ctrl Pts',(34.2646660459687,-32.2213545666294,176.260255425052));
#36177=CARTESIAN_POINT('Ctrl Pts',(33.0424034369847,-34.0226480708054,176.149125635832));
#36178=CARTESIAN_POINT('Ctrl Pts',(30.8661445068797,-33.9728359953733,176.037995846613));
#36179=CARTESIAN_POINT('Ctrl Pts',(29.7275778279212,-32.1175058114478,175.926866057393));
#36180=CARTESIAN_POINT('Ctrl Pts',(30.6687072774601,-30.1546355832039,175.815736268173));
#36181=CARTESIAN_POINT('Ctrl Pts',(32.8282213893975,-29.8806228570576,175.704606478953));
#36182=CARTESIAN_POINT('Ctrl Pts',(34.229756267446,-31.5462411084492,175.593476689734));
#36183=CARTESIAN_POINT('Ctrl Pts',(33.5906423902274,-33.6271345765753,175.482346900514));
#36184=CARTESIAN_POINT('Ctrl Pts',(31.4957898472712,-34.2188921257606,175.371217111294));
#36185=CARTESIAN_POINT('Ctrl Pts',(29.8623849681609,-32.7799436643323,175.260087322075));
#36186=CARTESIAN_POINT('Ctrl Pts',(30.1853021847201,-30.6271992194443,175.148957532855));
#36187=CARTESIAN_POINT('Ctrl Pts',(32.169011162245,-29.730827161516,175.037827743635));
#36188=CARTESIAN_POINT('Ctrl Pts',(33.9980429569331,-30.9111774772138,174.926697954415));
#36189=CARTESIAN_POINT('Ctrl Pts',(33.9984875053096,-33.0880063579768,174.815568165196));
#36190=CARTESIAN_POINT('Ctrl Pts',(32.1699379615213,-34.2691036188572,174.704438375976));
#36191=CARTESIAN_POINT('Ctrl Pts',(30.1858630382491,-33.3735418551635,174.593308586756));
#36192=CARTESIAN_POINT('Ctrl Pts',(29.8620665888753,-31.2209294810654,174.482178797537));
#36193=CARTESIAN_POINT('Ctrl Pts',(31.4948836124403,-29.7813139972282,174.371049008317));
#36194=CARTESIAN_POINT('Ctrl Pts',(33.5899776761409,-30.3722158824801,174.259919219097));
#36195=CARTESIAN_POINT('Ctrl Pts',(34.2299414132272,-32.4528481395024,174.148789429877));
#36196=CARTESIAN_POINT('Ctrl Pts',(32.8290869516356,-34.1190386901857,174.037659640658));
#36197=CARTESIAN_POINT('Ctrl Pts',(30.6694611029807,-33.8459080116287,173.926529851438));
#36198=CARTESIAN_POINT('Ctrl Pts',(29.7275300237844,-31.883422338868,173.815400062218));
#36199=CARTESIAN_POINT('Ctrl Pts',(30.8653388229099,-30.0276272773431,173.704270272998));
#36200=CARTESIAN_POINT('Ctrl Pts',(33.0415772264202,-29.9769263421023,173.593140483779));
#36201=CARTESIAN_POINT('Ctrl Pts',(34.2645754477454,-31.7777204792493,173.482010694559));
#36202=CARTESIAN_POINT('Ctrl Pts',(33.4150587775922,-33.7819424232662,173.370880905339));
#36203=CARTESIAN_POINT('Ctrl Pts',(31.27049565986,-34.1553499858709,173.259751116119));
#36204=CARTESIAN_POINT('Ctrl Pts',(29.7935670030788,-32.5562046152037,173.1486213269));
#36205=CARTESIAN_POINT('Ctrl Pts',(30.3359418973104,-30.4480268124901,173.03749153768));
#36206=CARTESIAN_POINT('Ctrl Pts',(32.4012447211648,-29.7601980405371,172.92636174846));
#36207=CARTESIAN_POINT('Ctrl Pts',(34.099332727527,-31.1222117322437,172.81523195924));
#36208=CARTESIAN_POINT('Ctrl Pts',(33.8761341879719,-33.2875677273836,172.704102170021));
#36209=CARTESIAN_POINT('Ctrl Pts',(31.935917985413,-34.2745557015125,172.592972380801));
#36210=CARTESIAN_POINT('Ctrl Pts',(30.0543489476635,-33.1798949641467,172.481842591581));
#36211=CARTESIAN_POINT('Ctrl Pts',(29.9534186533055,-31.0054071510219,172.370712802362));
#36212=CARTESIAN_POINT('Ctrl Pts',(31.7254974131916,-29.7411599273715,172.259583013142));
#36213=CARTESIAN_POINT('Ctrl Pts',(33.7487979636683,-30.5441786420902,172.148453223922));
#36214=CARTESIAN_POINT('Ctrl Pts',(34.1716175827199,-32.6795492758427,172.037323434702));
#36215=CARTESIAN_POINT('Ctrl Pts',(32.6069963402783,-34.193003781749,171.926193645483));
#36216=CARTESIAN_POINT('Ctrl Pts',(30.4868586298152,-33.6994450087343,171.815063856263));
#36217=CARTESIAN_POINT('Ctrl Pts',(29.7515314920104,-31.6505725934397,171.703934067043));
#36218=CARTESIAN_POINT('Ctrl Pts',(31.073978349092,-29.9214923512466,171.592804277824));
#36219=CARTESIAN_POINT('Ctrl Pts',(33.243910178798,-30.0946397687158,171.481674488604));
#36220=CARTESIAN_POINT('Ctrl Pts',(34.2754289025122,-32.011552207085,171.370544699384));
#36221=CARTESIAN_POINT('Ctrl Pts',(33.2244997706462,-33.9178921908084,171.259414910164));
#36222=CARTESIAN_POINT('Ctrl Pts',(31.0529217278318,-34.0689980401788,171.148285120945));
#36223=CARTESIAN_POINT('Ctrl Pts',(29.7480994490696,-32.3265793205269,171.037155331725));
#36224=CARTESIAN_POINT('Ctrl Pts',(30.5041921336743,-30.2852787483341,170.926025542505));
#36225=CARTESIAN_POINT('Ctrl Pts',(32.6292319561795,-29.8132724702883,170.814895753285));
#36226=CARTESIAN_POINT('Ctrl Pts',(34.1784055161256,-31.3425355133621,170.703765964066));
#36227=CARTESIAN_POINT('Ctrl Pts',(33.7339259715377,-33.4735029247014,170.592636174846));
#36228=CARTESIAN_POINT('Ctrl Pts',(31.7025761814426,-34.2559364388279,170.481506385626));
#36229=CARTESIAN_POINT('Ctrl Pts',(29.9434254446643,-32.973761388751,170.370376596406));
#36230=CARTESIAN_POINT('Ctrl Pts',(30.0664294383068,-30.8004104756918,170.259246807187));
#36231=CARTESIAN_POINT('Ctrl Pts',(31.9590162413113,-29.7249108862727,170.148117017967));
#36232=CARTESIAN_POINT('Ctrl Pts',(33.8891109358174,-30.7315481814228,170.036987228747));
#36233=CARTESIAN_POINT('Ctrl Pts',(34.0903117884183,-32.8990588251476,169.925857439528));
#36234=CARTESIAN_POINT('Ctrl Pts',(32.3784819607464,-34.2437605819842,169.814727650308));
#36235=CARTESIAN_POINT('Ctrl Pts',(30.320269547065,-33.5349969867593,169.703597861088));
#36236=CARTESIAN_POINT('Ctrl Pts',(29.7993282279921,-31.4214207956012,169.592468071869));
#36237=CARTESIAN_POINT('Ctrl Pts',(31.292417849368,-29.8373540178792,169.481338282649));
#36238=CARTESIAN_POINT('Ctrl Pts',(33.4330789815959,-30.2325173900741,169.370208493429));
#36239=CARTESIAN_POINT('Ctrl Pts',(34.2622017709567,-32.2452616793244,169.259078704209));
#36240=CARTESIAN_POINT('Ctrl Pts',(33.0209820321044,-34.0335451394052,169.14794891499));
#36241=CARTESIAN_POINT('Ctrl Pts',(30.8453706095393,-33.9607501407891,169.03681912577));
#36242=CARTESIAN_POINT('Ctrl Pts',(29.7264634837301,-32.0934978767565,168.92568933655));
#36243=CARTESIAN_POINT('Ctrl Pts',(30.6882723220514,-30.1406773698913,168.814559547331));
#36244=CARTESIAN_POINT('Ctrl Pts',(32.8505601063057,-29.8894887705209,168.703429758111));
#36245=CARTESIAN_POINT('Ctrl Pts',(34.2344245048656,-31.5698171609635,168.592299968891));
#36246=CARTESIAN_POINT('Ctrl Pts',(33.573367828597,-33.6438442202791,168.481170179671));
#36247=CARTESIAN_POINT('Ctrl Pts',(31.4723819766352,-34.2134428765023,168.370040390451));
#36248=CARTESIAN_POINT('Ctrl Pts',(29.8542664207788,-32.7573226148014,168.258910601232));
#36249=CARTESIAN_POINT('Ctrl Pts',(30.1999029612069,-30.6081089111724,168.147780812012));
#36250=CARTESIAN_POINT('Ctrl Pts',(32.1929688023261,-29.7327388328916,168.036651022792));
#36251=CARTESIAN_POINT('Ctrl Pts',(34.0094316637276,-30.932341596928,167.925521233573));
#36252=CARTESIAN_POINT('Ctrl Pts',(33.9868845077251,-33.1090537336298,167.814391444353));
#36253=CARTESIAN_POINT('Ctrl Pts',(32.1459620955973,-34.2707719603118,167.703261655133));
#36254=CARTESIAN_POINT('Ctrl Pts',(30.1714569631769,-33.3543042333534,167.592131865913));
#36255=CARTESIAN_POINT('Ctrl Pts',(29.8704141674635,-31.1983921238923,167.481002076694));
#36256=CARTESIAN_POINT('Ctrl Pts',(31.5183460882199,-29.776102513524,167.369872287474));
#36257=CARTESIAN_POINT('Ctrl Pts',(33.6070807009338,-30.3891004498334,167.258742498254));
#36258=CARTESIAN_POINT('Ctrl Pts',(34.2250360367554,-32.4763747918462,167.147612709035));
#36259=CARTESIAN_POINT('Ctrl Pts',(32.8066552879638,-34.1276789269702,167.036482919815));
#36260=CARTESIAN_POINT('Ctrl Pts',(30.6500470950584,-33.8317486063998,166.925353130595));
#36261=CARTESIAN_POINT('Ctrl Pts',(29.7288711743741,-31.85943358507,166.814223341375));
#36262=CARTESIAN_POINT('Ctrl Pts',(30.8862687812559,-30.0157394792471,166.703093552156));
#36263=CARTESIAN_POINT('Ctrl Pts',(33.0628168066279,-29.9880678339112,166.591963762936));
#36264=CARTESIAN_POINT('Ctrl Pts',(34.2669395338498,-31.8015954273855,166.480833973716));
#36265=CARTESIAN_POINT('Ctrl Pts',(33.395868395384,-33.7969028631354,166.369704184497));
#36266=CARTESIAN_POINT('Ctrl Pts',(31.248363254292,-34.1472925131801,166.258574395277));
#36267=CARTESIAN_POINT('Ctrl Pts',(29.786605960109,-32.5333489778486,166.147444606057));
#36268=CARTESIAN_POINT('Ctrl Pts',(30.3549344083866,-30.4295428224182,166.036314816837));
#36269=CARTESIAN_POINT('Ctrl Pts',(31.7306127536046,-29.9891675732324,165.962228290691));
#36270=CARTESIAN_POINT('Ctrl Pts',(32.3594718785484,-30.1086918117405,165.925185027618));
#36271=CARTESIAN_POINT('Ctrl Pts',(33.5652001142722,-30.6687801966684,179.224444917147));
#36272=CARTESIAN_POINT('Ctrl Pts',(34.0078301022497,-31.1892085331676,179.187401654074));
#36273=CARTESIAN_POINT('Ctrl Pts',(34.3249209220215,-32.6979173761351,179.113315127928));
#36274=CARTESIAN_POINT('Ctrl Pts',(32.6727317243372,-34.3350173650632,179.002185338708));
#36275=CARTESIAN_POINT('Ctrl Pts',(30.4041599371754,-33.8301198258457,178.891055549488));
#36276=CARTESIAN_POINT('Ctrl Pts',(29.5964289625556,-31.6527499346609,178.779925760269));
#36277=CARTESIAN_POINT('Ctrl Pts',(30.988248508056,-29.7919884506806,178.668795971049));
#36278=CARTESIAN_POINT('Ctrl Pts',(33.3060963778469,-29.9525600136615,178.557666181829));
#36279=CARTESIAN_POINT('Ctrl Pts',(34.4285775821774,-31.9866392352977,178.446536392609));
#36280=CARTESIAN_POINT('Ctrl Pts',(33.3284712654795,-34.033087144352,178.33540660339));
#36281=CARTESIAN_POINT('Ctrl Pts',(31.0125524608971,-34.2188064667841,178.22427681417));
#36282=CARTESIAN_POINT('Ctrl Pts',(29.600339843317,-32.3739321987841,178.11314702495));
#36283=CARTESIAN_POINT('Ctrl Pts',(30.3842677675772,-30.186822526131,178.002017235731));
#36284=CARTESIAN_POINT('Ctrl Pts',(32.6468974928654,-29.6591214220926,177.890887446511));
#36285=CARTESIAN_POINT('Ctrl Pts',(34.3174930665853,-31.2737629757136,177.779757657291));
#36286=CARTESIAN_POINT('Ctrl Pts',(33.8671444034839,-33.5530507580587,177.668627868071));
#36287=CARTESIAN_POINT('Ctrl Pts',(31.7080052904067,-34.4110023564038,177.557498078852));
#36288=CARTESIAN_POINT('Ctrl Pts',(29.8160966378782,-33.0624312219618,177.446368289632));
#36289=CARTESIAN_POINT('Ctrl Pts',(29.9228726250884,-30.7415343202187,177.335238500412));
#36290=CARTESIAN_POINT('Ctrl Pts',(31.9306130769242,-29.5723716763149,177.224108711192));
#36291=CARTESIAN_POINT('Ctrl Pts',(34.0018556801289,-30.624948091138,177.112978921973));
#36292=CARTESIAN_POINT('Ctrl Pts',(34.2410216781083,-32.9359571289216,177.001849132753));
#36293=CARTESIAN_POINT('Ctrl Pts',(32.4292289371827,-34.3903883387013,176.890719343533));
#36294=CARTESIAN_POINT('Ctrl Pts',(30.2246105287083,-33.6571620702863,176.779589554314));
#36295=CARTESIAN_POINT('Ctrl Pts',(29.6448093105881,-31.4073190430277,176.668459765094));
#36296=CARTESIAN_POINT('Ctrl Pts',(31.2204530706714,-29.6998912018496,176.557329975874));
#36297=CARTESIAN_POINT('Ctrl Pts',(33.5095297265273,-30.0974979883034,176.446200186654));
#36298=CARTESIAN_POINT('Ctrl Pts',(34.4171011468898,-32.2362539844767,176.335070397435));
#36299=CARTESIAN_POINT('Ctrl Pts',(33.1125678099616,-34.1587928959332,176.223940608215));
#36300=CARTESIAN_POINT('Ctrl Pts',(30.7898244786656,-34.1056279602598,176.112810818995));
#36301=CARTESIAN_POINT('Ctrl Pts',(29.5746206606811,-32.1254151498947,176.001681029775));
#36302=CARTESIAN_POINT('Ctrl Pts',(30.5790977119008,-30.0304237544394,175.890551240556));
#36303=CARTESIAN_POINT('Ctrl Pts',(32.8839691281437,-29.737967179745,175.779421451336));
#36304=CARTESIAN_POINT('Ctrl Pts',(34.3798415845562,-31.515698511429,175.668291662116));
#36305=CARTESIAN_POINT('Ctrl Pts',(33.6977088310898,-33.7366573134195,175.557161872896));
#36306=CARTESIAN_POINT('Ctrl Pts',(31.4618513662959,-34.3682461754341,175.446032083677));
#36307=CARTESIAN_POINT('Ctrl Pts',(29.7185016950889,-32.8324418202512,175.334902294457));
#36308=CARTESIAN_POINT('Ctrl Pts',(30.0631545307178,-30.5347957386302,175.223772505237));
#36309=CARTESIAN_POINT('Ctrl Pts',(32.1803873356192,-29.5780887075362,175.112642716017));
#36310=CARTESIAN_POINT('Ctrl Pts',(34.1325316071812,-30.8378886267708,175.001512926798));
#36311=CARTESIAN_POINT('Ctrl Pts',(34.1330060781932,-33.1612402722117,174.890383137578));
#36312=CARTESIAN_POINT('Ctrl Pts',(32.1813765179305,-34.4218374136508,174.779253348358));
#36313=CARTESIAN_POINT('Ctrl Pts',(30.0637531354043,-33.4659952178498,174.668123559139));
#36314=CARTESIAN_POINT('Ctrl Pts',(29.7181618856332,-31.1684900967289,174.556993769919));
#36315=CARTESIAN_POINT('Ctrl Pts',(31.4608841326267,-29.6319738217322,174.445863980699));
#36316=CARTESIAN_POINT('Ctrl Pts',(33.6969993749721,-30.2626494249117,174.33473419148));
#36317=CARTESIAN_POINT('Ctrl Pts',(34.380039192535,-32.4833294336296,174.22360440226));
#36318=CARTESIAN_POINT('Ctrl Pts',(32.8848929515401,-34.2616715861791,174.11247461304));
#36319=CARTESIAN_POINT('Ctrl Pts',(30.5799022775602,-33.9701564298645,174.00134482382));
#36320=CARTESIAN_POINT('Ctrl Pts',(29.5745696388387,-31.8755754743948,173.890215034601));
#36321=CARTESIAN_POINT('Ctrl Pts',(30.788964563955,-29.8948664954311,173.779085245381));
#36322=CARTESIAN_POINT('Ctrl Pts',(33.1116859870073,-29.8407528706267,173.667955456161));
#36323=CARTESIAN_POINT('Ctrl Pts',(34.417004450483,-31.7627588025647,173.556825666941));
#36324=CARTESIAN_POINT('Ctrl Pts',(33.5103066521985,-33.9018853056218,173.445695877722));
#36325=CARTESIAN_POINT('Ctrl Pts',(31.2213925844155,-34.3004270020612,173.334566088502));
#36326=CARTESIAN_POINT('Ctrl Pts',(29.6450515797297,-32.5936428533062,173.223436299282));
#36327=CARTESIAN_POINT('Ctrl Pts',(30.223933830923,-30.343563202994,173.112306510062));
#36328=CARTESIAN_POINT('Ctrl Pts',(32.4282525794201,-29.6094365459927,173.001176720843));
#36329=CARTESIAN_POINT('Ctrl Pts',(34.2406392114377,-31.0631276375177,172.890046931623));
#36330=CARTESIAN_POINT('Ctrl Pts',(34.002417135868,-33.3742341552288,172.778917142403));
#36331=CARTESIAN_POINT('Ctrl Pts',(31.9316046128615,-34.4276564770234,172.667787353183));
#36332=CARTESIAN_POINT('Ctrl Pts',(29.9233868064471,-33.2593139178844,172.556657563964));
#36333=CARTESIAN_POINT('Ctrl Pts',(29.8156628748399,-30.9384609177883,172.445527774744));
#36334=CARTESIAN_POINT('Ctrl Pts',(31.7070205920295,-29.5891169738205,172.334397985525));
#36335=CARTESIAN_POINT('Ctrl Pts',(33.8665098861644,-30.4461870304743,172.223268196305));
#36336=CARTESIAN_POINT('Ctrl Pts',(34.3177895739383,-32.7252898664381,172.112138407085));
#36337=CARTESIAN_POINT('Ctrl Pts',(32.6478533790253,-34.3406152820788,172.001008617865));
#36338=CARTESIAN_POINT('Ctrl Pts',(30.3850087973056,-33.8138349744767,171.889878828646));
#36339=CARTESIAN_POINT('Ctrl Pts',(29.6001866504415,-31.6270525684548,171.778749039426));
#36340=CARTESIAN_POINT('Ctrl Pts',(31.0116476562013,-29.7815876073365,171.667619250206));
#36341=CARTESIAN_POINT('Ctrl Pts',(33.3276380087708,-29.9663896103033,171.556489460986));
#36342=CARTESIAN_POINT('Ctrl Pts',(34.4285884533479,-32.0123297883341,171.445359671767));
#36343=CARTESIAN_POINT('Ctrl Pts',(33.3069210823662,-34.0469858777925,171.334229882547));
#36344=CARTESIAN_POINT('Ctrl Pts',(30.9891737097718,-34.2082626905328,171.223100093327));
#36345=CARTESIAN_POINT('Ctrl Pts',(29.5965235960397,-32.348561436509,171.111970304107));
#36346=CARTESIAN_POINT('Ctrl Pts',(30.4035090225958,-30.1698605357837,171.000840514888));
#36347=CARTESIAN_POINT('Ctrl Pts',(32.6715856784485,-29.666083425673,170.889710725668));
#36348=CARTESIAN_POINT('Ctrl Pts',(34.3250344044286,-31.2982814541151,170.778580936448));
#36349=CARTESIAN_POINT('Ctrl Pts',(33.8506368574238,-33.5726846859303,170.667451147228));
#36350=CARTESIAN_POINT('Ctrl Pts',(31.6825565278258,-34.4077839482373,170.556321358009));
#36351=CARTESIAN_POINT('Ctrl Pts',(29.8049970214305,-33.0393054524471,170.445191568789));
#36352=CARTESIAN_POINT('Ctrl Pts',(29.9362804372059,-30.7196658773756,170.334061779569));
#36353=CARTESIAN_POINT('Ctrl Pts',(31.9562576167437,-29.5717742066846,170.22293199035));
#36354=CARTESIAN_POINT('Ctrl Pts',(34.0162673510713,-30.6461684490236,170.11180220113));
#36355=CARTESIAN_POINT('Ctrl Pts',(34.2310110712073,-32.9595746451244,170.00067241191));
#36356=CARTESIAN_POINT('Ctrl Pts',(32.4039576532821,-34.394788532161,169.88954262269));
#36357=CARTESIAN_POINT('Ctrl Pts',(30.2072065718112,-33.6383179249642,169.778412833471));
#36358=CARTESIAN_POINT('Ctrl Pts',(29.6512005937841,-31.382476519658,169.667283044251));
#36359=CARTESIAN_POINT('Ctrl Pts',(31.2447903606557,-29.6917859067979,169.556153255031));
#36360=CARTESIAN_POINT('Ctrl Pts',(33.5295397995502,-30.113547800496,169.445023465812));
#36361=CARTESIAN_POINT('Ctrl Pts',(34.4144710010597,-32.2617702894598,169.333893676592));
#36362=CARTESIAN_POINT('Ctrl Pts',(33.0897045262574,-34.1704234482866,169.222763887372));
#36363=CARTESIAN_POINT('Ctrl Pts',(30.7676522863566,-34.092728604512,169.111634098152));
#36364=CARTESIAN_POINT('Ctrl Pts',(29.5734313097712,-32.0997912365677,169.000504308933));
#36365=CARTESIAN_POINT('Ctrl Pts',(30.599979683353,-30.0155260111423,168.889374519713));
#36366=CARTESIAN_POINT('Ctrl Pts',(32.9078114683222,-29.7474298595245,168.778244730493));
#36367=CARTESIAN_POINT('Ctrl Pts',(34.3848240419215,-31.5408614725078,168.667114941273));
#36368=CARTESIAN_POINT('Ctrl Pts',(33.679271515441,-33.7544916864091,168.555985152054));
#36369=CARTESIAN_POINT('Ctrl Pts',(31.4368679074494,-34.3624301361752,168.444855362834));
#36370=CARTESIAN_POINT('Ctrl Pts',(29.7098366867433,-32.8082981435875,168.333725573614));
#36371=CARTESIAN_POINT('Ctrl Pts',(30.0787380882382,-30.5144204580892,168.222595784395));
#36372=CARTESIAN_POINT('Ctrl Pts',(32.2059575689964,-29.5801290538745,168.111465995175));
#36373=CARTESIAN_POINT('Ctrl Pts',(34.1446868899892,-30.8604773073957,168.000336205955));
#36374=CARTESIAN_POINT('Ctrl Pts',(34.1206220806415,-33.1837043507103,167.889206416735));
#36375=CARTESIAN_POINT('Ctrl Pts',(32.1557868319255,-34.4236180514851,167.778076627515));
#36376=CARTESIAN_POINT('Ctrl Pts',(30.0483773846876,-33.4454627080684,167.666946838296));
#36377=CARTESIAN_POINT('Ctrl Pts',(29.7270713413188,-31.1444357457715,167.555817049076));
#36378=CARTESIAN_POINT('Ctrl Pts',(31.4859258720994,-29.6264115520718,167.444687259857));
#36379=CARTESIAN_POINT('Ctrl Pts',(33.7152536076064,-30.2806704956948,167.333557470637));
#36380=CARTESIAN_POINT('Ctrl Pts',(34.3748036342428,-32.5084396694031,167.222427681417));
#36381=CARTESIAN_POINT('Ctrl Pts',(32.8609514083336,-34.2708933989397,167.111297892197));
#36382=CARTESIAN_POINT('Ctrl Pts',(30.5591815090839,-33.9550439523851,167.000168102978));
#36383=CARTESIAN_POINT('Ctrl Pts',(29.5760010625288,-31.8499720330306,166.889038313758));
#36384=CARTESIAN_POINT('Ctrl Pts',(30.8113033217656,-29.8821785273914,166.777908524538));
#36385=CARTESIAN_POINT('Ctrl Pts',(33.1343552073857,-29.8526442983615,166.666778735318));
#36386=CARTESIAN_POINT('Ctrl Pts',(34.4195276636713,-31.7882407779865,166.555648946099));
#36387=CARTESIAN_POINT('Ctrl Pts',(33.4898245617256,-33.917852735535,166.444519156879));
#36388=CARTESIAN_POINT('Ctrl Pts',(31.1977704424326,-34.291827179356,166.333389367659));
#36389=CARTESIAN_POINT('Ctrl Pts',(29.6376219876378,-32.5692487986674,166.222259578439));
#36390=CARTESIAN_POINT('Ctrl Pts',(30.2442047315206,-30.3238350520459,166.11112978922));
#36391=CARTESIAN_POINT('Ctrl Pts',(31.7124802469756,-29.853818061345,166.037043263073));
#36392=CARTESIAN_POINT('Ctrl Pts',(32.3836679988472,-29.9813874990082,166.));
#36393=CARTESIAN_POINT('Ctrl Pts',(33.2690708798528,-30.920641346952,179.));
#36394=CARTESIAN_POINT('Ctrl Pts',(33.3143937870934,-30.9629228091432,179.));
#36395=CARTESIAN_POINT('Ctrl Pts',(33.3569863363192,-31.0077738608052,179.));
#36396=CARTESIAN_POINT('Ctrl Pts',(33.3968502559163,-31.0548493575027,179.));
#36397=CARTESIAN_POINT('Ctrl Pts',(33.4393504278583,-31.1050380174266,179.));
#36398=CARTESIAN_POINT('Ctrl Pts',(33.4787498660929,-31.1577552940212,179.));
#36399=CARTESIAN_POINT('Ctrl Pts',(33.515021814116,-31.2126376739653,179.));
#36400=CARTESIAN_POINT('Ctrl Pts',(33.5467597686362,-31.2606597564164,179.));
#36401=CARTESIAN_POINT('Ctrl Pts',(33.5761029944634,-31.3103407222917,179.));
#36402=CARTESIAN_POINT('Ctrl Pts',(33.6030106666263,-31.361464609715,179.));
#36403=CARTESIAN_POINT('Ctrl Pts',(33.6165048228579,-31.3871031606784,179.));
#36404=CARTESIAN_POINT('Ctrl Pts',(33.6293860750336,-31.4131049631121,179.));
#36405=CARTESIAN_POINT('Ctrl Pts',(33.641646934939,-31.4394446180088,179.));
#36406=CARTESIAN_POINT('Ctrl Pts',(33.6472617614843,-31.4515067893939,179.));
#36407=CARTESIAN_POINT('Ctrl Pts',(33.6527470722687,-31.4636415260275,179.));
#36408=CARTESIAN_POINT('Ctrl Pts',(33.658093608444,-31.4758263637454,179.));
#36409=CARTESIAN_POINT('Ctrl Pts',(33.6850051809481,-31.5371582490902,179.));
#36410=CARTESIAN_POINT('Ctrl Pts',(33.7084559555629,-31.5998656904031,179.));
#36411=CARTESIAN_POINT('Ctrl Pts',(33.7284227072741,-31.663590733636,179.));
#36412=CARTESIAN_POINT('Ctrl Pts',(33.7487447393774,-31.7284496747945,179.));
#36413=CARTESIAN_POINT('Ctrl Pts',(33.765458215908,-31.7943635951405,179.));
#36414=CARTESIAN_POINT('Ctrl Pts',(33.7784993315041,-31.8609916099304,179.));
#36415=CARTESIAN_POINT('Ctrl Pts',(33.7894070090125,-31.9167197332644,179.));
#36416=CARTESIAN_POINT('Ctrl Pts',(33.797745034606,-31.9729483616004,179.));
#36417=CARTESIAN_POINT('Ctrl Pts',(33.8034512516889,-32.029490320182,179.));
#36418=CARTESIAN_POINT('Ctrl Pts',(33.8060783951693,-32.0555222491633,179.));
#36419=CARTESIAN_POINT('Ctrl Pts',(33.8081473437298,-32.0816207072311,179.));
#36420=CARTESIAN_POINT('Ctrl Pts',(33.8096502328989,-32.1077678283934,179.));
#36421=CARTESIAN_POINT('Ctrl Pts',(33.8103081534512,-32.1192142668601,179.));
#36422=CARTESIAN_POINT('Ctrl Pts',(33.810857477492,-32.130669870472,179.));
#36423=CARTESIAN_POINT('Ctrl Pts',(33.8112972071105,-32.1421189247609,179.));
#36424=CARTESIAN_POINT('Ctrl Pts',(33.8139908004847,-32.2122508773816,179.));
#36425=CARTESIAN_POINT('Ctrl Pts',(33.8125842846173,-32.2822684969545,179.));
#36426=CARTESIAN_POINT('Ctrl Pts',(33.8070233187848,-32.3518106703801,179.));
#36427=CARTESIAN_POINT('Ctrl Pts',(33.802053136137,-32.4139648561934,179.));
#36428=CARTESIAN_POINT('Ctrl Pts',(33.7937639803061,-32.4757402141871,179.));
#36429=CARTESIAN_POINT('Ctrl Pts',(33.7820839574515,-32.5368910554573,179.));
#36430=CARTESIAN_POINT('Ctrl Pts',(33.7693542202861,-32.6035376833369,179.));
#36431=CARTESIAN_POINT('Ctrl Pts',(33.7525978242256,-32.6694433303306,179.));
#36432=CARTESIAN_POINT('Ctrl Pts',(33.7320598219069,-32.7343945881359,179.));
#36433=CARTESIAN_POINT('Ctrl Pts',(33.7241290562722,-32.7594755670618,179.));
#36434=CARTESIAN_POINT('Ctrl Pts',(33.7156338517038,-32.7844141873628,179.));
#36435=CARTESIAN_POINT('Ctrl Pts',(33.7065863065718,-32.8091978397264,179.));
#36436=CARTESIAN_POINT('Ctrl Pts',(33.7026186329799,-32.820066361691,179.));
#36437=CARTESIAN_POINT('Ctrl Pts',(33.698544834818,-32.8309045228361,179.));
#36438=CARTESIAN_POINT('Ctrl Pts',(33.6943710227137,-32.841698708458,179.));
#36439=CARTESIAN_POINT('Ctrl Pts',(33.6691495102391,-32.9069258151202,179.));
#36440=CARTESIAN_POINT('Ctrl Pts',(33.6402375808801,-32.9706664152282,179.));
#36441=CARTESIAN_POINT('Ctrl Pts',(33.6079477009133,-33.0327018841654,179.));
#36442=CARTESIAN_POINT('Ctrl Pts',(33.5749109983802,-33.096172152122,179.));
#36443=CARTESIAN_POINT('Ctrl Pts',(33.5383379809688,-33.1578583209809,179.));
#36444=CARTESIAN_POINT('Ctrl Pts',(33.498507171859,-33.2175225123557,179.));
#36445=CARTESIAN_POINT('Ctrl Pts',(33.4680143720159,-33.2631989192893,179.));
#36446=CARTESIAN_POINT('Ctrl Pts',(33.4356110327496,-33.3076903192047,179.));
#36447=CARTESIAN_POINT('Ctrl Pts',(33.4014025677393,-33.3508838705313,179.));
#36448=CARTESIAN_POINT('Ctrl Pts',(33.3801002535635,-33.3777813826077,179.));
#36449=CARTESIAN_POINT('Ctrl Pts',(33.3580976222504,-33.4041754908389,179.));
#36450=CARTESIAN_POINT('Ctrl Pts',(33.3354172175954,-33.4300372539183,179.));
#36451=CARTESIAN_POINT('Ctrl Pts',(33.3227588439286,-33.4444712054162,179.));
#36452=CARTESIAN_POINT('Ctrl Pts',(33.3098849003051,-33.4587438432578,179.));
#36453=CARTESIAN_POINT('Ctrl Pts',(33.2968229201931,-33.4728248058561,179.));
#36454=CARTESIAN_POINT('Ctrl Pts',(33.2459584485793,-33.527657282727,179.));
#36455=CARTESIAN_POINT('Ctrl Pts',(33.1921974637621,-33.5796446805326,179.));
#36456=CARTESIAN_POINT('Ctrl Pts',(33.1358246431769,-33.6285233175597,179.));
#36457=CARTESIAN_POINT('Ctrl Pts',(33.0936773563628,-33.6650675584275,179.));
#36458=CARTESIAN_POINT('Ctrl Pts',(33.0500689377864,-33.6998738513906,179.));
#36459=CARTESIAN_POINT('Ctrl Pts',(33.0051019841789,-33.7328222569625,179.));
#36460=CARTESIAN_POINT('Ctrl Pts',(32.9910181375986,-33.7431418417224,179.));
#36461=CARTESIAN_POINT('Ctrl Pts',(32.976800930029,-33.7532790962547,179.));
#36462=CARTESIAN_POINT('Ctrl Pts',(32.9624532710857,-33.7632301075464,179.));
#36463=CARTESIAN_POINT('Ctrl Pts',(32.9486742705369,-33.7727867181818,179.));
#36464=CARTESIAN_POINT('Ctrl Pts',(32.9347820152157,-33.7821665966601,179.));
#36465=CARTESIAN_POINT('Ctrl Pts',(32.9207844060457,-33.7913635692792,179.));
#36466=CARTESIAN_POINT('Ctrl Pts',(32.8578362168016,-33.8327229732939,179.));
#36467=CARTESIAN_POINT('Ctrl Pts',(32.7927300171995,-33.8704071115942,179.));
#36468=CARTESIAN_POINT('Ctrl Pts',(32.7257268190738,-33.9041370513948,179.));
#36469=CARTESIAN_POINT('Ctrl Pts',(32.6745421251937,-33.9299038310647,179.));
#36470=CARTESIAN_POINT('Ctrl Pts',(32.6222494359116,-33.9533626701466,179.));
#36471=CARTESIAN_POINT('Ctrl Pts',(32.5689512759831,-33.9743740101343,179.));
#36472=CARTESIAN_POINT('Ctrl Pts',(32.5564668663362,-33.9792956467535,179.));
#36473=CARTESIAN_POINT('Ctrl Pts',(32.5439272450406,-33.9840829288593,179.));
#36474=CARTESIAN_POINT('Ctrl Pts',(32.5313343692882,-33.9887364495513,179.));
#36475=CARTESIAN_POINT('Ctrl Pts',(30.3326674689016,-32.0013033567452,177.87148036339));
#36476=CARTESIAN_POINT('Ctrl Pts',(30.3319312465786,-32.0869545016077,177.877220944861));
#36477=CARTESIAN_POINT('Ctrl Pts',(30.3379613926568,-32.1725016619386,177.882961526332));
#36478=CARTESIAN_POINT('Ctrl Pts',(30.3511187262443,-32.2569381575126,177.888702107803));
#36479=CARTESIAN_POINT('Ctrl Pts',(30.4360213745041,-32.8017964326578,177.925745370876));
#36480=CARTESIAN_POINT('Ctrl Pts',(30.817697364428,-33.3004070552782,177.962788633949));
#36481=CARTESIAN_POINT('Ctrl Pts',(31.3214948214846,-33.524615364425,177.999831897022));
#36482=CARTESIAN_POINT('Ctrl Pts',(31.8252922785413,-33.7488236735718,178.036875160096));
#36483=CARTESIAN_POINT('Ctrl Pts',(32.4512112027306,-33.698629669245,178.073918423169));
#36484=CARTESIAN_POINT('Ctrl Pts',(32.9128324747469,-33.3969878954966,178.110961686242));
#36485=CARTESIAN_POINT('Ctrl Pts',(33.3744537467632,-33.0953461217483,178.148004949315));
#36486=CARTESIAN_POINT('Ctrl Pts',(33.6717773666064,-32.5422565785785,178.185048212389));
#36487=CARTESIAN_POINT('Ctrl Pts',(33.6687537576681,-31.9908384660968,178.222091475462));
#36488=CARTESIAN_POINT('Ctrl Pts',(33.6657301487298,-31.4394203536152,178.259134738535));
#36489=CARTESIAN_POINT('Ctrl Pts',(33.36235931101,-30.8896736718216,178.296178001608));
#36490=CARTESIAN_POINT('Ctrl Pts',(32.8974537476822,-30.5931016470682,178.333221264682));
#36491=CARTESIAN_POINT('Ctrl Pts',(32.4325481843545,-30.2965296223148,178.370264527755));
#36492=CARTESIAN_POINT('Ctrl Pts',(31.8061078954188,-30.2531322546016,178.407307790828));
#36493=CARTESIAN_POINT('Ctrl Pts',(31.3048055541871,-30.4828857857193,178.444351053901));
#36494=CARTESIAN_POINT('Ctrl Pts',(30.8035032129554,-30.7126393168371,178.481394316974));
#36495=CARTESIAN_POINT('Ctrl Pts',(30.4273388194276,-31.2155437467857,178.518437580048));
#36496=CARTESIAN_POINT('Ctrl Pts',(30.3484085717018,-31.7612327495861,178.555480843121));
#36497=CARTESIAN_POINT('Ctrl Pts',(30.3370448670893,-31.8397964031507,178.560814016544));
#36498=CARTESIAN_POINT('Ctrl Pts',(30.3318421685893,-31.9192468862352,178.566147189967));
#36499=CARTESIAN_POINT('Ctrl Pts',(30.3325025779359,-31.9987820654682,178.57148036339));
#36500=CARTESIAN_POINT('Ctrl Pts',(31.4698297828105,-33.9851743256715,179.));
#36501=CARTESIAN_POINT('Ctrl Pts',(30.8097602092464,-33.8088929660693,178.962956736927));
#36502=CARTESIAN_POINT('Ctrl Pts',(29.6908221036295,-32.748363474976,178.88887021078));
#36503=CARTESIAN_POINT('Ctrl Pts',(30.1185590192689,-30.4621264977465,178.777740421561));
#36504=CARTESIAN_POINT('Ctrl Pts',(32.2716026642884,-29.5870613462295,178.666610632341));
#36505=CARTESIAN_POINT('Ctrl Pts',(34.1744104601116,-30.9184848843002,178.555480843121));
#36506=CARTESIAN_POINT('Ctrl Pts',(34.0880400722661,-33.2405822108959,178.444351053901));
#36507=CARTESIAN_POINT('Ctrl Pts',(32.0903159787745,-34.4268786410256,178.333221264682));
#36508=CARTESIAN_POINT('Ctrl Pts',(30.0101331764293,-33.3923349810139,178.222091475462));
#36509=CARTESIAN_POINT('Ctrl Pts',(29.750957902677,-31.0834368587032,178.110961686242));
#36510=CARTESIAN_POINT('Ctrl Pts',(31.5501292172184,-29.6134187564108,177.999831897022));
#36511=CARTESIAN_POINT('Ctrl Pts',(33.7609939876075,-30.3275486926383,177.888702107803));
#36512=CARTESIAN_POINT('Ctrl Pts',(34.3602276546561,-32.5723003233786,177.777572318583));
#36513=CARTESIAN_POINT('Ctrl Pts',(32.7994009204969,-34.2932828161059,177.666442529363));
#36514=CARTESIAN_POINT('Ctrl Pts',(30.506973906968,-33.9154807357568,177.555312740144));
#36515=CARTESIAN_POINT('Ctrl Pts',(29.580946820041,-31.7846499895867,177.444182950924));
#36516=CARTESIAN_POINT('Ctrl Pts',(30.8688116391535,-29.8509059591332,177.333053161704));
#36517=CARTESIAN_POINT('Ctrl Pts',(33.1919274501366,-29.8839891344978,177.221923372484));
#36518=CARTESIAN_POINT('Ctrl Pts',(34.4242043461506,-31.8536226808824,177.110793583265));
#36519=CARTESIAN_POINT('Ctrl Pts',(33.4378756346499,-33.9572190768126,176.999663794045));
#36520=CARTESIAN_POINT('Ctrl Pts',(31.1356187743909,-34.2695898408057,176.888534004825));
#36521=CARTESIAN_POINT('Ctrl Pts',(29.6244342188476,-32.5048565745377,176.777404215605));
#36522=CARTESIAN_POINT('Ctrl Pts',(30.2873417136773,-30.2780840563291,176.666274426386));
#36523=CARTESIAN_POINT('Ctrl Pts',(32.5176554945262,-29.6271903313891,176.555144637166));
#36524=CARTESIAN_POINT('Ctrl Pts',(34.2742165827931,-31.1478662855577,176.444014847946));
#36525=CARTESIAN_POINT('Ctrl Pts',(33.9494393162254,-33.4484057729775,176.332885058727));
#36526=CARTESIAN_POINT('Ctrl Pts',(31.8405563287846,-34.4233800048647,176.221755269507));
#36527=CARTESIAN_POINT('Ctrl Pts',(29.8775944598767,-33.1805031364718,176.110625480287));
#36528=CARTESIAN_POINT('Ctrl Pts',(29.857035124892,-30.8572425997456,175.999495691067));
#36529=CARTESIAN_POINT('Ctrl Pts',(31.797694004055,-29.5798212429744,175.888365901848));
#36530=CARTESIAN_POINT('Ctrl Pts',(33.9235011368215,-30.5173212389216,175.777236112628));
#36531=CARTESIAN_POINT('Ctrl Pts',(34.2889408886545,-32.8117527580092,175.666106323408));
#36532=CARTESIAN_POINT('Ctrl Pts',(32.5595667617289,-34.3632769560673,175.554976534188));
#36533=CARTESIAN_POINT('Ctrl Pts',(30.3180832027141,-33.7519557125998,175.443846744969));
#36534=CARTESIAN_POINT('Ctrl Pts',(29.615871656949,-31.5372636001316,175.332716955749));
#36535=CARTESIAN_POINT('Ctrl Pts',(31.095588515948,-29.7460628226547,175.221587166529));
#36536=CARTESIAN_POINT('Ctrl Pts',(33.4030129572177,-30.0176409069538,175.110457377309));
#36537=CARTESIAN_POINT('Ctrl Pts',(34.4264151550835,-32.1034525354194,174.99932758809));
#36538=CARTESIAN_POINT('Ctrl Pts',(33.2291885163936,-34.0945855253653,174.88819779887));
#36539=CARTESIAN_POINT('Ctrl Pts',(30.9070218774947,-34.168776557331,174.777068009651));
#36540=CARTESIAN_POINT('Ctrl Pts',(29.5851369634584,-32.2581268034298,174.665938220431));
#36541=CARTESIAN_POINT('Ctrl Pts',(30.4733085123659,-30.1112421982983,174.554808431211));
#36542=CARTESIAN_POINT('Ctrl Pts',(32.7586915544763,-29.6929282505587,174.443678641991));
#36543=CARTESIAN_POINT('Ctrl Pts',(34.3497283135974,-31.3860213487566,174.332548852772));
#36544=CARTESIAN_POINT('Ctrl Pts',(33.7903192018566,-33.6410210502512,174.221419063552));
#36545=CARTESIAN_POINT('Ctrl Pts',(31.5924293717799,-34.3941760826881,174.110289274332));
#36546=CARTESIAN_POINT('Ctrl Pts',(29.7675437607309,-32.9562071280074,173.999159485112));
#36547=CARTESIAN_POINT('Ctrl Pts',(29.9857778898812,-30.6431277794088,173.888029695893));
#36548=CARTESIAN_POINT('Ctrl Pts',(32.0474062508829,-29.5718431724288,173.776899906673));
#36549=CARTESIAN_POINT('Ctrl Pts',(34.0656489251761,-30.7227813617776,173.665770117453));
#36550=CARTESIAN_POINT('Ctrl Pts',(34.1934321041778,-33.0426161979683,173.554640328233));
#36551=CARTESIAN_POINT('Ctrl Pts',(32.3138100082167,-34.4082599964802,173.443510539014));
#36552=CARTESIAN_POINT('Ctrl Pts',(30.1469923958635,-33.5698903627056,173.332380749794));
#36553=CARTESIAN_POINT('Ctrl Pts',(29.6760272477853,-31.2947740937349,173.221250960574));
#36554=CARTESIAN_POINT('Ctrl Pts',(31.331936760099,-29.6650729263216,173.110121171355));
#36555=CARTESIAN_POINT('Ctrl Pts',(33.5992505047259,-30.1722716955089,172.998991382135));
#36556=CARTESIAN_POINT('Ctrl Pts',(34.4029475305773,-32.3521875880785,172.887861592915));
#36557=CARTESIAN_POINT('Ctrl Pts',(33.0074930353251,-34.2097852193539,172.776731803695));
#36558=CARTESIAN_POINT('Ctrl Pts',(30.6899918399505,-34.0450113819995,172.665602014476));
#36559=CARTESIAN_POINT('Ctrl Pts',(29.5713959062062,-32.0086653050641,172.554472225256));
#36560=CARTESIAN_POINT('Ctrl Pts',(30.6754321019873,-29.9643888349053,172.443342436036));
#36561=CARTESIAN_POINT('Ctrl Pts',(32.9916984736889,-29.7830816277574,172.332212646816));
#36562=CARTESIAN_POINT('Ctrl Pts',(34.4003731567925,-31.6306740734072,172.221082857597));
#36563=CARTESIAN_POINT('Ctrl Pts',(33.6122523577626,-33.8162696019019,172.109953068377));
#36564=CARTESIAN_POINT('Ctrl Pts',(31.3486156850571,-34.3396348873596,171.998823279157));
#36565=CARTESIAN_POINT('Ctrl Pts',(29.6811188734186,-32.7217916961897,171.887693489937));
#36566=CARTESIAN_POINT('Ctrl Pts',(30.1358369216088,-30.4433725721719,171.776563700718));
#36567=CARTESIAN_POINT('Ctrl Pts',(32.2966168031358,-29.589561989181,171.665433911498));
#36568=CARTESIAN_POINT('Ctrl Pts',(34.1859362031082,-30.9417581335798,171.554304122278));
#36569=CARTESIAN_POINT('Ctrl Pts',(34.0747104954871,-33.2624457579713,171.443174333059));
#36570=CARTESIAN_POINT('Ctrl Pts',(32.0647322416946,-34.4277567153216,171.332044543839));
#36571=CARTESIAN_POINT('Ctrl Pts',(29.9955117422951,-33.3712110547348,171.220914754619));
#36572=CARTESIAN_POINT('Ctrl Pts',(29.7607771585773,-31.0597479070194,171.1097849654));
#36573=CARTESIAN_POINT('Ctrl Pts',(31.5753550359689,-29.6087932781905,170.99865517618));
#36574=CARTESIAN_POINT('Ctrl Pts',(33.778563379359,-30.3462451096045,170.88752538696));
#36575=CARTESIAN_POINT('Ctrl Pts',(34.3540498056764,-32.5971954824835,170.77639559774));
#36576=CARTESIAN_POINT('Ctrl Pts',(32.7751353784459,-34.3015990261089,170.665265808521));
#36577=CARTESIAN_POINT('Ctrl Pts',(30.4868254588548,-33.8996041008415,170.554136019301));
#36578=CARTESIAN_POINT('Ctrl Pts',(29.5833564696252,-31.7591121028326,170.443006230081));
#36579=CARTESIAN_POINT('Ctrl Pts',(30.8915734319869,-29.8390780959909,170.331876440861));
#36580=CARTESIAN_POINT('Ctrl Pts',(33.2142103690085,-29.896696381476,170.220746651642));
#36581=CARTESIAN_POINT('Ctrl Pts',(34.4256151438767,-31.8792353292564,170.109616862422));
#36582=CARTESIAN_POINT('Ctrl Pts',(33.4171232437699,-33.9722967940629,169.998487073202));
#36583=CARTESIAN_POINT('Ctrl Pts',(31.1116955190265,-34.2603336216113,169.887357283983));
#36584=CARTESIAN_POINT('Ctrl Pts',(29.6192344220091,-32.4797376309583,169.776227494763));
#36585=CARTESIAN_POINT('Ctrl Pts',(30.3056241636414,-30.2600909629904,169.665097705543));
#36586=CARTESIAN_POINT('Ctrl Pts',(32.5426882959684,-29.6327901771656,169.553967916323));
#36587=CARTESIAN_POINT('Ctrl Pts',(34.2830899850343,-31.1719341498779,169.442838127104));
#36588=CARTESIAN_POINT('Ctrl Pts',(33.9340324788774,-33.4689150086206,169.331708337884));
#36589=CARTESIAN_POINT('Ctrl Pts',(31.8149694217593,-34.4215607811959,169.220578548664));
#36590=CARTESIAN_POINT('Ctrl Pts',(29.8652443432771,-33.1580203875493,169.109448759444));
#36591=CARTESIAN_POINT('Ctrl Pts',(29.8692244913603,-30.8346722934351,168.998318970224));
#36592=CARTESIAN_POINT('Ctrl Pts',(31.8232672776651,-29.5778194788973,168.887189181005));
#36593=CARTESIAN_POINT('Ctrl Pts',(33.9390539348382,-30.5377200098576,168.776059391785));
#36594=CARTESIAN_POINT('Ctrl Pts',(34.2802394590648,-32.8358833299508,168.664929602565));
#36595=CARTESIAN_POINT('Ctrl Pts',(32.5345745584143,-34.3690552914116,168.553799813346));
#36596=CARTESIAN_POINT('Ctrl Pts',(30.299672819343,-33.7340935411791,168.442670024126));
#36597=CARTESIAN_POINT('Ctrl Pts',(29.62089207628,-31.5121081881889,168.331540234906));
#36598=CARTESIAN_POINT('Ctrl Pts',(31.1194451055679,-29.7366361290419,168.220410445686));
#36599=CARTESIAN_POINT('Ctrl Pts',(33.42387242316,-30.0325701422052,168.109280656467));
#36600=CARTESIAN_POINT('Ctrl Pts',(34.4251871441161,-32.1290746196978,167.998150867247));
#36601=CARTESIAN_POINT('Ctrl Pts',(33.2069968831276,-34.107451416473,167.887021078027));
#36602=CARTESIAN_POINT('Ctrl Pts',(30.8841761797311,-34.1571115078919,167.775891288808));
#36603=CARTESIAN_POINT('Ctrl Pts',(29.5825453040883,-32.2326065877438,167.664761499588));
#36604=CARTESIAN_POINT('Ctrl Pts',(30.4933428149864,-30.0952225441907,167.553631710368));
#36605=CARTESIAN_POINT('Ctrl Pts',(32.7830165101667,-29.7010703688433,167.442501921148));
#36606=CARTESIAN_POINT('Ctrl Pts',(34.3560822562997,-31.4108732598121,167.331372131929));
#36607=CARTESIAN_POINT('Ctrl Pts',(33.7728865232597,-33.6598393714977,167.220242342709));
#36608=CARTESIAN_POINT('Ctrl Pts',(31.567165387668,-34.3897368274991,167.10911255349));
#36609=CARTESIAN_POINT('Ctrl Pts',(29.7575675205768,-32.9325764403901,166.997982764269));
#36610=CARTESIAN_POINT('Ctrl Pts',(30.0002241716332,-30.6219253154616,166.88685297505));
#36611=CARTESIAN_POINT('Ctrl Pts',(32.0730445458741,-29.572487230153,166.77572318583));
#36612=CARTESIAN_POINT('Ctrl Pts',(34.0790345383106,-30.7446539377421,166.66459339661));
#36613=CARTESIAN_POINT('Ctrl Pts',(34.1822755906712,-33.0657579093129,166.55346360739));
#36614=CARTESIAN_POINT('Ctrl Pts',(32.2884012423449,-34.4113733924264,166.442333818171));
#36615=CARTESIAN_POINT('Ctrl Pts',(30.1304232450055,-33.550367157342,166.331204028951));
#36616=CARTESIAN_POINT('Ctrl Pts',(29.6837913440556,-31.2699909201536,166.220074239732));
#36617=CARTESIAN_POINT('Ctrl Pts',(31.3562571438711,-29.6587105925812,166.108944450511));
#36618=CARTESIAN_POINT('Ctrl Pts',(33.6192360418519,-30.188108801921,165.997814661292));
#36619=CARTESIAN_POINT('Ctrl Pts',(34.3974969940138,-32.3799455374906,165.886684872072));
#36620=CARTESIAN_POINT('Ctrl Pts',(33.4572031808892,-33.601662702255,165.812598345926));
#36621=CARTESIAN_POINT('Ctrl Pts',(32.8326019491383,-33.8785024771853,165.775555082853));
#36622=CARTESIAN_POINT('Ctrl Pts',(31.5032651029115,-33.8599788000025,179.074814972382));
#36623=CARTESIAN_POINT('Ctrl Pts',(30.8848229855218,-33.6948146693488,179.037771709309));
#36624=CARTESIAN_POINT('Ctrl Pts',(29.8364509972035,-32.7011677413673,178.963685183163));
#36625=CARTESIAN_POINT('Ctrl Pts',(30.2372125750557,-30.5591128827894,178.852555393943));
#36626=CARTESIAN_POINT('Ctrl Pts',(32.2544739729241,-29.7392339384594,178.741425604723));
#36627=CARTESIAN_POINT('Ctrl Pts',(34.0372807093117,-30.9866909111856,178.630295815504));
#36628=CARTESIAN_POINT('Ctrl Pts',(33.9563572920262,-33.1623445770418,178.519166026284));
#36629=CARTESIAN_POINT('Ctrl Pts',(32.0846201785151,-34.2738269199405,178.408036237064));
#36630=CARTESIAN_POINT('Ctrl Pts',(30.1356246356763,-33.3045270199694,178.296906447844));
#36631=CARTESIAN_POINT('Ctrl Pts',(29.8927943167313,-31.1412401472102,178.185776658625));
#36632=CARTESIAN_POINT('Ctrl Pts',(31.5785004329878,-29.7639291118385,178.074646869405));
#36633=CARTESIAN_POINT('Ctrl Pts',(33.6499364521924,-30.4330222613185,177.963517080185));
#36634=CARTESIAN_POINT('Ctrl Pts',(34.2113792950426,-32.5362080573748,177.852387290966));
#36635=CARTESIAN_POINT('Ctrl Pts',(32.7489864973565,-34.1486563498267,177.741257501746));
#36636=CARTESIAN_POINT('Ctrl Pts',(30.6011319786987,-33.7946804541288,177.630127712526));
#36637=CARTESIAN_POINT('Ctrl Pts',(29.733505026426,-31.7982310929729,177.518997923306));
#36638=CARTESIAN_POINT('Ctrl Pts',(30.9401503219258,-29.98643912349,177.407868134087));
#36639=CARTESIAN_POINT('Ctrl Pts',(33.1167582411914,-30.0174358999541,177.296738344867));
#36640=CARTESIAN_POINT('Ctrl Pts',(34.2713212801546,-31.8628540038831,177.185608555647));
#36641=CARTESIAN_POINT('Ctrl Pts',(33.347195640657,-33.83378655605,177.074478766427));
#36642=CARTESIAN_POINT('Ctrl Pts',(31.1901311970629,-34.1264575780627,176.963348977208));
#36643=CARTESIAN_POINT('Ctrl Pts',(29.7742498813245,-32.4730176657732,176.852219187988));
#36644=CARTESIAN_POINT('Ctrl Pts',(30.3953509457505,-30.3866771249266,176.741089398768));
#36645=CARTESIAN_POINT('Ctrl Pts',(32.4850094186051,-29.7768321789249,176.629959609548));
#36646=CARTESIAN_POINT('Ctrl Pts',(34.1307925333854,-31.2016063158112,176.518829820329));
#36647=CARTESIAN_POINT('Ctrl Pts',(33.8264974280504,-33.3570616931227,176.407700031109));
#36648=CARTESIAN_POINT('Ctrl Pts',(31.8506116846162,-34.2705489261624,176.296570241889));
#36649=CARTESIAN_POINT('Ctrl Pts',(30.0114445071206,-33.1060544047845,176.18544045267));
#36650=CARTESIAN_POINT('Ctrl Pts',(29.9921817518455,-30.9293108869418,176.07431066345));
#36651=CARTESIAN_POINT('Ctrl Pts',(31.8104524833385,-29.7324504341645,175.96318087423));
#36652=CARTESIAN_POINT('Ctrl Pts',(33.8021950465527,-30.610826753521,175.85205108501));
#36653=CARTESIAN_POINT('Ctrl Pts',(34.1445882471386,-32.7605593630827,175.740921295791));
#36654=CARTESIAN_POINT('Ctrl Pts',(32.5242775410416,-34.2142362914817,175.629791506571));
#36655=CARTESIAN_POINT('Ctrl Pts',(30.4241537149329,-33.6414681783056,175.518661717351));
#36656=CARTESIAN_POINT('Ctrl Pts',(29.766227319578,-31.5664461893272,175.407531928131));
#36657=CARTESIAN_POINT('Ctrl Pts',(31.1526254570884,-29.8882079461803,175.296402138912));
#36658=CARTESIAN_POINT('Ctrl Pts',(33.3145315868777,-30.1426588892585,175.185272349692));
#36659=CARTESIAN_POINT('Ctrl Pts',(34.2733926638577,-32.0969282748614,175.074142560472));
#36660=CARTESIAN_POINT('Ctrl Pts',(33.1516694287921,-33.9624899544547,174.963012771252));
#36661=CARTESIAN_POINT('Ctrl Pts',(30.9759508218308,-34.0320021100483,174.851882982033));
#36662=CARTESIAN_POINT('Ctrl Pts',(29.7374309173791,-32.241847970671,174.740753192813));
#36663=CARTESIAN_POINT('Ctrl Pts',(30.5695897008021,-30.2303571912677,174.629623403593));
#36664=CARTESIAN_POINT('Ctrl Pts',(32.7108444778972,-29.838424319439,174.518493614374));
#36665=CARTESIAN_POINT('Ctrl Pts',(34.2015420976082,-31.4247420691477,174.407363825154));
#36666=CARTESIAN_POINT('Ctrl Pts',(33.6774122643181,-33.5375296387599,174.296234035934));
#36667=CARTESIAN_POINT('Ctrl Pts',(31.6181329175025,-34.2431867567937,174.185104246714));
#36668=CARTESIAN_POINT('Ctrl Pts',(29.9083341834127,-32.8959036813573,174.073974457495));
#36669=CARTESIAN_POINT('Ctrl Pts',(30.1128053214922,-30.7286992724136,173.962844668275));
#36670=CARTESIAN_POINT('Ctrl Pts',(32.0444165635681,-29.7249755026746,173.851714879055));
#36671=CARTESIAN_POINT('Ctrl Pts',(33.935378248344,-30.8033294812745,173.740585089836));
#36672=CARTESIAN_POINT('Ctrl Pts',(34.0551027485386,-32.9768633412606,173.629455300616));
#36673=CARTESIAN_POINT('Ctrl Pts',(32.2940194999319,-34.2563824649668,173.518325511396));
#36674=CARTESIAN_POINT('Ctrl Pts',(30.2638527934963,-33.4708848261843,173.407195722177));
#36675=CARTESIAN_POINT('Ctrl Pts',(29.8225891827203,-31.3392493455597,173.296065932956));
#36676=CARTESIAN_POINT('Ctrl Pts',(31.3740683388817,-29.8123256983364,173.184936143737));
#36677=CARTESIAN_POINT('Ctrl Pts',(33.4983933633523,-30.2875378476557,173.073806354517));
#36678=CARTESIAN_POINT('Ctrl Pts',(34.2514050310823,-32.3299767879219,172.962676565298));
#36679=CARTESIAN_POINT('Ctrl Pts',(32.9439552298366,-34.0704245503311,172.851546776078));
#36680=CARTESIAN_POINT('Ctrl Pts',(30.7726078390127,-33.9160422170966,172.740416986858));
#36681=CARTESIAN_POINT('Ctrl Pts',(29.7245564434107,-32.0081188253879,172.629287197638));
#36682=CARTESIAN_POINT('Ctrl Pts',(30.7589663146413,-30.0927651727292,172.518157408419));
#36683=CARTESIAN_POINT('Ctrl Pts',(32.9291567562624,-29.9228921508882,172.407027619199));
#36684=CARTESIAN_POINT('Ctrl Pts',(34.2489930108375,-31.6539657072577,172.295897829979));
#36685=CARTESIAN_POINT('Ctrl Pts',(33.5105752512078,-33.7017260957593,172.184768040759));
#36686=CARTESIAN_POINT('Ctrl Pts',(31.3896954031792,-34.192085215873,172.07363825154));
#36687=CARTESIAN_POINT('Ctrl Pts',(29.8273597036832,-32.676271718594,171.96250846232));
#36688=CARTESIAN_POINT('Ctrl Pts',(30.2534008420735,-30.5415416783192,171.8513786731));
#36689=CARTESIAN_POINT('Ctrl Pts',(32.2779105887189,-29.7415768777247,171.74024888388));
#36690=CARTESIAN_POINT('Ctrl Pts',(34.0480795783837,-31.0084964270577,171.629119094661));
#36691=CARTESIAN_POINT('Ctrl Pts',(33.9438683484098,-33.1828292939389,171.517989305441));
#36692=CARTESIAN_POINT('Ctrl Pts',(32.0606498863458,-34.2746496182569,171.406859516222));
#36693=CARTESIAN_POINT('Ctrl Pts',(30.1219253060186,-33.284735279494,171.295729727001));
#36694=CARTESIAN_POINT('Ctrl Pts',(29.9019943187514,-31.1190451453122,171.184599937782));
#36695=CARTESIAN_POINT('Ctrl Pts',(31.6021353790386,-29.7595953405831,171.073470148562));
#36696=CARTESIAN_POINT('Ctrl Pts',(33.6663978257676,-30.4505395839755,170.962340359342));
#36697=CARTESIAN_POINT('Ctrl Pts',(34.205591053686,-32.559533196915,170.851210570123));
#36698=CARTESIAN_POINT('Ctrl Pts',(32.72625126791,-34.1564480959227,170.740080780903));
#36699=CARTESIAN_POINT('Ctrl Pts',(30.5822541976098,-33.7798050832478,170.628950991683));
#36700=CARTESIAN_POINT('Ctrl Pts',(29.7357627108441,-31.7743037595668,170.517821202464));
#36701=CARTESIAN_POINT('Ctrl Pts',(30.9614766364829,-29.9753571875565,170.406691413244));
#36702=CARTESIAN_POINT('Ctrl Pts',(33.1376358820957,-30.0293417611574,170.295561624024));
#36703=CARTESIAN_POINT('Ctrl Pts',(34.2726431055619,-31.8868513840484,170.184431834804));
#36704=CARTESIAN_POINT('Ctrl Pts',(33.327752004606,-33.8479133932125,170.073302045585));
#36705=CARTESIAN_POINT('Ctrl Pts',(31.1677166679057,-34.117785104695,169.962172256365));
#36706=CARTESIAN_POINT('Ctrl Pts',(29.7693780110011,-32.4494828547835,169.851042467145));
#36707=CARTESIAN_POINT('Ctrl Pts',(30.4124804083402,-30.369818770613,169.739912677925));
#36708=CARTESIAN_POINT('Ctrl Pts',(32.5084635200333,-29.7820788689979,169.628782888706));
#36709=CARTESIAN_POINT('Ctrl Pts',(34.139106332249,-31.2241563341233,169.517653099486));
#36710=CARTESIAN_POINT('Ctrl Pts',(33.8120622268332,-33.3762775085839,169.406523310266));
#36711=CARTESIAN_POINT('Ctrl Pts',(31.8266384224149,-34.2688444322986,169.295393521047));
#36712=CARTESIAN_POINT('Ctrl Pts',(29.9998732537773,-33.0849895361627,169.184263731827));
#36713=CARTESIAN_POINT('Ctrl Pts',(30.0036023928055,-30.908163982761,169.073133942607));
#36714=CARTESIAN_POINT('Ctrl Pts',(31.8344129719196,-29.73057491185,168.962004153387));
#36715=CARTESIAN_POINT('Ctrl Pts',(33.8167670033918,-30.62993907076,168.850874364168));
#36716=CARTESIAN_POINT('Ctrl Pts',(34.1364355754274,-32.7831681343442,168.739744574948));
#36717=CARTESIAN_POINT('Ctrl Pts',(32.5008614774095,-34.2196502146324,168.628614785728));
#36718=CARTESIAN_POINT('Ctrl Pts',(30.4069043870894,-33.6247324892858,168.517484996508));
#36719=CARTESIAN_POINT('Ctrl Pts',(29.7709311248822,-31.5428772098609,168.406355207289));
#36720=CARTESIAN_POINT('Ctrl Pts',(31.1749775247933,-29.8793757494069,168.295225418069));
#36721=CARTESIAN_POINT('Ctrl Pts',(33.3340755452748,-30.1566466084773,168.184095628849));
#36722=CARTESIAN_POINT('Ctrl Pts',(34.2722420977155,-32.1209344958534,168.072965839629));
#36723=CARTESIAN_POINT('Ctrl Pts',(33.1308773165435,-33.974544454855,167.96183605041));
#36724=CARTESIAN_POINT('Ctrl Pts',(30.9545458938293,-34.0210727199301,167.85070626119));
#36725=CARTESIAN_POINT('Ctrl Pts',(29.7350027016688,-32.2179371939027,167.73957647197));
#36726=CARTESIAN_POINT('Ctrl Pts',(30.588360535013,-30.2153478207362,167.628446682751));
#36727=CARTESIAN_POINT('Ctrl Pts',(32.7336353740468,-29.8460529529552,167.517316893531));
#36728=CARTESIAN_POINT('Ctrl Pts',(34.2074953272919,-31.4480266880878,167.406187104311));
#36729=CARTESIAN_POINT('Ctrl Pts',(33.6610789820475,-33.5551611777726,167.295057315091));
#36730=CARTESIAN_POINT('Ctrl Pts',(31.5944622129986,-34.2390274643665,167.183927525872));
#36731=CARTESIAN_POINT('Ctrl Pts',(29.8989870973908,-32.8737632690876,167.072797736652));
#36732=CARTESIAN_POINT('Ctrl Pts',(30.1263405447975,-30.7088339472683,166.961667947432));
#36733=CARTESIAN_POINT('Ctrl Pts',(32.06843797294,-29.7255789427341,166.850538158213));
#36734=CARTESIAN_POINT('Ctrl Pts',(33.9479196943688,-30.8238226576517,166.739408368993));
#36735=CARTESIAN_POINT('Ctrl Pts',(34.0446498234045,-32.9985456146712,166.628278579773));
#36736=CARTESIAN_POINT('Ctrl Pts',(32.2702131443668,-34.2592995138028,166.517148790553));
#36737=CARTESIAN_POINT('Ctrl Pts',(30.2483285803673,-33.4525928567512,166.406019001334));
#36738=CARTESIAN_POINT('Ctrl Pts',(29.8298636342772,-31.3160291291474,166.294889212114));
#36739=CARTESIAN_POINT('Ctrl Pts',(31.3968549514422,-29.8063646067977,166.183759422894));
#36740=CARTESIAN_POINT('Ctrl Pts',(33.517118507477,-30.3023761829087,166.072629633675));
#36741=CARTESIAN_POINT('Ctrl Pts',(34.2462982339988,-32.3559841751676,165.961499844455));
#36742=CARTESIAN_POINT('Ctrl Pts',(33.3653042902584,-33.5006534350284,165.887413318308));
#36743=CARTESIAN_POINT('Ctrl Pts',(32.7800936946503,-33.7600342388747,165.850370055235));
#36744=CARTESIAN_POINT('Ctrl Pts',(31.5367004230124,-33.7347832743336,179.149629944765));
#36745=CARTESIAN_POINT('Ctrl Pts',(30.9598857617972,-33.5807363726283,179.112586681692));
#36746=CARTESIAN_POINT('Ctrl Pts',(29.9820798907776,-32.6539720077587,179.038500155545));
#36747=CARTESIAN_POINT('Ctrl Pts',(30.3558661308426,-30.6560992678324,178.927370366326));
#36748=CARTESIAN_POINT('Ctrl Pts',(32.2373452815599,-29.8914065306893,178.816240577106));
#36749=CARTESIAN_POINT('Ctrl Pts',(33.9001509585118,-31.054896938071,178.705110787886));
#36750=CARTESIAN_POINT('Ctrl Pts',(33.8246745117864,-33.0841069431875,178.593980998666));
#36751=CARTESIAN_POINT('Ctrl Pts',(32.0789243782558,-34.1207751988554,178.482851209447));
#36752=CARTESIAN_POINT('Ctrl Pts',(30.2611160949232,-33.2167190589247,178.371721420227));
#36753=CARTESIAN_POINT('Ctrl Pts',(30.0346307307857,-31.1990434357172,178.260591631007));
#36754=CARTESIAN_POINT('Ctrl Pts',(31.6068716487571,-29.9144394672662,178.149461841787));
#36755=CARTESIAN_POINT('Ctrl Pts',(33.5388789167773,-30.5384958299987,178.038332052568));
#36756=CARTESIAN_POINT('Ctrl Pts',(34.0625309354291,-32.5001157913711,177.927202263348));
#36757=CARTESIAN_POINT('Ctrl Pts',(32.6985720742161,-34.0040298835476,177.816072474128));
#36758=CARTESIAN_POINT('Ctrl Pts',(30.6952900504295,-33.6738801725007,177.704942684908));
#36759=CARTESIAN_POINT('Ctrl Pts',(29.8860632328111,-31.811812196359,177.593812895689));
#36760=CARTESIAN_POINT('Ctrl Pts',(31.011489004698,-30.1219722878469,177.482683106469));
#36761=CARTESIAN_POINT('Ctrl Pts',(33.0415890322462,-30.1508826654104,177.371553317249));
#36762=CARTESIAN_POINT('Ctrl Pts',(34.1184382141585,-31.8720853268838,177.26042352803));
#36763=CARTESIAN_POINT('Ctrl Pts',(33.2565156466643,-33.7103540352874,177.14929373881));
#36764=CARTESIAN_POINT('Ctrl Pts',(31.2446436197348,-33.9833253153198,177.03816394959));
#36765=CARTESIAN_POINT('Ctrl Pts',(29.9240655438013,-32.4411787570087,176.92703416037));
#36766=CARTESIAN_POINT('Ctrl Pts',(30.5033601778239,-30.4952701935241,176.815904371151));
#36767=CARTESIAN_POINT('Ctrl Pts',(32.4523633426839,-29.9264740264607,176.704774581931));
#36768=CARTESIAN_POINT('Ctrl Pts',(33.9873684839778,-31.2553463460645,176.593644792711));
#36769=CARTESIAN_POINT('Ctrl Pts',(33.7035555398755,-33.2657176132679,176.482515003491));
#36770=CARTESIAN_POINT('Ctrl Pts',(31.8606670404478,-34.11771784746,176.371385214272));
#36771=CARTESIAN_POINT('Ctrl Pts',(30.1452945543645,-33.0316056730973,176.260255425052));
#36772=CARTESIAN_POINT('Ctrl Pts',(30.127328378799,-31.0013791741379,176.149125635832));
#36773=CARTESIAN_POINT('Ctrl Pts',(31.8232109626221,-29.8850796253547,176.037995846613));
#36774=CARTESIAN_POINT('Ctrl Pts',(33.6808889562839,-30.7043322681203,175.926866057393));
#36775=CARTESIAN_POINT('Ctrl Pts',(34.0002356056227,-32.7093659681561,175.815736268173));
#36776=CARTESIAN_POINT('Ctrl Pts',(32.4889883203542,-34.0651956268962,175.704606478953));
#36777=CARTESIAN_POINT('Ctrl Pts',(30.5302242271517,-33.5309806440114,175.593476689734));
#36778=CARTESIAN_POINT('Ctrl Pts',(29.9165829822071,-31.5956287785228,175.482346900514));
#36779=CARTESIAN_POINT('Ctrl Pts',(31.2096623982289,-30.030353069706,175.371217111294));
#36780=CARTESIAN_POINT('Ctrl Pts',(33.2260502165377,-30.2676768715632,175.260087322075));
#36781=CARTESIAN_POINT('Ctrl Pts',(34.1203701726319,-32.0904040143035,175.148957532855));
#36782=CARTESIAN_POINT('Ctrl Pts',(33.0741503411905,-33.8303943835441,175.037827743635));
#36783=CARTESIAN_POINT('Ctrl Pts',(31.0448797661669,-33.8952276627656,174.926697954415));
#36784=CARTESIAN_POINT('Ctrl Pts',(29.8897248712998,-32.2255691379122,174.815568165196));
#36785=CARTESIAN_POINT('Ctrl Pts',(30.6658708892383,-30.349472184237,174.704438375976));
#36786=CARTESIAN_POINT('Ctrl Pts',(32.6629974013181,-29.9839203883193,174.593308586756));
#36787=CARTESIAN_POINT('Ctrl Pts',(34.0533558816191,-31.4634627895388,174.482178797536));
#36788=CARTESIAN_POINT('Ctrl Pts',(33.5645053267795,-33.4340382272686,174.371049008317));
#36789=CARTESIAN_POINT('Ctrl Pts',(31.6438364632251,-34.0921974308992,174.259919219097));
#36790=CARTESIAN_POINT('Ctrl Pts',(30.0491246060944,-32.8356002347072,174.148789429877));
#36791=CARTESIAN_POINT('Ctrl Pts',(30.2398327531034,-30.8142707654184,174.037659640658));
#36792=CARTESIAN_POINT('Ctrl Pts',(32.0414268762532,-29.8781078329205,173.926529851438));
#36793=CARTESIAN_POINT('Ctrl Pts',(33.8051075715119,-30.8838776007715,173.815400062218));
#36794=CARTESIAN_POINT('Ctrl Pts',(33.9167733928993,-32.9111104845529,173.704270272998));
#36795=CARTESIAN_POINT('Ctrl Pts',(32.2742289916473,-34.1045049334533,173.593140483779));
#36796=CARTESIAN_POINT('Ctrl Pts',(30.3807131911291,-33.3718792896629,173.482010694559));
#36797=CARTESIAN_POINT('Ctrl Pts',(29.9691511176554,-31.3837245973844,173.370880905339));
#36798=CARTESIAN_POINT('Ctrl Pts',(31.4161999176645,-29.9595784703513,173.25975111612));
#36799=CARTESIAN_POINT('Ctrl Pts',(33.3975362219787,-30.4028039998025,173.1486213269));
#36800=CARTESIAN_POINT('Ctrl Pts',(34.0998625315873,-32.3077659877652,173.03749153768));
#36801=CARTESIAN_POINT('Ctrl Pts',(32.8804174243481,-33.9310638813083,172.92636174846));
#36802=CARTESIAN_POINT('Ctrl Pts',(30.8552238380749,-33.7870730521938,172.81523195924));
#36803=CARTESIAN_POINT('Ctrl Pts',(29.877716980615,-32.0075723457118,172.704102170021));
#36804=CARTESIAN_POINT('Ctrl Pts',(30.8425005272953,-30.221141510553,172.592972380801));
#36805=CARTESIAN_POINT('Ctrl Pts',(32.8666150388358,-30.0627026740191,172.481842591581));
#36806=CARTESIAN_POINT('Ctrl Pts',(34.0976128648825,-31.6772573411082,172.370712802362));
#36807=CARTESIAN_POINT('Ctrl Pts',(33.4088981446531,-33.5871825896167,172.259583013142));
#36808=CARTESIAN_POINT('Ctrl Pts',(31.4307751213012,-34.0445355443865,172.148453223922));
#36809=CARTESIAN_POINT('Ctrl Pts',(29.9736005339478,-32.6307517409984,172.037323434702));
#36810=CARTESIAN_POINT('Ctrl Pts',(30.3709647625382,-30.6397107844664,171.926193645483));
#36811=CARTESIAN_POINT('Ctrl Pts',(32.2592043743021,-29.8935917662685,171.815063856263));
#36812=CARTESIAN_POINT('Ctrl Pts',(33.9102229536591,-31.0752347205356,171.703934067043));
#36813=CARTESIAN_POINT('Ctrl Pts',(33.8130262013327,-33.1032128299065,171.592804277823));
#36814=CARTESIAN_POINT('Ctrl Pts',(32.056567530997,-34.1215425211921,171.481674488604));
#36815=CARTESIAN_POINT('Ctrl Pts',(30.2483388697421,-33.1982595042532,171.370544699384));
#36816=CARTESIAN_POINT('Ctrl Pts',(30.0432114789254,-31.178342383605,171.259414910164));
#36817=CARTESIAN_POINT('Ctrl Pts',(31.6289157221082,-29.9103974029757,171.148285120945));
#36818=CARTESIAN_POINT('Ctrl Pts',(33.5542322721762,-30.5548340583465,171.037155331725));
#36819=CARTESIAN_POINT('Ctrl Pts',(34.0571323016956,-32.5218709113466,170.926025542505));
#36820=CARTESIAN_POINT('Ctrl Pts',(32.6773671573741,-34.0112971657366,170.814895753285));
#36821=CARTESIAN_POINT('Ctrl Pts',(30.6776829363647,-33.6600060656541,170.703765964066));
#36822=CARTESIAN_POINT('Ctrl Pts',(29.8881689520629,-31.789495416301,170.592636174846));
#36823=CARTESIAN_POINT('Ctrl Pts',(31.0313798409791,-30.1116362791222,170.481506385626));
#36824=CARTESIAN_POINT('Ctrl Pts',(33.0610613951829,-30.1619871408389,170.370376596406));
#36825=CARTESIAN_POINT('Ctrl Pts',(34.1196710672471,-31.8944674388404,170.259246807187));
#36826=CARTESIAN_POINT('Ctrl Pts',(33.2383807654422,-33.7235299923622,170.148117017967));
#36827=CARTESIAN_POINT('Ctrl Pts',(31.2237378167849,-33.9752365877787,170.036987228748));
#36828=CARTESIAN_POINT('Ctrl Pts',(29.9195215999931,-32.4192280786088,169.925857439527));
#36829=CARTESIAN_POINT('Ctrl Pts',(30.519336653039,-30.4795465782356,169.814727650308));
#36830=CARTESIAN_POINT('Ctrl Pts',(32.4742387440983,-29.9313675608301,169.703597861088));
#36831=CARTESIAN_POINT('Ctrl Pts',(33.9951226794636,-31.2763785183688,169.592468071869));
#36832=CARTESIAN_POINT('Ctrl Pts',(33.690091974789,-33.2836400085472,169.481338282649));
#36833=CARTESIAN_POINT('Ctrl Pts',(31.8383074230704,-34.1161280834014,169.370208493429));
#36834=CARTESIAN_POINT('Ctrl Pts',(30.1345021642776,-33.0119586847762,169.259078704209));
#36835=CARTESIAN_POINT('Ctrl Pts',(30.1379802942507,-30.9816556720869,169.14794891499));
#36836=CARTESIAN_POINT('Ctrl Pts',(31.845558666174,-29.8833303448027,169.03681912577));
#36837=CARTESIAN_POINT('Ctrl Pts',(33.6944800719454,-30.7221581316624,168.92568933655));
#36838=CARTESIAN_POINT('Ctrl Pts',(33.9926316917901,-32.7304529387375,168.81455954733));
#36839=CARTESIAN_POINT('Ctrl Pts',(32.4671483964048,-34.0702451378531,168.703429758111));
#36840=CARTESIAN_POINT('Ctrl Pts',(30.5141359548357,-33.5153714373925,168.592299968891));
#36841=CARTESIAN_POINT('Ctrl Pts',(29.9209701734844,-31.5736462315329,168.481170179671));
#36842=CARTESIAN_POINT('Ctrl Pts',(31.2305099440188,-30.0221153697719,168.370040390451));
#36843=CARTESIAN_POINT('Ctrl Pts',(33.2442786673897,-30.2807230747493,168.258910601232));
#36844=CARTESIAN_POINT('Ctrl Pts',(34.1192970513148,-32.1127943720091,168.147780812012));
#36845=CARTESIAN_POINT('Ctrl Pts',(33.0547577499595,-33.841637493237,168.036651022792));
#36846=CARTESIAN_POINT('Ctrl Pts',(31.0249156079274,-33.8850339319685,167.925521233573));
#36847=CARTESIAN_POINT('Ctrl Pts',(29.8874600992493,-32.2032678000614,167.814391444353));
#36848=CARTESIAN_POINT('Ctrl Pts',(30.6833782550396,-30.3354730972818,167.703261655133));
#36849=CARTESIAN_POINT('Ctrl Pts',(32.6842542379269,-29.9910355370672,167.592131865913));
#36850=CARTESIAN_POINT('Ctrl Pts',(34.0589083982841,-31.4851801163634,167.481002076694));
#36851=CARTESIAN_POINT('Ctrl Pts',(33.5492714408353,-33.4504829840476,167.369872287474));
#36852=CARTESIAN_POINT('Ctrl Pts',(31.6217590383292,-34.0883181012338,167.258742498254));
#36853=CARTESIAN_POINT('Ctrl Pts',(30.0404066742048,-32.8149500977851,167.147612709034));
#36854=CARTESIAN_POINT('Ctrl Pts',(30.2524569179617,-30.7957425790749,167.036482919815));
#36855=CARTESIAN_POINT('Ctrl Pts',(32.063831400006,-29.8786706553152,166.925353130595));
#36856=CARTESIAN_POINT('Ctrl Pts',(33.816804850427,-30.9029913775613,166.814223341375));
#36857=CARTESIAN_POINT('Ctrl Pts',(33.9070240561379,-32.9313333200294,166.703093552155));
#36858=CARTESIAN_POINT('Ctrl Pts',(32.2520250463887,-34.1072256351791,166.591963762936));
#36859=CARTESIAN_POINT('Ctrl Pts',(30.3662339157292,-33.3548185561604,166.480833973716));
#36860=CARTESIAN_POINT('Ctrl Pts',(29.9759359244988,-31.3620673381413,166.369704184496));
#36861=CARTESIAN_POINT('Ctrl Pts',(31.4374527590133,-29.9540186210142,166.258574395277));
#36862=CARTESIAN_POINT('Ctrl Pts',(33.4150009731022,-30.4166435638964,166.147444606057));
#36863=CARTESIAN_POINT('Ctrl Pts',(34.0950994739837,-32.3320228128446,166.036314816837));
#36864=CARTESIAN_POINT('Ctrl Pts',(33.2734053996277,-33.3996441678017,165.962228290691));
#36865=CARTESIAN_POINT('Ctrl Pts',(32.7275854401623,-33.6415660005642,165.925185027618));
#36866=CARTESIAN_POINT('Ctrl Pts',(31.5701357431134,-33.6095877486647,179.224444917147));
#36867=CARTESIAN_POINT('Ctrl Pts',(31.0349485380725,-33.4666580759078,179.187401654074));
#36868=CARTESIAN_POINT('Ctrl Pts',(30.1277087843517,-32.6067762741501,179.113315127928));
#36869=CARTESIAN_POINT('Ctrl Pts',(30.4745196866295,-30.7530856528753,179.002185338708));
#36870=CARTESIAN_POINT('Ctrl Pts',(32.2202165901956,-30.0435791229192,178.891055549488));
#36871=CARTESIAN_POINT('Ctrl Pts',(33.7630212077119,-31.1231029649564,178.779925760268));
#36872=CARTESIAN_POINT('Ctrl Pts',(33.6929917315466,-33.0058693093333,178.668795971049));
#36873=CARTESIAN_POINT('Ctrl Pts',(32.0732285779965,-33.9677234777703,178.557666181829));
#36874=CARTESIAN_POINT('Ctrl Pts',(30.3866075541702,-33.1289110978801,178.446536392609));
#36875=CARTESIAN_POINT('Ctrl Pts',(30.17646714484,-31.2568467242241,178.33540660339));
#36876=CARTESIAN_POINT('Ctrl Pts',(31.6352428645265,-30.064949822694,178.22427681417));
#36877=CARTESIAN_POINT('Ctrl Pts',(33.4278213813623,-30.6439693986789,178.11314702495));
#36878=CARTESIAN_POINT('Ctrl Pts',(33.9136825758156,-32.4640235253674,178.002017235731));
#36879=CARTESIAN_POINT('Ctrl Pts',(32.6481576510757,-33.8594034172685,177.890887446511));
#36880=CARTESIAN_POINT('Ctrl Pts',(30.7894481221602,-33.5530798908727,177.779757657291));
#36881=CARTESIAN_POINT('Ctrl Pts',(30.0386214391961,-31.8253932997452,177.668627868071));
#36882=CARTESIAN_POINT('Ctrl Pts',(31.0828276874703,-30.2575054522038,177.557498078852));
#36883=CARTESIAN_POINT('Ctrl Pts',(32.9664198233009,-30.2843294308667,177.446368289632));
#36884=CARTESIAN_POINT('Ctrl Pts',(33.9655551481625,-31.8813166498845,177.335238500412));
#36885=CARTESIAN_POINT('Ctrl Pts',(33.1658356526715,-33.5869215145248,177.224108711192));
#36886=CARTESIAN_POINT('Ctrl Pts',(31.2991560424068,-33.8401930525768,177.112978921973));
#36887=CARTESIAN_POINT('Ctrl Pts',(30.0738812062782,-32.4093398482442,177.001849132753));
#36888=CARTESIAN_POINT('Ctrl Pts',(30.6113694098972,-30.6038632621215,176.890719343533));
#36889=CARTESIAN_POINT('Ctrl Pts',(32.4197172667628,-30.0761158739965,176.779589554313));
#36890=CARTESIAN_POINT('Ctrl Pts',(33.8439444345702,-31.3090863763179,176.668459765094));
#36891=CARTESIAN_POINT('Ctrl Pts',(33.5806136517005,-33.1743735334131,176.557329975874));
#36892=CARTESIAN_POINT('Ctrl Pts',(31.8707223962794,-33.9648867687576,176.446200186654));
#36893=CARTESIAN_POINT('Ctrl Pts',(30.2791446016083,-32.9571569414099,176.335070397435));
#36894=CARTESIAN_POINT('Ctrl Pts',(30.2624750057525,-31.0734474613341,176.223940608215));
#36895=CARTESIAN_POINT('Ctrl Pts',(31.8359694419057,-30.0377088165447,176.112810818995));
#36896=CARTESIAN_POINT('Ctrl Pts',(33.5595828660151,-30.7978377827197,176.001681029775));
#36897=CARTESIAN_POINT('Ctrl Pts',(33.8558829641068,-32.6581725732295,175.890551240556));
#36898=CARTESIAN_POINT('Ctrl Pts',(32.4536990996669,-33.9161549623108,175.779421451336));
#36899=CARTESIAN_POINT('Ctrl Pts',(30.6362947393706,-33.4204931097171,175.668291662116));
#36900=CARTESIAN_POINT('Ctrl Pts',(30.0669386448361,-31.6248113677183,175.557161872896));
#36901=CARTESIAN_POINT('Ctrl Pts',(31.2666993393694,-30.1724981932316,175.446032083677));
#36902=CARTESIAN_POINT('Ctrl Pts',(33.1375688461977,-30.3926948538679,175.334902294457));
#36903=CARTESIAN_POINT('Ctrl Pts',(33.9673476814061,-32.0838797537456,175.223772505237));
#36904=CARTESIAN_POINT('Ctrl Pts',(32.9966312535889,-33.6982988126334,175.112642716018));
#36905=CARTESIAN_POINT('Ctrl Pts',(31.113808710503,-33.7584532154829,175.001512926798));
#36906=CARTESIAN_POINT('Ctrl Pts',(30.0420188252204,-32.2092903051534,174.890383137578));
#36907=CARTESIAN_POINT('Ctrl Pts',(30.7621520776745,-30.4685871772064,174.779253348358));
#36908=CARTESIAN_POINT('Ctrl Pts',(32.615150324739,-30.1294164571996,174.668123559139));
#36909=CARTESIAN_POINT('Ctrl Pts',(33.90516966563,-31.5021835099298,174.556993769919));
#36910=CARTESIAN_POINT('Ctrl Pts',(33.451598389241,-33.3305468157773,174.445863980699));
#36911=CARTESIAN_POINT('Ctrl Pts',(31.6695400089477,-33.9412081050047,174.334734191479));
#36912=CARTESIAN_POINT('Ctrl Pts',(30.1899150287761,-32.7752967880571,174.22360440226));
#36913=CARTESIAN_POINT('Ctrl Pts',(30.3668601847145,-30.8998422584232,174.11247461304));
#36914=CARTESIAN_POINT('Ctrl Pts',(32.0384371889383,-30.0312401631664,174.00134482382));
#36915=CARTESIAN_POINT('Ctrl Pts',(33.6748368946798,-30.9644257202684,173.890215034601));
#36916=CARTESIAN_POINT('Ctrl Pts',(33.7784440372601,-32.8453576278453,173.779085245381));
#36917=CARTESIAN_POINT('Ctrl Pts',(32.2544384833625,-33.9526274019399,173.667955456161));
#36918=CARTESIAN_POINT('Ctrl Pts',(30.4975735887619,-33.2728737531416,173.556825666941));
#36919=CARTESIAN_POINT('Ctrl Pts',(30.1157130525905,-31.4281998492091,173.445695877722));
#36920=CARTESIAN_POINT('Ctrl Pts',(31.4583314964472,-30.1068312423661,173.334566088502));
#36921=CARTESIAN_POINT('Ctrl Pts',(33.2966790806051,-30.5180701519493,173.223436299282));
#36922=CARTESIAN_POINT('Ctrl Pts',(33.9483200320923,-32.2855551876086,173.112306510063));
#36923=CARTESIAN_POINT('Ctrl Pts',(32.8168796188595,-33.7917032122855,173.001176720843));
#36924=CARTESIAN_POINT('Ctrl Pts',(30.9378398371371,-33.658103887291,172.890046931623));
#36925=CARTESIAN_POINT('Ctrl Pts',(30.0308775178194,-32.0070258660356,172.778917142403));
#36926=CARTESIAN_POINT('Ctrl Pts',(30.9260347399493,-30.3495178483768,172.667787353183));
#36927=CARTESIAN_POINT('Ctrl Pts',(32.8040733214092,-30.2025131971499,172.556657563964));
#36928=CARTESIAN_POINT('Ctrl Pts',(33.9462327189276,-31.7005489749587,172.445527774744));
#36929=CARTESIAN_POINT('Ctrl Pts',(33.3072210380983,-33.4726390834741,172.334397985525));
#36930=CARTESIAN_POINT('Ctrl Pts',(31.4718548394233,-33.8969858728999,172.223268196305));
#36931=CARTESIAN_POINT('Ctrl Pts',(30.1198413642124,-32.5852317634028,172.112138407085));
#36932=CARTESIAN_POINT('Ctrl Pts',(30.4885286830029,-30.7378798906137,172.001008617865));
#36933=CARTESIAN_POINT('Ctrl Pts',(32.2404981598852,-30.0456066548122,171.889878828646));
#36934=CARTESIAN_POINT('Ctrl Pts',(33.7723663289346,-31.1419730140134,171.778749039426));
#36935=CARTESIAN_POINT('Ctrl Pts',(33.6821840542554,-33.0235963658742,171.667619250206));
#36936=CARTESIAN_POINT('Ctrl Pts',(32.0524851756482,-33.9684354241274,171.556489460986));
#36937=CARTESIAN_POINT('Ctrl Pts',(30.3747524334657,-33.1117837290124,171.445359671766));
#36938=CARTESIAN_POINT('Ctrl Pts',(30.1844286390995,-31.2376396218978,171.334229882547));
#36939=CARTESIAN_POINT('Ctrl Pts',(31.6556960651779,-30.0611994653682,171.223100093327));
#36940=CARTESIAN_POINT('Ctrl Pts',(33.4420667185848,-30.6591285327175,171.111970304107));
#36941=CARTESIAN_POINT('Ctrl Pts',(33.9086735497053,-32.4842086257781,171.000840514888));
#36942=CARTESIAN_POINT('Ctrl Pts',(32.6284830468382,-33.8661462355505,170.889710725668));
#36943=CARTESIAN_POINT('Ctrl Pts',(30.7731116751197,-33.5402070480603,170.778580936448));
#36944=CARTESIAN_POINT('Ctrl Pts',(30.0405751932818,-31.8046870730353,170.667451147228));
#36945=CARTESIAN_POINT('Ctrl Pts',(31.1012830454752,-30.2479153706878,170.556321358009));
#36946=CARTESIAN_POINT('Ctrl Pts',(32.9844869082701,-30.2946325205203,170.445191568789));
#36947=CARTESIAN_POINT('Ctrl Pts',(33.9666990289323,-31.9020834936324,170.334061779569));
#36948=CARTESIAN_POINT('Ctrl Pts',(33.1490095262784,-33.5991465915118,170.222931990349));
#36949=CARTESIAN_POINT('Ctrl Pts',(31.279758965664,-33.8326880708624,170.11180220113));
#36950=CARTESIAN_POINT('Ctrl Pts',(30.0696651889851,-32.3889733024341,170.00067241191));
#36951=CARTESIAN_POINT('Ctrl Pts',(30.6261928977377,-30.5892743858582,169.889542622691));
#36952=CARTESIAN_POINT('Ctrl Pts',(32.4400139681632,-30.0806562526623,169.77841283347));
#36953=CARTESIAN_POINT('Ctrl Pts',(33.8511390266782,-31.3286007026142,169.667283044251));
#36954=CARTESIAN_POINT('Ctrl Pts',(33.5681217227447,-33.1910025085104,169.556153255031));
#36955=CARTESIAN_POINT('Ctrl Pts',(31.849976423726,-33.9634117345042,169.445023465811));
#36956=CARTESIAN_POINT('Ctrl Pts',(30.2691310747778,-32.9389278333895,169.333893676592));
#36957=CARTESIAN_POINT('Ctrl Pts',(30.2723581956959,-31.0551473614128,169.222763887372));
#36958=CARTESIAN_POINT('Ctrl Pts',(31.8567043604284,-30.0360857777554,169.111634098152));
#36959=CARTESIAN_POINT('Ctrl Pts',(33.572193140499,-30.8143771925649,169.000504308933));
#36960=CARTESIAN_POINT('Ctrl Pts',(33.8488278081528,-32.6777377431309,168.889374519713));
#36961=CARTESIAN_POINT('Ctrl Pts',(32.4334353154,-33.920840061074,168.778244730493));
#36962=CARTESIAN_POINT('Ctrl Pts',(30.6213675225821,-33.4060103854991,168.667114941273));
#36963=CARTESIAN_POINT('Ctrl Pts',(30.0710092220866,-31.6044152532049,168.555985152054));
#36964=CARTESIAN_POINT('Ctrl Pts',(31.2860423632443,-30.1648549901369,168.444855362834));
#36965=CARTESIAN_POINT('Ctrl Pts',(33.1544817895046,-30.4047995410214,168.333725573614));
#36966=CARTESIAN_POINT('Ctrl Pts',(33.9663520049142,-32.1046542481647,168.222595784395));
#36967=CARTESIAN_POINT('Ctrl Pts',(32.9786381833754,-33.7087305316189,168.111465995175));
#36968=CARTESIAN_POINT('Ctrl Pts',(31.0952853220256,-33.7489951440067,168.000336205955));
#36969=CARTESIAN_POINT('Ctrl Pts',(30.0399174968298,-32.1885984062203,167.889206416735));
#36970=CARTESIAN_POINT('Ctrl Pts',(30.7783959750662,-30.4555983738273,167.778076627515));
#36971=CARTESIAN_POINT('Ctrl Pts',(32.634873101807,-30.1360181211792,167.666946838296));
#36972=CARTESIAN_POINT('Ctrl Pts',(33.9103214692762,-31.522333544639,167.555817049076));
#36973=CARTESIAN_POINT('Ctrl Pts',(33.4374638996232,-33.3458047903225,167.444687259856));
#36974=CARTESIAN_POINT('Ctrl Pts',(31.6490558636597,-33.9376087381012,167.333557470637));
#36975=CARTESIAN_POINT('Ctrl Pts',(30.1818262510189,-32.7561369264825,167.222427681417));
#36976=CARTESIAN_POINT('Ctrl Pts',(30.3785732911259,-30.8826512108817,167.111297892197));
#36977=CARTESIAN_POINT('Ctrl Pts',(32.059224827072,-30.0317623678963,167.000168102977));
#36978=CARTESIAN_POINT('Ctrl Pts',(33.6856900064852,-30.9821600974709,166.889038313758));
#36979=CARTESIAN_POINT('Ctrl Pts',(33.7693982888712,-32.8641210253877,166.777908524538));
#36980=CARTESIAN_POINT('Ctrl Pts',(32.2338369484106,-33.9551517565555,166.666778735318));
#36981=CARTESIAN_POINT('Ctrl Pts',(30.484139251091,-33.2570442555697,166.555648946099));
#36982=CARTESIAN_POINT('Ctrl Pts',(30.1220082147204,-31.4081055471351,166.444519156879));
#36983=CARTESIAN_POINT('Ctrl Pts',(31.4780505665844,-30.1016726352307,166.333389367659));
#36984=CARTESIAN_POINT('Ctrl Pts',(33.3128834387275,-30.530910944884,166.222259578439));
#36985=CARTESIAN_POINT('Ctrl Pts',(33.9439007139686,-32.3080614505216,166.11112978922));
#36986=CARTESIAN_POINT('Ctrl Pts',(33.1815065089969,-33.2986349005751,166.037043263073));
#36987=CARTESIAN_POINT('Ctrl Pts',(32.6750771856743,-33.5230977622536,166.));
#36988=CARTESIAN_POINT('Ctrl Pts',(30.3361334267378,-31.9990537049732,178.37851963661));
#36989=CARTESIAN_POINT('Ctrl Pts',(30.3350134860168,-31.7834929963847,178.364148625536));
#36990=CARTESIAN_POINT('Ctrl Pts',(30.3738847213991,-31.5683196627767,178.349777614463));
#36991=CARTESIAN_POINT('Ctrl Pts',(30.4546198330094,-31.3702079695784,178.33540660339));
#36992=CARTESIAN_POINT('Ctrl Pts',(30.6627257180688,-30.8595477570474,178.298363340316));
#36993=CARTESIAN_POINT('Ctrl Pts',(31.1489842912976,-30.4622487898707,178.261320077243));
#36994=CARTESIAN_POINT('Ctrl Pts',(31.6908766640514,-30.3601025689465,178.22427681417));
#36995=CARTESIAN_POINT('Ctrl Pts',(32.2327690368051,-30.2579563480223,178.187233551097));
#36996=CARTESIAN_POINT('Ctrl Pts',(32.8302952090837,-30.4509628733506,178.150190288023));
#36997=CARTESIAN_POINT('Ctrl Pts',(33.2100351609652,-30.8508084904628,178.11314702495));
#36998=CARTESIAN_POINT('Ctrl Pts',(33.5897751128467,-31.2506541075751,178.076103761877));
#36999=CARTESIAN_POINT('Ctrl Pts',(33.7517288443312,-31.8573388164712,178.039060498804));
#37000=CARTESIAN_POINT('Ctrl Pts',(33.6217848892834,-32.3932444862362,178.002017235731));
#37001=CARTESIAN_POINT('Ctrl Pts',(33.4918409342357,-32.9291501560011,177.964973972657));
#37002=CARTESIAN_POINT('Ctrl Pts',(33.0699992926557,-33.3942767866348,177.927930709584));
#37003=CARTESIAN_POINT('Ctrl Pts',(32.5492935503798,-33.5757861808857,177.890887446511));
#37004=CARTESIAN_POINT('Ctrl Pts',(32.0285878081039,-33.7572955751366,177.853844183437));
#37005=CARTESIAN_POINT('Ctrl Pts',(31.4090179651321,-33.6551877330046,177.816800920364));
#37006=CARTESIAN_POINT('Ctrl Pts',(30.9740952631521,-33.3161860467508,177.779757657291));
#37007=CARTESIAN_POINT('Ctrl Pts',(30.5778854457224,-33.0073592239439,177.746011650397));
#37008=CARTESIAN_POINT('Ctrl Pts',(30.3349144830452,-32.5019339530042,177.712265643504));
#37009=CARTESIAN_POINT('Ctrl Pts',(30.3317668085256,-31.999144727569,177.67851963661));
#37010=CARTESIAN_POINT('Ctrl Pts',(31.4698297828105,-33.9851743256715,179.));
#37011=CARTESIAN_POINT('Ctrl Pts',(31.4011717473165,-33.959752800589,179.));
#37012=CARTESIAN_POINT('Ctrl Pts',(31.3342169943201,-33.9304405272318,179.));
#37013=CARTESIAN_POINT('Ctrl Pts',(31.2691543409406,-33.8975318476629,179.));
#37014=CARTESIAN_POINT('Ctrl Pts',(31.2022750469363,-33.8637043115593,179.));
#37015=CARTESIAN_POINT('Ctrl Pts',(31.1373942160753,-33.8260760433842,179.));
#37016=CARTESIAN_POINT('Ctrl Pts',(31.0747481415806,-33.7849220758473,179.));
#37017=CARTESIAN_POINT('Ctrl Pts',(31.0218168792491,-33.7501500415378,179.));
#37018=CARTESIAN_POINT('Ctrl Pts',(30.9704813415884,-33.7128599624529,179.));
#37019=CARTESIAN_POINT('Ctrl Pts',(30.9209067960986,-33.6731997220801,179.));
#37020=CARTESIAN_POINT('Ctrl Pts',(30.8988714343571,-33.6555711642237,179.));
#37021=CARTESIAN_POINT('Ctrl Pts',(30.8771842966684,-33.6374741525735,179.));
#37022=CARTESIAN_POINT('Ctrl Pts',(30.8558614512686,-33.6189209496161,179.));
#37023=CARTESIAN_POINT('Ctrl Pts',(30.8441499403614,-33.6087306567763,179.));
#37024=CARTESIAN_POINT('Ctrl Pts',(30.8325483440617,-33.5984027370162,179.));
#37025=CARTESIAN_POINT('Ctrl Pts',(30.8210594589826,-33.5879391805166,179.));
#37026=CARTESIAN_POINT('Ctrl Pts',(30.8104646008526,-33.5782898632951,179.));
#37027=CARTESIAN_POINT('Ctrl Pts',(30.79996415815,-33.5685236791905,179.));
#37028=CARTESIAN_POINT('Ctrl Pts',(30.7895762178146,-33.558657652978,179.));
#37029=CARTESIAN_POINT('Ctrl Pts',(30.7364925058988,-33.5082409893936,179.));
#37030=CARTESIAN_POINT('Ctrl Pts',(30.6862488283153,-33.4551355694144,179.));
#37031=CARTESIAN_POINT('Ctrl Pts',(30.6390637895127,-33.3996012573837,179.));
#37032=CARTESIAN_POINT('Ctrl Pts',(30.5922435997919,-33.3444963535567,179.));
#37033=CARTESIAN_POINT('Ctrl Pts',(30.5484344225798,-33.2869990900772,179.));
#37034=CARTESIAN_POINT('Ctrl Pts',(30.5078946257251,-33.2273391119527,179.));
#37035=CARTESIAN_POINT('Ctrl Pts',(30.4742099597326,-33.1777674171696,179.));
#37036=CARTESIAN_POINT('Ctrl Pts',(30.4427831212109,-33.1267019303825,179.));
#37037=CARTESIAN_POINT('Ctrl Pts',(30.4137899183792,-33.0742679245007,179.));
#37038=CARTESIAN_POINT('Ctrl Pts',(30.4016832373463,-33.0523730759677,179.));
#37039=CARTESIAN_POINT('Ctrl Pts',(30.3900012174127,-33.0302395674683,179.));
#37040=CARTESIAN_POINT('Ctrl Pts',(30.3787581006213,-33.0078764377137,179.));
#37041=CARTESIAN_POINT('Ctrl Pts',(30.3735598553067,-32.9975368640329,179.));
#37042=CARTESIAN_POINT('Ctrl Pts',(30.368455445269,-32.9871482050211,179.));
#37043=CARTESIAN_POINT('Ctrl Pts',(30.3634463432331,-32.9767113560277,179.));
#37044=CARTESIAN_POINT('Ctrl Pts',(30.3582116535791,-32.9658044778979,179.));
#37045=CARTESIAN_POINT('Ctrl Pts',(30.3530846523394,-32.9548524099599,179.));
#37046=CARTESIAN_POINT('Ctrl Pts',(30.3480684170179,-32.9438605003377,179.));
#37047=CARTESIAN_POINT('Ctrl Pts',(30.3195275433178,-32.8813198330565,179.));
#37048=CARTESIAN_POINT('Ctrl Pts',(30.2945476959897,-32.8174470078339,179.));
#37049=CARTESIAN_POINT('Ctrl Pts',(30.2733523004482,-32.752446851706,179.));
#37050=CARTESIAN_POINT('Ctrl Pts',(30.2541560082979,-32.6935773682653,179.));
#37051=CARTESIAN_POINT('Ctrl Pts',(30.2380642754967,-32.6337825821927,179.));
#37052=CARTESIAN_POINT('Ctrl Pts',(30.2252797403903,-32.5732098531994,179.));
#37053=CARTESIAN_POINT('Ctrl Pts',(30.2101450163511,-32.5015020022702,179.));
#37054=CARTESIAN_POINT('Ctrl Pts',(30.1996445746367,-32.4287023826296,179.));
#37055=CARTESIAN_POINT('Ctrl Pts',(30.1937033647945,-32.3552336691758,179.));
#37056=CARTESIAN_POINT('Ctrl Pts',(30.1923960684006,-32.3390677052201,179.));
#37057=CARTESIAN_POINT('Ctrl Pts',(30.1913097402832,-32.3228694274561,179.));
#37058=CARTESIAN_POINT('Ctrl Pts',(30.1904439498812,-32.3066435031514,179.));
#37059=CARTESIAN_POINT('Ctrl Pts',(30.1895460181996,-32.2898152136935,179.));
#37060=CARTESIAN_POINT('Ctrl Pts',(30.188885292102,-32.2729509603928,179.));
#37061=CARTESIAN_POINT('Ctrl Pts',(30.1884618549855,-32.2560903450774,179.));
#37062=CARTESIAN_POINT('Ctrl Pts',(30.1867401326158,-32.1875340059679,179.));
#37063=CARTESIAN_POINT('Ctrl Pts',(30.1889297256531,-32.1189513246165,179.));
#37064=CARTESIAN_POINT('Ctrl Pts',(30.1949101410477,-32.050680284215,179.));
#37065=CARTESIAN_POINT('Ctrl Pts',(30.2008893408697,-31.9824231205106,179.));
#37066=CARTESIAN_POINT('Ctrl Pts',(30.2106582755871,-31.9144764003355,179.));
#37067=CARTESIAN_POINT('Ctrl Pts',(30.224146128777,-31.8471929428052,179.));
#37068=CARTESIAN_POINT('Ctrl Pts',(30.2339040657141,-31.7985159794482,179.));
#37069=CARTESIAN_POINT('Ctrl Pts',(30.2456095194275,-31.7501864309561,179.));
#37070=CARTESIAN_POINT('Ctrl Pts',(30.2592498723843,-31.7023475393497,179.));
#37071=CARTESIAN_POINT('Ctrl Pts',(30.2694853564288,-31.6664500656337,179.));
#37072=CARTESIAN_POINT('Ctrl Pts',(30.2808105812034,-31.6308290228568,179.));
#37073=CARTESIAN_POINT('Ctrl Pts',(30.2932241308889,-31.595549108902,179.));
#37074=CARTESIAN_POINT('Ctrl Pts',(30.2973532985701,-31.5838138128595,179.));
#37075=CARTESIAN_POINT('Ctrl Pts',(30.3015996892027,-31.572125456135,179.));
#37076=CARTESIAN_POINT('Ctrl Pts',(30.3059626598347,-31.5604865933038,179.));
#37077=CARTESIAN_POINT('Ctrl Pts',(30.3290856768936,-31.4988025604527,179.));
#37078=CARTESIAN_POINT('Ctrl Pts',(30.3554815657399,-31.4385021658608,179.));
#37079=CARTESIAN_POINT('Ctrl Pts',(30.385100405382,-31.3799192305409,179.));
#37080=CARTESIAN_POINT('Ctrl Pts',(30.4059269993117,-31.3387264282618,179.));
#37081=CARTESIAN_POINT('Ctrl Pts',(30.4283479556147,-31.2983833101766,179.));
#37082=CARTESIAN_POINT('Ctrl Pts',(30.4523563132414,-31.2590172662485,179.));
#37083=CARTESIAN_POINT('Ctrl Pts',(30.4600693856112,-31.2463702892894,179.));
#37084=CARTESIAN_POINT('Ctrl Pts',(30.4679474502836,-31.233822557199,179.));
#37085=CARTESIAN_POINT('Ctrl Pts',(30.4759869645798,-31.2213839090576,179.));
#37086=CARTESIAN_POINT('Ctrl Pts',(30.5102319017654,-31.168400518695,179.));
#37087=CARTESIAN_POINT('Ctrl Pts',(30.5473331851848,-31.1175005866592,179.));
#37088=CARTESIAN_POINT('Ctrl Pts',(30.5872566410985,-31.0689991104218,179.));
#37089=CARTESIAN_POINT('Ctrl Pts',(30.6240225828063,-31.0243335771588,179.));
#37090=CARTESIAN_POINT('Ctrl Pts',(30.6631825310147,-30.9817020284588,179.));
#37091=CARTESIAN_POINT('Ctrl Pts',(30.7047312003651,-30.9413832981698,179.));
#37092=CARTESIAN_POINT('Ctrl Pts',(30.7125728983667,-30.9337737330097,179.));
#37093=CARTESIAN_POINT('Ctrl Pts',(30.7204997382999,-30.9262466564544,179.));
#37094=CARTESIAN_POINT('Ctrl Pts',(30.7285101132666,-30.9188027417083,179.));
#37095=CARTESIAN_POINT('Origin',(32.,-32.,172.));
#37096=CARTESIAN_POINT('Origin',(32.,-32.,165.));
#37097=CARTESIAN_POINT('Origin',(-32.,-32.,165.));
#37098=CARTESIAN_POINT('Origin',(-32.,32.,165.));
#37099=CARTESIAN_POINT('Origin',(32.,32.,165.));
#37100=CARTESIAN_POINT('Origin',(-32.,-32.,54.));
#37101=CARTESIAN_POINT('Ctrl Pts',(-32.6750771856749,-33.5230977622534,
54.));
#37102=CARTESIAN_POINT('Ctrl Pts',(-32.7347606773045,-33.5045114867892,
54.));
#37103=CARTESIAN_POINT('Ctrl Pts',(-32.7931316179784,-33.4823506253332,
54.));
#37104=CARTESIAN_POINT('Ctrl Pts',(-32.8500334557689,-33.4569140519098,
54.));
#37105=CARTESIAN_POINT('Ctrl Pts',(-32.88611617735,-33.4407841546612,54.));
#37106=CARTESIAN_POINT('Ctrl Pts',(-32.9216082071983,-33.4233359556206,
54.));
#37107=CARTESIAN_POINT('Ctrl Pts',(-32.9564687278967,-33.404635225715,54.));
#37108=CARTESIAN_POINT('Ctrl Pts',(-32.9802307380722,-33.3918882292444,
54.));
#37109=CARTESIAN_POINT('Ctrl Pts',(-33.0036993179247,-33.3785591155432,
54.));
#37110=CARTESIAN_POINT('Ctrl Pts',(-33.026861076465,-33.3646667567952,54.));
#37111=CARTESIAN_POINT('Ctrl Pts',(-33.0392102711152,-33.35725974398,54.));
#37112=CARTESIAN_POINT('Ctrl Pts',(-33.0514720828672,-33.3496925419692,
54.));
#37113=CARTESIAN_POINT('Ctrl Pts',(-33.0636323953525,-33.3419759097187,
54.));
#37114=CARTESIAN_POINT('Ctrl Pts',(-33.1193342204595,-33.3066289150955,
54.));
#37115=CARTESIAN_POINT('Ctrl Pts',(-33.1729722743323,-33.2681125032569,
54.));
#37116=CARTESIAN_POINT('Ctrl Pts',(-33.2243647334445,-33.2267291539377,
54.));
#37117=CARTESIAN_POINT('Ctrl Pts',(-33.2614335678882,-33.1968797839885,
54.));
#37118=CARTESIAN_POINT('Ctrl Pts',(-33.297334027751,-33.1655376472296,54.));
#37119=CARTESIAN_POINT('Ctrl Pts',(-33.3319925959414,-33.1328003832817,
54.));
#37120=CARTESIAN_POINT('Ctrl Pts',(-33.3414614125186,-33.1238564723314,
54.));
#37121=CARTESIAN_POINT('Ctrl Pts',(-33.3508375003105,-33.1148083596757,
54.));
#37122=CARTESIAN_POINT('Ctrl Pts',(-33.360119276131,-33.1056578841604,54.));
#37123=CARTESIAN_POINT('Ctrl Pts',(-33.3696833014298,-33.0962291518769,
54.));
#37124=CARTESIAN_POINT('Ctrl Pts',(-33.3791414850281,-33.0866973059031,
54.));
#37125=CARTESIAN_POINT('Ctrl Pts',(-33.3884886005182,-33.0770687715598,
54.));
#37126=CARTESIAN_POINT('Ctrl Pts',(-33.4357509408447,-33.0283834774211,
54.));
#37127=CARTESIAN_POINT('Ctrl Pts',(-33.4802063982923,-32.9771992571969,
54.));
#37128=CARTESIAN_POINT('Ctrl Pts',(-33.5216712678792,-32.9238232033015,
54.));
#37129=CARTESIAN_POINT('Ctrl Pts',(-33.5637353819771,-32.869675766121,54.));
#37130=CARTESIAN_POINT('Ctrl Pts',(-33.6027227351054,-32.8132721038918,
54.));
#37131=CARTESIAN_POINT('Ctrl Pts',(-33.6384171844749,-32.7548859058909,
54.));
#37132=CARTESIAN_POINT('Ctrl Pts',(-33.6605278962276,-32.7187189270709,
54.));
#37133=CARTESIAN_POINT('Ctrl Pts',(-33.6813745553917,-32.6817903356339,
54.));
#37134=CARTESIAN_POINT('Ctrl Pts',(-33.7008988738744,-32.6441579100733,
54.));
#37135=CARTESIAN_POINT('Ctrl Pts',(-33.716883135418,-32.6133488176477,54.));
#37136=CARTESIAN_POINT('Ctrl Pts',(-33.7319810240453,-32.5820678683706,
54.));
#37137=CARTESIAN_POINT('Ctrl Pts',(-33.7461572317173,-32.5503445540004,
54.));
#37138=CARTESIAN_POINT('Ctrl Pts',(-33.7519692674621,-32.5373384637026,
54.));
#37139=CARTESIAN_POINT('Ctrl Pts',(-33.7576272327853,-32.5242555213422,
54.));
#37140=CARTESIAN_POINT('Ctrl Pts',(-33.7631195251678,-32.5111202466595,
54.));
#37141=CARTESIAN_POINT('Ctrl Pts',(-33.7903101131696,-32.4460916907641,
54.));
#37142=CARTESIAN_POINT('Ctrl Pts',(-33.8134949920671,-32.3796713042743,
54.));
#37143=CARTESIAN_POINT('Ctrl Pts',(-33.8324625892457,-32.3121542210127,
54.));
#37144=CARTESIAN_POINT('Ctrl Pts',(-33.8345626238842,-32.304678935018,54.));
#37145=CARTESIAN_POINT('Ctrl Pts',(-33.836610926341,-32.2971901668236,54.));
#37146=CARTESIAN_POINT('Ctrl Pts',(-33.8386071814357,-32.2896882893515,
54.));
#37147=CARTESIAN_POINT('Ctrl Pts',(-33.8559453184839,-32.2245319974152,
54.));
#37148=CARTESIAN_POINT('Ctrl Pts',(-33.8693611558278,-32.1583888617247,
54.));
#37149=CARTESIAN_POINT('Ctrl Pts',(-33.8790087385963,-32.091563338769,54.));
#37150=CARTESIAN_POINT('Ctrl Pts',(-33.8893872049359,-32.0196752340216,
54.));
#37151=CARTESIAN_POINT('Ctrl Pts',(-33.8954054565889,-31.9469966406791,
54.));
#37152=CARTESIAN_POINT('Ctrl Pts',(-33.8971951234157,-31.873884038871,54.));
#37153=CARTESIAN_POINT('Ctrl Pts',(-33.8975151977,-31.8608081616469,54.));
#37154=CARTESIAN_POINT('Ctrl Pts',(-33.8976998585592,-31.8477183678653,
54.));
#37155=CARTESIAN_POINT('Ctrl Pts',(-33.8977496523165,-31.8346166621305,
54.));
#37156=CARTESIAN_POINT('Ctrl Pts',(-33.8977946179896,-31.822785319217,54.));
#37157=CARTESIAN_POINT('Ctrl Pts',(-33.8977295479978,-31.8109528682838,
54.));
#37158=CARTESIAN_POINT('Ctrl Pts',(-33.8975553940223,-31.7991242809208,
54.));
#37159=CARTESIAN_POINT('Ctrl Pts',(-33.8965091698478,-31.7280644385481,
54.));
#37160=CARTESIAN_POINT('Ctrl Pts',(-33.8915303674477,-31.6571067098811,
54.));
#37161=CARTESIAN_POINT('Ctrl Pts',(-33.8827991172353,-31.58658669665,54.));
#37162=CARTESIAN_POINT('Ctrl Pts',(-33.8738836330992,-31.5145786744368,
54.));
#37163=CARTESIAN_POINT('Ctrl Pts',(-33.8610557270815,-31.4430260992478,
54.));
#37164=CARTESIAN_POINT('Ctrl Pts',(-33.8444544762436,-31.3722700783463,
54.));
#37165=CARTESIAN_POINT('Ctrl Pts',(-33.8277523080762,-31.30108393873,54.));
#37166=CARTESIAN_POINT('Ctrl Pts',(-33.8072307013535,-31.230702996705,54.));
#37167=CARTESIAN_POINT('Ctrl Pts',(-33.7829788829121,-31.1614736899745,
54.));
#37168=CARTESIAN_POINT('Ctrl Pts',(-33.7769978633042,-31.1444002551724,
54.));
#37169=CARTESIAN_POINT('Ctrl Pts',(-33.7707897192942,-31.1273969048688,
54.));
#37170=CARTESIAN_POINT('Ctrl Pts',(-33.7643553120831,-31.110468945581,54.));
#37171=CARTESIAN_POINT('Ctrl Pts',(-33.759286336738,-31.0971332325215,54.));
#37172=CARTESIAN_POINT('Ctrl Pts',(-33.7540761635107,-31.0838427060458,
54.));
#37173=CARTESIAN_POINT('Ctrl Pts',(-33.7487336536153,-31.0706201630216,
54.));
#37174=CARTESIAN_POINT('Ctrl Pts',(-33.7205084795823,-31.000763749964,54.));
#37175=CARTESIAN_POINT('Ctrl Pts',(-33.6885470726678,-30.9326782822882,
54.));
#37176=CARTESIAN_POINT('Ctrl Pts',(-33.6530075396668,-30.8667211000107,
54.));
#37177=CARTESIAN_POINT('Ctrl Pts',(-33.6174289999564,-30.8006915258803,
54.));
#37178=CARTESIAN_POINT('Ctrl Pts',(-33.5782643040916,-30.7367937961817,
54.));
#37179=CARTESIAN_POINT('Ctrl Pts',(-33.5356203132441,-30.6753908521558,
54.));
#37180=CARTESIAN_POINT('Ctrl Pts',(-33.4939464409215,-30.6153847786457,
54.));
#37181=CARTESIAN_POINT('Ctrl Pts',(-33.4489494371178,-30.5577602901018,
54.));
#37182=CARTESIAN_POINT('Ctrl Pts',(-33.4006836999752,-30.5028757358465,
54.));
#37183=CARTESIAN_POINT('Ctrl Pts',(-33.3903485119752,-30.4911232542703,
54.));
#37184=CARTESIAN_POINT('Ctrl Pts',(-33.3798632874165,-30.4794965079344,
54.));
#37185=CARTESIAN_POINT('Ctrl Pts',(-33.3692283040305,-30.4679992023154,
54.));
#37186=CARTESIAN_POINT('Ctrl Pts',(-33.3601172578224,-30.4581494001143,
54.));
#37187=CARTESIAN_POINT('Ctrl Pts',(-33.3508962951961,-30.4483946015766,
54.));
#37188=CARTESIAN_POINT('Ctrl Pts',(-33.3415672767799,-30.4387352221184,
54.));
#37189=CARTESIAN_POINT('Ctrl Pts',(-32.3836679988468,-29.9813874990081,
54.));
#37190=CARTESIAN_POINT('Ctrl Pts',(-32.3093502868603,-29.9743669052867,
54.));
#37191=CARTESIAN_POINT('Ctrl Pts',(-32.2347844751733,-29.9717482530017,
54.));
#37192=CARTESIAN_POINT('Ctrl Pts',(-32.1602926808089,-29.9733679476272,
54.));
#37193=CARTESIAN_POINT('Ctrl Pts',(-32.0877589921938,-29.9749450666458,
54.));
#37194=CARTESIAN_POINT('Ctrl Pts',(-32.0152946982106,-29.9805412908907,
54.));
#37195=CARTESIAN_POINT('Ctrl Pts',(-31.9432103771728,-29.9900494467721,
54.));
#37196=CARTESIAN_POINT('Ctrl Pts',(-31.9271201986695,-29.9921717935344,
54.));
#37197=CARTESIAN_POINT('Ctrl Pts',(-31.9110468988445,-29.9944895420622,
54.));
#37198=CARTESIAN_POINT('Ctrl Pts',(-31.895000900343,-29.9970006837775,54.));
#37199=CARTESIAN_POINT('Ctrl Pts',(-31.8213673331251,-30.0085240752489,
54.));
#37200=CARTESIAN_POINT('Ctrl Pts',(-31.7484534163863,-30.0240919768973,
54.));
#37201=CARTESIAN_POINT('Ctrl Pts',(-31.6765910828333,-30.0435648983486,
54.));
#37202=CARTESIAN_POINT('Ctrl Pts',(-31.6261438372765,-30.0572348586962,
54.));
#37203=CARTESIAN_POINT('Ctrl Pts',(-31.5762150877003,-30.072830311071,54.));
#37204=CARTESIAN_POINT('Ctrl Pts',(-31.5269276035993,-30.0903161409675,
54.));
#37205=CARTESIAN_POINT('Ctrl Pts',(-31.5082001964427,-30.0969601046819,
54.));
#37206=CARTESIAN_POINT('Ctrl Pts',(-31.4895654530443,-30.1038770881373,
54.));
#37207=CARTESIAN_POINT('Ctrl Pts',(-31.4710304416861,-30.1110655275264,
54.));
#37208=CARTESIAN_POINT('Ctrl Pts',(-31.4533429018407,-30.1179252917674,
54.));
#37209=CARTESIAN_POINT('Ctrl Pts',(-31.4357407210111,-30.1250347094918,
54.));
#37210=CARTESIAN_POINT('Ctrl Pts',(-31.4182609553468,-30.1323791943156,
54.));
#37211=CARTESIAN_POINT('Ctrl Pts',(-31.3513338021807,-30.160500021,54.));
#37212=CARTESIAN_POINT('Ctrl Pts',(-31.2861267740855,-30.1920888911457,
54.));
#37213=CARTESIAN_POINT('Ctrl Pts',(-31.2229480770285,-30.2270186551939,
54.));
#37214=CARTESIAN_POINT('Ctrl Pts',(-31.1611263845489,-30.2611981687319,
54.));
#37215=CARTESIAN_POINT('Ctrl Pts',(-31.1012461299126,-30.2985772270485,
54.));
#37216=CARTESIAN_POINT('Ctrl Pts',(-31.0436284472419,-30.3390735157394,
54.));
#37217=CARTESIAN_POINT('Ctrl Pts',(-30.9872742147514,-30.3786817950404,
54.));
#37218=CARTESIAN_POINT('Ctrl Pts',(-30.9330838522464,-30.4212726194304,
54.));
#37219=CARTESIAN_POINT('Ctrl Pts',(-30.8813982632594,-30.46679619445,54.));
#37220=CARTESIAN_POINT('Ctrl Pts',(-30.8645714248051,-30.4816169183254,
54.));
#37221=CARTESIAN_POINT('Ctrl Pts',(-30.848010428094,-30.4967486715566,54.));
#37222=CARTESIAN_POINT('Ctrl Pts',(-30.831728140297,-30.512190239164,54.));
#37223=CARTESIAN_POINT('Ctrl Pts',(-30.8225975381376,-30.5208493915078,
54.));
#37224=CARTESIAN_POINT('Ctrl Pts',(-30.8135537587495,-30.5296069313898,
54.));
#37225=CARTESIAN_POINT('Ctrl Pts',(-30.8046115260975,-30.5384500275864,
54.));
#37226=CARTESIAN_POINT('Ctrl Pts',(-30.7560460841086,-30.5864770575297,
54.));
#37227=CARTESIAN_POINT('Ctrl Pts',(-30.7103849485071,-30.6371066388124,
54.));
#37228=CARTESIAN_POINT('Ctrl Pts',(-30.6679204829488,-30.6902577823286,
54.));
#37229=CARTESIAN_POINT('Ctrl Pts',(-30.6618145456302,-30.697900349978,54.));
#37230=CARTESIAN_POINT('Ctrl Pts',(-30.6557747732231,-30.7055951018378,
54.));
#37231=CARTESIAN_POINT('Ctrl Pts',(-30.6498021107534,-30.7133418456573,
54.));
#37232=CARTESIAN_POINT('Ctrl Pts',(-30.6074436402858,-30.7682822044938,
54.));
#37233=CARTESIAN_POINT('Ctrl Pts',(-30.568456554529,-30.8258362406613,54.));
#37234=CARTESIAN_POINT('Ctrl Pts',(-30.5329080920352,-30.8856417419126,
54.));
#37235=CARTESIAN_POINT('Ctrl Pts',(-30.4997462572144,-30.9414320634833,
54.));
#37236=CARTESIAN_POINT('Ctrl Pts',(-30.4695772268648,-30.9991826610177,
54.));
#37237=CARTESIAN_POINT('Ctrl Pts',(-30.4424952980961,-31.058604931198,54.));
#37238=CARTESIAN_POINT('Ctrl Pts',(-30.4366014843027,-31.0715369420091,
54.));
#37239=CARTESIAN_POINT('Ctrl Pts',(-30.4308540294333,-31.0845481194749,
54.));
#37240=CARTESIAN_POINT('Ctrl Pts',(-30.4252541510133,-31.0976354614338,
54.));
#37241=CARTESIAN_POINT('Ctrl Pts',(-30.4207268514394,-31.1082161050176,
54.));
#37242=CARTESIAN_POINT('Ctrl Pts',(-30.4162962339789,-31.1188462321919,
54.));
#37243=CARTESIAN_POINT('Ctrl Pts',(-30.4119679662711,-31.1295112213537,
54.));
#37244=CARTESIAN_POINT('Ctrl Pts',(-30.3862551907436,-31.1928683172718,
54.));
#37245=CARTESIAN_POINT('Ctrl Pts',(-30.3640997107775,-31.2575711336523,
54.));
#37246=CARTESIAN_POINT('Ctrl Pts',(-30.3455477942828,-31.3232696018123,
54.));
#37247=CARTESIAN_POINT('Ctrl Pts',(-30.3270815170559,-31.3886647930192,
54.));
#37248=CARTESIAN_POINT('Ctrl Pts',(-30.3121856030553,-31.4550476008397,
54.));
#37249=CARTESIAN_POINT('Ctrl Pts',(-30.3009567442566,-31.5220754131288,
54.));
#37250=CARTESIAN_POINT('Ctrl Pts',(-30.289968467501,-31.5876671321944,54.));
#37251=CARTESIAN_POINT('Ctrl Pts',(-30.2824919234282,-31.6538774769525,
54.));
#37252=CARTESIAN_POINT('Ctrl Pts',(-30.27866560992,-31.7203725063053,54.));
#37253=CARTESIAN_POINT('Ctrl Pts',(-30.2775523112949,-31.7397198035387,
54.));
#37254=CARTESIAN_POINT('Ctrl Pts',(-30.2767483380266,-31.7590910662344,
54.));
#37255=CARTESIAN_POINT('Ctrl Pts',(-30.2762578628063,-31.7784776822845,
54.));
#37256=CARTESIAN_POINT('Ctrl Pts',(-30.2759857202441,-31.7892344405202,
54.));
#37257=CARTESIAN_POINT('Ctrl Pts',(-30.2758103453474,-31.7999861747191,
54.));
#37258=CARTESIAN_POINT('Ctrl Pts',(-30.2757319690388,-31.8107314277276,
54.));
#37259=CARTESIAN_POINT('Ctrl Pts',(-30.2752558284876,-31.8760094534826,
54.));
#37260=CARTESIAN_POINT('Ctrl Pts',(-30.2783554819153,-31.9410502912499,
54.));
#37261=CARTESIAN_POINT('Ctrl Pts',(-30.2851111645757,-32.005544110067,54.));
#37262=CARTESIAN_POINT('Ctrl Pts',(-30.2920241952358,-32.0715400677344,
54.));
#37263=CARTESIAN_POINT('Ctrl Pts',(-30.3027653449035,-32.1369643722245,
54.));
#37264=CARTESIAN_POINT('Ctrl Pts',(-30.3174745232328,-32.2014643058222,
54.));
#37265=CARTESIAN_POINT('Ctrl Pts',(-30.3311068192429,-32.261242096787,54.));
#37266=CARTESIAN_POINT('Ctrl Pts',(-30.3481479568216,-32.3202263605165,
54.));
#37267=CARTESIAN_POINT('Ctrl Pts',(-30.3687510889275,-32.3781081209656,
54.));
#37268=CARTESIAN_POINT('Ctrl Pts',(-30.3703786319819,-32.3826804867937,
54.));
#37269=CARTESIAN_POINT('Ctrl Pts',(-30.3720284233314,-32.3872459552685,
54.));
#37270=CARTESIAN_POINT('Ctrl Pts',(-30.3737005491397,-32.3918043647069,
54.));
#37271=CARTESIAN_POINT('Ctrl Pts',(-30.377463203204,-32.4020617973208,54.));
#37272=CARTESIAN_POINT('Ctrl Pts',(-30.3813389467107,-32.4122834887951,
54.));
#37273=CARTESIAN_POINT('Ctrl Pts',(-30.3853267233299,-32.4224680762713,
54.));
#37274=CARTESIAN_POINT('Origin',(-32.,-32.,39.4540747194623));
#37275=CARTESIAN_POINT('Ctrl Pts',(-29.9434322372613,-31.9985074052702,
41.2040747194623));
#37276=CARTESIAN_POINT('Ctrl Pts',(-29.9426158455512,-31.9004173014865,
41.2094078928854));
#37277=CARTESIAN_POINT('Ctrl Pts',(-29.9935881722041,-31.121837189222,41.2517843293816));
#37278=CARTESIAN_POINT('Ctrl Pts',(-30.9882785852064,-29.7919911926234,
41.3312040289512));
#37279=CARTESIAN_POINT('Ctrl Pts',(-33.3060692951901,-29.9526095058617,
41.4423338181709));
#37280=CARTESIAN_POINT('Ctrl Pts',(-34.4285436397314,-31.9866292178594,
41.5534636073906));
#37281=CARTESIAN_POINT('Ctrl Pts',(-33.3284492207144,-34.0330616120671,
41.6645933966103));
#37282=CARTESIAN_POINT('Ctrl Pts',(-31.0125684200493,-34.218769212662,41.7757231858301));
#37283=CARTESIAN_POINT('Ctrl Pts',(-29.9981580665322,-32.8935770673079,
41.8555502934473));
#37284=CARTESIAN_POINT('Ctrl Pts',(-29.9427300189926,-32.1072436601885,
41.8983341379914));
#37285=CARTESIAN_POINT('Ctrl Pts',(-29.9436380165453,-32.001608018912,41.9040747194623));
#37286=CARTESIAN_POINT('Ctrl Pts',(-29.9473238289665,-32.0023603893952,
41.1459252805377));
#37287=CARTESIAN_POINT('Ctrl Pts',(-29.950874167023,-31.5322379170384,41.171370046505));
#37288=CARTESIAN_POINT('Ctrl Pts',(-30.3433200420557,-30.3706660396747,
41.2338580755455));
#37289=CARTESIAN_POINT('Ctrl Pts',(-32.2715961806528,-29.5872035622868,
41.3333893676592));
#37290=CARTESIAN_POINT('Ctrl Pts',(-34.1743722595742,-30.9184415569553,
41.444519156879));
#37291=CARTESIAN_POINT('Ctrl Pts',(-34.0880140492357,-33.2405968969734,
41.5556489460986));
#37292=CARTESIAN_POINT('Ctrl Pts',(-32.090310165188,-34.4268231234318,41.6667787353184));
#37293=CARTESIAN_POINT('Ctrl Pts',(-30.279165136739,-33.5261027188181,41.7635375134647));
#37294=CARTESIAN_POINT('Ctrl Pts',(-29.95009226531,-32.4182605833851,41.8232530285378));
#37295=CARTESIAN_POINT('Ctrl Pts',(-29.9479126462767,-31.9988339667449,
41.8459252805377));
#37296=CARTESIAN_POINT('Ctrl Pts',(-33.2690708798524,-30.9206413469515,
41.));
#37297=CARTESIAN_POINT('Ctrl Pts',(-33.6279571482407,-31.3426068457263,
41.0370432630732));
#37298=CARTESIAN_POINT('Ctrl Pts',(-33.8852968192855,-32.5656196832009,
41.1111297892197));
#37299=CARTESIAN_POINT('Ctrl Pts',(-32.5453396492552,-33.8933251529091,
41.2222595784395));
#37300=CARTESIAN_POINT('Ctrl Pts',(-30.7061567832839,-33.4837760673271,
41.3333893676592));
#37301=CARTESIAN_POINT('Ctrl Pts',(-30.0511799688433,-31.7184951900074,
41.4445191568789));
#37302=CARTESIAN_POINT('Ctrl Pts',(-31.1796919931641,-30.2097371100672,
41.5556489460986));
#37303=CARTESIAN_POINT('Ctrl Pts',(-33.0589665145573,-30.3399671185134,
41.6667787353183));
#37304=CARTESIAN_POINT('Ctrl Pts',(-33.9690734657708,-31.9891589132273,
41.7779085245381));
#37305=CARTESIAN_POINT('Ctrl Pts',(-33.0771122529311,-33.6484149632334,
41.8890383137578));
#37306=CARTESIAN_POINT('Ctrl Pts',(-31.1993862941002,-33.7989874720987,
42.0001681029776));
#37307=CARTESIAN_POINT('Ctrl Pts',(-30.0543749801228,-32.3031825501919,
42.1112978921972));
#37308=CARTESIAN_POINT('Ctrl Pts',(-30.6899777445458,-30.5298898605771,
42.222427681417));
#37309=CARTESIAN_POINT('Ctrl Pts',(-32.5244990950944,-30.1020353158865,
42.3335574706367));
#37310=CARTESIAN_POINT('Ctrl Pts',(-33.8790043473039,-31.4111727754414,
42.4446872598565));
#37311=CARTESIAN_POINT('Ctrl Pts',(-33.513865306157,-33.25920089568,42.5558170490762));
#37312=CARTESIAN_POINT('Ctrl Pts',(-31.7632530992687,-33.9548208142199,
42.6669468382959));
#37313=CARTESIAN_POINT('Ctrl Pts',(-30.2293091161659,-32.8614105276525,
42.7780766275156));
#37314=CARTESIAN_POINT('Ctrl Pts',(-30.3158822136371,-30.9796463621952,
42.8892064167354));
#37315=CARTESIAN_POINT('Ctrl Pts',(-31.9437416527471,-30.0316989351598,
43.0003362059551));
#37316=CARTESIAN_POINT('Ctrl Pts',(-33.6230881176018,-30.885119219342,43.1114659951748));
#37317=CARTESIAN_POINT('Ctrl Pts',(-33.8170019406859,-32.7588663430016,
43.2225957843946));
#37318=CARTESIAN_POINT('Ctrl Pts',(-32.34801529131,-33.938107199206,43.3337255736143));
#37319=CARTESIAN_POINT('Ctrl Pts',(-30.5605288218555,-33.343613374649,43.444855362834));
#37320=CARTESIAN_POINT('Ctrl Pts',(-30.0904307639918,-31.5194591554142,
43.5559851520537));
#37321=CARTESIAN_POINT('Ctrl Pts',(-31.367949762624,-30.1350907084618,43.6671149412734));
#37322=CARTESIAN_POINT('Ctrl Pts',(-33.2239142841442,-30.4574670197298,
43.7782447304932));
#37323=CARTESIAN_POINT('Ctrl Pts',(-33.9597657256432,-32.1915527871223,
43.8893745197128));
#37324=CARTESIAN_POINT('Ctrl Pts',(-32.9020608277928,-33.7503315207131,
44.0005043089327));
#37325=CARTESIAN_POINT('Ctrl Pts',(-31.0187996427964,-33.7072258282694,
44.1116340981523));
#37326=CARTESIAN_POINT('Ctrl Pts',(-30.0335223840341,-32.1016855718022,
44.2227638873721));
#37327=CARTESIAN_POINT('Ctrl Pts',(-30.847944113844,-30.4030837827984,44.3338936765918));
#37328=CARTESIAN_POINT('Ctrl Pts',(-32.7167148971371,-30.1659623979207,
44.4450234658116));
#37329=CARTESIAN_POINT('Ctrl Pts',(-33.9295559790202,-31.6073323371673,
44.5561532550312));
#37330=CARTESIAN_POINT('Ctrl Pts',(-33.376488354067,-33.4080674631294,44.667283044251));
#37331=CARTESIAN_POINT('Ctrl Pts',(-31.5636735148665,-33.920154516694,44.7784128334707));
#37332=CARTESIAN_POINT('Ctrl Pts',(-30.1501799430964,-32.6749369797875,
44.8895426226904));
#37333=CARTESIAN_POINT('Ctrl Pts',(-30.4296216269414,-30.812024438367,45.0006724119102));
#37334=CARTESIAN_POINT('Ctrl Pts',(-32.1462565677652,-30.0363342478941,
45.1118022011299));
#37335=CARTESIAN_POINT('Ctrl Pts',(-33.7290390838569,-31.0577696586804,
45.2229319903496));
#37336=CARTESIAN_POINT('Ctrl Pts',(-33.7294237810507,-32.9415240597797,
45.3340617795693));
#37337=CARTESIAN_POINT('Ctrl Pts',(-32.1470585886469,-33.963605851772,45.4451915687891));
#37338=CARTESIAN_POINT('Ctrl Pts',(-30.4301069706974,-33.1886168626412,
45.5563213580088));
#37339=CARTESIAN_POINT('Ctrl Pts',(-30.1499044283847,-31.3258186108344,
45.6674511472285));
#37340=CARTESIAN_POINT('Ctrl Pts',(-31.5628892897633,-30.0800238551992,
45.7785809364483));
#37341=CARTESIAN_POINT('Ctrl Pts',(-33.3759131328822,-30.5913704460114,
45.889710725668));
#37342=CARTESIAN_POINT('Ctrl Pts',(-33.929716197944,-32.3918795286826,46.0008405148877));
#37343=CARTESIAN_POINT('Ctrl Pts',(-32.7174639255481,-33.83374471646,46.1119703041074));
#37344=CARTESIAN_POINT('Ctrl Pts',(-30.8485964490629,-33.5973866258666,
46.2231000933272));
#37345=CARTESIAN_POINT('Ctrl Pts',(-30.0334810159438,-31.8991176182166,
46.3342298825469));
#37346=CARTESIAN_POINT('Ctrl Pts',(-31.0181024310225,-30.293175072351,46.4453596717666));
#37347=CARTESIAN_POINT('Ctrl Pts',(-32.9013458529938,-30.2493001905241,
46.5564894609864));
#37348=CARTESIAN_POINT('Ctrl Pts',(-33.9596873249938,-31.8076467887807,
46.6676192502061));
#37349=CARTESIAN_POINT('Ctrl Pts',(-33.2245442090837,-33.5420329599615,
46.7787490394258));
#37350=CARTESIAN_POINT('Ctrl Pts',(-31.3687115126491,-33.8651672888366,
46.8898788286455));
#37351=CARTESIAN_POINT('Ctrl Pts',(-30.0906271937995,-32.4813207418654,
47.0010086178652));
#37352=CARTESIAN_POINT('Ctrl Pts',(-30.5599801608987,-30.6569746716451,
47.112138407085));
#37353=CARTESIAN_POINT('Ctrl Pts',(-32.3472236683786,-30.061750817432,47.2232681963047));
#37354=CARTESIAN_POINT('Ctrl Pts',(-33.8166918400422,-31.2403915956679,
47.3343979855244));
#37355=CARTESIAN_POINT('Ctrl Pts',(-33.6235433409019,-33.1142177479385,
47.4455277747442));
#37356=CARTESIAN_POINT('Ctrl Pts',(-31.9445455827624,-33.9683239004841,
47.5566575639638));
#37357=CARTESIAN_POINT('Ctrl Pts',(-30.3162991059008,-33.0210413648905,
47.6677873531837));
#37358=CARTESIAN_POINT('Ctrl Pts',(-30.2289574283427,-31.1393128448816,
47.7789171424033));
#37359=CARTESIAN_POINT('Ctrl Pts',(-31.7624547062086,-30.0452758754736,
47.8900469316231));
#37360=CARTESIAN_POINT('Ctrl Pts',(-33.5133508608809,-30.7401812267317,
48.0011767208428));
#37361=CARTESIAN_POINT('Ctrl Pts',(-33.8792447192816,-32.5880590571192,
48.1123065100625));
#37362=CARTESIAN_POINT('Ctrl Pts',(-32.5252741901563,-33.8977516156662,
48.2234362992822));
#37363=CARTESIAN_POINT('Ctrl Pts',(-30.6905784185613,-33.4706424758147,
48.334566088502));
#37364=CARTESIAN_POINT('Ctrl Pts',(-30.0542510782132,-31.6976172905512,
48.4456958777217));
#37365=CARTESIAN_POINT('Ctrl Pts',(-31.1986520503161,-30.2013294817713,
48.5568256669414));
#37366=CARTESIAN_POINT('Ctrl Pts',(-33.076437975713,-30.3511654255047,48.6679554561611));
#37367=CARTESIAN_POINT('Ctrl Pts',(-33.9690795392212,-32.0099968909499,
48.7790852453809));
#37368=CARTESIAN_POINT('Ctrl Pts',(-33.0596408622125,-33.6596793102095,
48.8902150346006));
#37369=CARTESIAN_POINT('Ctrl Pts',(-31.1804303594337,-33.790441223238,49.0013448238204));
#37370=CARTESIAN_POINT('Ctrl Pts',(-30.0512811038385,-32.2826107452856,
49.11247461304));
#37371=CARTESIAN_POINT('Ctrl Pts',(-30.7055782490339,-30.5161379780338,
49.2236044022598));
#37372=CARTESIAN_POINT('Ctrl Pts',(-32.5445161432941,-30.1076796414719,
49.3347341914795));
#37373=CARTESIAN_POINT('Ctrl Pts',(-33.8851187682433,-31.4310523756752,
49.4458639806993));
#37374=CARTESIAN_POINT('Ctrl Pts',(-33.5004811397579,-33.2751198056805,
49.5569937699189));
#37375=CARTESIAN_POINT('Ctrl Pts',(-31.7426194442066,-33.9522114176255,
49.6681235591387));
#37376=CARTESIAN_POINT('Ctrl Pts',(-30.2203096421414,-32.8426603110109,
49.7792533483584));
#37377=CARTESIAN_POINT('Ctrl Pts',(-30.3267531556502,-30.9619156260297,
49.8903831375781));
#37378=CARTESIAN_POINT('Ctrl Pts',(-31.9645340355014,-30.0312145025498,
50.0015129267979));
#37379=CARTESIAN_POINT('Ctrl Pts',(-33.6347729814496,-30.9023245157467,
50.1126427160176));
#37380=CARTESIAN_POINT('Ctrl Pts',(-33.8088854231495,-32.7780152283373,
50.2237725052373));
#37381=CARTESIAN_POINT('Ctrl Pts',(-32.327525542129,-33.9416748411773,50.3349022944571));
#37382=CARTESIAN_POINT('Ctrl Pts',(-30.546417836818,-33.328334695959,50.4460320836767));
#37383=CARTESIAN_POINT('Ctrl Pts',(-30.0956127638102,-31.4993170421883,
50.5571618728965));
#37384=CARTESIAN_POINT('Ctrl Pts',(-31.3876822371413,-30.1285190017276,
50.6682916621162));
#37385=CARTESIAN_POINT('Ctrl Pts',(-33.2401382867359,-30.470480075517,50.779421451336));
#37386=CARTESIAN_POINT('Ctrl Pts',(-33.9576332250398,-32.2122411972453,
50.8905512405557));
#37387=CARTESIAN_POINT('Ctrl Pts',(-32.8835234654548,-33.7597614769049,
51.0016810297755));
#37388=CARTESIAN_POINT('Ctrl Pts',(-31.0008226116605,-33.6967671367391,
51.1128108189951));
#37389=CARTESIAN_POINT('Ctrl Pts',(-30.0325580681222,-32.0809099136646,
51.2239406082149));
#37390=CARTESIAN_POINT('Ctrl Pts',(-30.8648750444701,-30.3910048151118,
51.3350703974346));
#37391=CARTESIAN_POINT('Ctrl Pts',(-32.7360460704965,-30.1736346607921,
51.4462001866543));
#37392=CARTESIAN_POINT('Ctrl Pts',(-33.9335957143077,-31.6277342591057,
51.557329975874));
#37393=CARTESIAN_POINT('Ctrl Pts',(-33.3615395305129,-33.4225274258428,
51.6684597650937));
#37394=CARTESIAN_POINT('Ctrl Pts',(-31.5434171313856,-33.9154389202823,
51.7795895543135));
#37395=CARTESIAN_POINT('Ctrl Pts',(-30.1431544267094,-32.655361484641,51.8907193435332));
#37396=CARTESIAN_POINT('Ctrl Pts',(-30.4422566450893,-30.7955043299255,
52.001849132753));
#37397=CARTESIAN_POINT('Ctrl Pts',(-32.1669887066119,-30.0379885412045,
52.1129789219726));
#37398=CARTESIAN_POINT('Ctrl Pts',(-33.738894479621,-31.0760843803515,52.2241087111924));
#37399=CARTESIAN_POINT('Ctrl Pts',(-33.7193829519648,-32.9597377397069,
52.3352385004121));
#37400=CARTESIAN_POINT('Ctrl Pts',(-32.126310654911,-33.9650495977709,52.4463682896319));
#37401=CARTESIAN_POINT('Ctrl Pts',(-30.4176404888248,-33.1719692351367,
52.5574980788516));
#37402=CARTESIAN_POINT('Ctrl Pts',(-30.1571280478576,-31.3063156129234,
52.6686278680713));
#37403=CARTESIAN_POINT('Ctrl Pts',(-31.5831931003876,-30.0755138748217,
52.779757657291));
#37404=CARTESIAN_POINT('Ctrl Pts',(-33.3907131932281,-30.6059820456399,
52.8908874465108));
#37405=CARTESIAN_POINT('Ctrl Pts',(-33.9254718382176,-32.4122381981941,
53.0020172357305));
#37406=CARTESIAN_POINT('Ctrl Pts',(-32.6980512536445,-33.8412226437882,
53.1131470249502));
#37407=CARTESIAN_POINT('Ctrl Pts',(-30.8317981301991,-33.5851317365559,
53.2242768141699));
#37408=CARTESIAN_POINT('Ctrl Pts',(-30.0346382286355,-31.87836199572,53.3354066033897));
#37409=CARTESIAN_POINT('Ctrl Pts',(-31.0362203629822,-30.2828812929693,
53.4465363926094));
#37410=CARTESIAN_POINT('Ctrl Pts',(-32.9197159734883,-30.2589538275277,
53.5576661818291));
#37411=CARTESIAN_POINT('Ctrl Pts',(-33.9617492885598,-31.8282846250777,
53.6687959710488));
#37412=CARTESIAN_POINT('Ctrl Pts',(-33.207912453419,-33.5550215357871,53.7799257602685));
#37413=CARTESIAN_POINT('Ctrl Pts',(-31.3495946578974,-33.8581158678563,
53.8910555494883));
#37414=CARTESIAN_POINT('Ctrl Pts',(-30.0845579730524,-32.461689624197,54.002185338708));
#37415=CARTESIAN_POINT('Ctrl Pts',(-30.5764960032975,-30.6406229021335,
54.1133151279277));
#37416=CARTESIAN_POINT('Ctrl Pts',(-31.7668777668624,-30.2598665970073,
54.1874016540742));
#37417=CARTESIAN_POINT('Ctrl Pts',(-32.3110796379505,-30.3633004372052,
54.2244449171475));
#37418=CARTESIAN_POINT('Ctrl Pts',(-33.3677806246589,-30.8366876301903,
40.9251850276175));
#37419=CARTESIAN_POINT('Ctrl Pts',(-33.7545814662436,-31.2914740748731,
40.9622282906908));
#37420=CARTESIAN_POINT('Ctrl Pts',(-34.0319373031784,-32.609614211381,41.0363148168372));
#37421=CARTESIAN_POINT('Ctrl Pts',(-32.5877567738346,-34.0405900895225,
41.147444606057));
#37422=CARTESIAN_POINT('Ctrl Pts',(-30.6055202185583,-33.599185820463,41.2585743952767));
#37423=CARTESIAN_POINT('Ctrl Pts',(-29.8995985788648,-31.6965994327276,
41.3697041844964));
#37424=CARTESIAN_POINT('Ctrl Pts',(-31.1158875238449,-30.0704884709193,
41.4808339737161));
#37425=CARTESIAN_POINT('Ctrl Pts',(-33.1413341081016,-30.2108479142962,
41.5919637629359));
#37426=CARTESIAN_POINT('Ctrl Pts',(-34.1222301904244,-31.988315681438,41.7030935521556));
#37427=CARTESIAN_POINT('Ctrl Pts',(-33.1608912421922,-33.7766305128446,
41.8142233413753));
#37428=CARTESIAN_POINT('Ctrl Pts',(-31.1371136694165,-33.9389147189532,
41.925353130595));
#37429=CARTESIAN_POINT('Ctrl Pts',(-29.903042101676,-32.3267644262197,42.0364829198148));
#37430=CARTESIAN_POINT('Ctrl Pts',(-30.5880827561889,-30.4155430585161,
42.1476127090345));
#37431=CARTESIAN_POINT('Ctrl Pts',(-32.5652952181873,-29.9544095113748,
42.2587424982543));
#37432=CARTESIAN_POINT('Ctrl Pts',(-34.0251553957261,-31.3653731388774,
42.3698722874739));
#37433=CARTESIAN_POINT('Ctrl Pts',(-33.6316154337617,-33.3571429421376,
42.4810020766937));
#37434=CARTESIAN_POINT('Ctrl Pts',(-31.7448386619619,-34.1068689517806,
42.5921318659134));
#37435=CARTESIAN_POINT('Ctrl Pts',(-30.0915828094251,-32.928411996765,42.7032616551332));
#37436=CARTESIAN_POINT('Ctrl Pts',(-30.1848896587255,-30.9002821211595,
42.8143914443528));
#37437=CARTESIAN_POINT('Ctrl Pts',(-31.9393658159135,-29.8786022887098,
42.9255212335726));
#37438=CARTESIAN_POINT('Ctrl Pts',(-33.7493337169851,-30.7984025519789,
43.0366510227924));
#37439=CARTESIAN_POINT('Ctrl Pts',(-33.9583303729471,-32.8178918113572,
43.147780812012));
#37440=CARTESIAN_POINT('Ctrl Pts',(-32.3750843078159,-34.088855333198,43.2589106012318));
#37441=CARTESIAN_POINT('Ctrl Pts',(-30.4485651522869,-33.4481211176251,
43.3700403904515));
#37442=CARTESIAN_POINT('Ctrl Pts',(-29.9419023445243,-31.4820821539471,
43.4811701796712));
#37443=CARTESIAN_POINT('Ctrl Pts',(-31.3187881920398,-29.990035989157,43.5922999688909));
#37444=CARTESIAN_POINT('Ctrl Pts',(-33.3191116987022,-30.3374870885413,
43.7034297581107));
#37445=CARTESIAN_POINT('Ctrl Pts',(-34.1121984839153,-32.2064519759966,
43.8145595473304));
#37446=CARTESIAN_POINT('Ctrl Pts',(-32.9722241224715,-33.8864742535418,
43.9256893365502));
#37447=CARTESIAN_POINT('Ctrl Pts',(-30.9424807874817,-33.840015752387,44.0368191257698));
#37448=CARTESIAN_POINT('Ctrl Pts',(-29.8805675674661,-32.1095947886966,
44.1479489149896));
#37449=CARTESIAN_POINT('Ctrl Pts',(-30.75833592542,-30.278873862943,44.2590787042093));
#37450=CARTESIAN_POINT('Ctrl Pts',(-32.7724617791423,-30.0233089129651,
44.370208493429));
#37451=CARTESIAN_POINT('Ctrl Pts',(-34.0796389895932,-31.576790209531,44.4813382826488));
#37452=CARTESIAN_POINT('Ctrl Pts',(-33.4835531495139,-33.5175885168092,
44.5924680718685));
#37453=CARTESIAN_POINT('Ctrl Pts',(-31.5297355554636,-34.0695062710687,
44.7035978610883));
#37454=CARTESIAN_POINT('Ctrl Pts',(-30.0062988812474,-32.7274343289057,
44.8147276503079));
#37455=CARTESIAN_POINT('Ctrl Pts',(-30.3074758501253,-30.7196223776258,
44.9258574395277));
#37456=CARTESIAN_POINT('Ctrl Pts',(-32.1576325663084,-29.8835981412252,
45.0369872287474));
#37457=CARTESIAN_POINT('Ctrl Pts',(-33.8635256672601,-30.9844819345531,
45.1481170179671));
#37458=CARTESIAN_POINT('Ctrl Pts',(-33.8639402866296,-33.0147568485431,
45.2592468071869));
#37459=CARTESIAN_POINT('Ctrl Pts',(-32.1584969692665,-34.1163372993263,
45.3703765964066));
#37460=CARTESIAN_POINT('Ctrl Pts',(-30.3079989444586,-33.2810688044883,
45.4815063856263));
#37461=CARTESIAN_POINT('Ctrl Pts',(-30.0060019366949,-31.2733800323954,
45.592636174846));
#37462=CARTESIAN_POINT('Ctrl Pts',(-31.5288903324594,-29.9306859747887,
45.7037659640658));
#37463=CARTESIAN_POINT('Ctrl Pts',(-33.4829331869855,-30.4818056722793,
45.8148957532855));
#37464=CARTESIAN_POINT('Ctrl Pts',(-34.0798116705231,-32.4223603543679,
45.9260255425052));
#37465=CARTESIAN_POINT('Ctrl Pts',(-32.7732690678164,-33.9763754204464,
46.0371553317249));
#37466=CARTESIAN_POINT('Ctrl Pts',(-30.7590389999979,-33.7216331346312,
46.1482851209446));
#37467=CARTESIAN_POINT('Ctrl Pts',(-29.8805229817197,-31.8912708743355,
46.2594149101644));
#37468=CARTESIAN_POINT('Ctrl Pts',(-30.9417293458004,-30.1604163307297,
46.3705446993841));
#37469=CARTESIAN_POINT('Ctrl Pts',(-32.9714535361373,-30.1131288117858,
46.4816744886039));
#37470=CARTESIAN_POINT('Ctrl Pts',(-34.1121139851762,-31.7926853420297,
46.5928042778235));
#37471=CARTESIAN_POINT('Ctrl Pts',(-33.3197906199043,-33.6619739990141,
46.7039340670433));
#37472=CARTESIAN_POINT('Ctrl Pts',(-31.3196091918293,-34.0102420754583,
46.815063856263));
#37473=CARTESIAN_POINT('Ctrl Pts',(-29.942114052861,-32.5187584046106,46.9261936454828));
#37474=CARTESIAN_POINT('Ctrl Pts',(-30.4479738158706,-30.5525126675639,
47.0373234347025));
#37475=CARTESIAN_POINT('Ctrl Pts',(-32.3742311115723,-29.9109916398163,
47.1484532239222));
#37476=CARTESIAN_POINT('Ctrl Pts',(-33.9579961523304,-31.1813084089564,
47.2595830131419));
#37477=CARTESIAN_POINT('Ctrl Pts',(-33.7498243480599,-33.2008828438791,
47.3707128023617));
#37478=CARTESIAN_POINT('Ctrl Pts',(-31.9402322764998,-34.1214223231157,
47.4818425915813));
#37479=CARTESIAN_POINT('Ctrl Pts',(-30.1853389773331,-33.100459098104,47.5929723808012));
#37480=CARTESIAN_POINT('Ctrl Pts',(-30.0912037669319,-31.0723676404894,
47.7041021700208));
#37481=CARTESIAN_POINT('Ctrl Pts',(-31.7439781690014,-29.8932352585449,
47.8152319592406));
#37482=CARTESIAN_POINT('Ctrl Pts',(-33.6310609743597,-30.6421911210678,
47.9263617484603));
#37483=CARTESIAN_POINT('Ctrl Pts',(-34.0254144641037,-32.6337989447653,
48.03749153768));
#37484=CARTESIAN_POINT('Ctrl Pts',(-32.5661306010053,-34.0453608474769,
48.1486213268997));
#37485=CARTESIAN_POINT('Ctrl Pts',(-30.5887301512975,-33.5850306835924,
48.2597511161195));
#37486=CARTESIAN_POINT('Ctrl Pts',(-29.9029085625381,-31.6740976270261,
48.3708809053392));
#37487=CARTESIAN_POINT('Ctrl Pts',(-31.1363223153341,-30.0614268879414,
48.4820106945589));
#37488=CARTESIAN_POINT('Ctrl Pts',(-33.160164518942,-30.2229172380628,48.5931404837787));
#37489=CARTESIAN_POINT('Ctrl Pts',(-34.1222367362744,-32.010774460249,48.7042702729984));
#37490=CARTESIAN_POINT('Ctrl Pts',(-33.1420609072676,-33.7887710132595,
48.8154000622181));
#37491=CARTESIAN_POINT('Ctrl Pts',(-31.1166833210643,-33.9297037333487,
48.9265298514378));
#37492=CARTESIAN_POINT('Ctrl Pts',(-29.8997075802525,-32.3045925234428,
49.0376596406576));
#37493=CARTESIAN_POINT('Ctrl Pts',(-30.6048966852708,-30.4007215392504,
49.1487894298773));
#37494=CARTESIAN_POINT('Ctrl Pts',(-32.5868692146638,-29.9604928588832,
49.259919219097));
#37495=CARTESIAN_POINT('Ctrl Pts',(-34.0317454031282,-31.3867989965323,
49.3710490083168));
#37496=CARTESIAN_POINT('Ctrl Pts',(-33.617190232011,-33.3743000426669,49.4821787975364));
#37497=CARTESIAN_POINT('Ctrl Pts',(-31.7226000982552,-34.1040565934162,
49.5933085867562));
#37498=CARTESIAN_POINT('Ctrl Pts',(-30.0818833462996,-32.9082033674146,
49.7044383759759));
#37499=CARTESIAN_POINT('Ctrl Pts',(-30.1966061547016,-30.8811722686105,
49.8155681651957));
#37500=CARTESIAN_POINT('Ctrl Pts',(-31.9617754533289,-29.8780801763926,
49.9266979544154));
#37501=CARTESIAN_POINT('Ctrl Pts',(-33.7619274425416,-30.8169460954779,
50.0378277436351));
#37502=CARTESIAN_POINT('Ctrl Pts',(-33.9495825436476,-32.8385301182965,
50.1489575328548));
#37503=CARTESIAN_POINT('Ctrl Pts',(-32.3530008431499,-34.0927004703305,
50.2600873220746));
#37504=CARTESIAN_POINT('Ctrl Pts',(-30.4333565991355,-33.4316540463099,
50.3712171112942));
#37505=CARTESIAN_POINT('Ctrl Pts',(-29.9474874060534,-31.4603733647475,
50.4823469005141));
#37506=CARTESIAN_POINT('Ctrl Pts',(-31.3400554803763,-29.9829531277623,
50.5934766897337));
#37507=CARTESIAN_POINT('Ctrl Pts',(-33.3365976222639,-30.351512314284,50.7046064789536));
#37508=CARTESIAN_POINT('Ctrl Pts',(-34.1099001150427,-32.2287495536736,
50.8157362681731));
#37509=CARTESIAN_POINT('Ctrl Pts',(-32.9522449034691,-33.8966376822164,
50.926866057393));
#37510=CARTESIAN_POINT('Ctrl Pts',(-30.9231054828656,-33.8287435721946,
51.0379958466126));
#37511=CARTESIAN_POINT('Ctrl Pts',(-29.8795282459899,-32.0872031767573,
51.1491256358324));
#37512=CARTESIAN_POINT('Ctrl Pts',(-30.776583762665,-30.2658553797126,51.2602554250521));
#37513=CARTESIAN_POINT('Ctrl Pts',(-32.7932965526705,-30.0315779329776,
51.3713852142718));
#37514=CARTESIAN_POINT('Ctrl Pts',(-34.0839929399853,-31.5987790156538,
51.4825150034916));
#37515=CARTESIAN_POINT('Ctrl Pts',(-33.4674415898341,-33.5331731915083,
51.5936447927112));
#37516=CARTESIAN_POINT('Ctrl Pts',(-31.5079036079414,-34.0644238903223,
51.7047745819311));
#37517=CARTESIAN_POINT('Ctrl Pts',(-29.9987269123803,-32.70633622997,51.8159043711507));
#37518=CARTESIAN_POINT('Ctrl Pts',(-30.3210936340406,-30.7018173167719,
51.9270341603705));
#37519=CARTESIAN_POINT('Ctrl Pts',(-32.1799772739779,-29.8853811073095,
52.0381639495902));
#37520=CARTESIAN_POINT('Ctrl Pts',(-33.8741476266704,-31.0042211956499,
52.1492937388099));
#37521=CARTESIAN_POINT('Ctrl Pts',(-33.8531184706876,-33.0343872087567,
52.2604235280296));
#37522=CARTESIAN_POINT('Ctrl Pts',(-32.1361352381636,-34.1178933414951,
52.3715533172494));
#37523=CARTESIAN_POINT('Ctrl Pts',(-30.2945628057577,-33.2631263059969,
52.4826831064691));
#37524=CARTESIAN_POINT('Ctrl Pts',(-30.0137874173263,-31.2523600696109,
52.5938128956888));
#37525=CARTESIAN_POINT('Ctrl Pts',(-31.5507733960611,-29.9258252031204,
52.7049426849085));
#37526=CARTESIAN_POINT('Ctrl Pts',(-33.4988844124893,-30.4975537783814,
52.8160724741283));
#37527=CARTESIAN_POINT('Ctrl Pts',(-34.0752371797756,-32.444302543842,52.927202263348));
#37528=CARTESIAN_POINT('Ctrl Pts',(-32.7523464566965,-33.9844349892809,
53.0383320525677));
#37529=CARTESIAN_POINT('Ctrl Pts',(-30.7409340892057,-33.708425046397,53.1494618417874));
#37530=CARTESIAN_POINT('Ctrl Pts',(-29.881770203702,-31.8689008564315,53.2605916310072));
#37531=CARTESIAN_POINT('Ctrl Pts',(-30.9612565106631,-30.1493218897363,
53.3717214202269));
#37532=CARTESIAN_POINT('Ctrl Pts',(-32.9912525050397,-30.1235333194147,
53.4828512094466));
#37533=CARTESIAN_POINT('Ctrl Pts',(-34.1143363305622,-31.8149284121924,
53.5939809986663));
#37534=CARTESIAN_POINT('Ctrl Pts',(-33.301865227782,-33.6759728407165,53.7051107878861));
#37535=CARTESIAN_POINT('Ctrl Pts',(-31.2990054068485,-34.0026421871099,
53.8162405771058));
#37536=CARTESIAN_POINT('Ctrl Pts',(-29.9355727613726,-32.4976003567713,
53.9273703663255));
#37537=CARTESIAN_POINT('Ctrl Pts',(-30.4657742788641,-30.5348890392292,
54.0385001555452));
#37538=CARTESIAN_POINT('Ctrl Pts',(-31.7487452602333,-30.1245170851199,
54.1125866816917));
#37539=CARTESIAN_POINT('Ctrl Pts',(-32.3352757582493,-30.2359961244728,
54.149629944765));
#37540=CARTESIAN_POINT('Ctrl Pts',(-33.4664903694653,-30.7527339134291,
40.850370055235));
#37541=CARTESIAN_POINT('Ctrl Pts',(-33.8812057842465,-31.24034130402,40.8874133183083));
#37542=CARTESIAN_POINT('Ctrl Pts',(-34.1785777870715,-32.6536087395612,
40.9614998444547));
#37543=CARTESIAN_POINT('Ctrl Pts',(-32.630173898414,-34.1878550261358,41.0726296336745));
#37544=CARTESIAN_POINT('Ctrl Pts',(-30.5048836538327,-33.7145955735989,
41.1837594228942));
#37545=CARTESIAN_POINT('Ctrl Pts',(-29.7480171888864,-31.6747036754478,
41.2948892121139));
#37546=CARTESIAN_POINT('Ctrl Pts',(-31.0520830545257,-29.9312398317713,
41.4060190013337));
#37547=CARTESIAN_POINT('Ctrl Pts',(-33.2237017016458,-30.0817287100789,
41.5171487905533));
#37548=CARTESIAN_POINT('Ctrl Pts',(-34.2753869150779,-31.9874724496487,
41.6282785797731));
#37549=CARTESIAN_POINT('Ctrl Pts',(-33.2446702314533,-33.9048460624559,
41.7394083689928));
#37550=CARTESIAN_POINT('Ctrl Pts',(-31.0748410447329,-34.0788419658076,
41.8505381582126));
#37551=CARTESIAN_POINT('Ctrl Pts',(-29.7517092232292,-32.3503463022476,
41.9616679474323));
#37552=CARTESIAN_POINT('Ctrl Pts',(-30.486187767832,-30.3011962564552,42.072797736652));
#37553=CARTESIAN_POINT('Ctrl Pts',(-32.6060913412801,-29.8067837068632,
42.1839275258717));
#37554=CARTESIAN_POINT('Ctrl Pts',(-34.1713064441483,-31.3195735023133,
42.2950573150915));
#37555=CARTESIAN_POINT('Ctrl Pts',(-33.7493655613665,-33.4550849885953,
42.4061871043112));
#37556=CARTESIAN_POINT('Ctrl Pts',(-31.7264242246551,-34.2589170893411,
42.5173168935309));
#37557=CARTESIAN_POINT('Ctrl Pts',(-29.9538565026843,-32.9954134658777,
42.6284466827507));
#37558=CARTESIAN_POINT('Ctrl Pts',(-30.0538971038138,-30.8209178801238,
42.7395764719703));
#37559=CARTESIAN_POINT('Ctrl Pts',(-31.9349899790798,-29.7255056422599,
42.8507062611902));
#37560=CARTESIAN_POINT('Ctrl Pts',(-33.8755793163684,-30.7116858846159,
42.9618360504098));
#37561=CARTESIAN_POINT('Ctrl Pts',(-34.0996588052083,-32.8769172797129,
43.0729658396296));
#37562=CARTESIAN_POINT('Ctrl Pts',(-32.4021533243219,-34.2396034671898,
43.1840956288493));
#37563=CARTESIAN_POINT('Ctrl Pts',(-30.3366014827183,-33.5526288606013,
43.295225418069));
#37564=CARTESIAN_POINT('Ctrl Pts',(-29.7933739250569,-31.44470515248,43.4063552072888));
#37565=CARTESIAN_POINT('Ctrl Pts',(-31.2696266214556,-29.8449812698521,
43.5174849965084));
#37566=CARTESIAN_POINT('Ctrl Pts',(-33.4143091132602,-30.2175071573529,
43.6286147857283));
#37567=CARTESIAN_POINT('Ctrl Pts',(-34.2646312421873,-32.2213511648709,
43.7397445749479));
#37568=CARTESIAN_POINT('Ctrl Pts',(-33.0423874171503,-34.0226169863703,
43.8508743641677));
#37569=CARTESIAN_POINT('Ctrl Pts',(-30.866161932167,-33.9728056765046,43.9620041533873));
#37570=CARTESIAN_POINT('Ctrl Pts',(-29.7276127508981,-32.117504005591,44.0731339426071));
#37571=CARTESIAN_POINT('Ctrl Pts',(-30.668727736996,-30.1546639430877,44.1842637318268));
#37572=CARTESIAN_POINT('Ctrl Pts',(-32.8282086611475,-29.8806554280094,
44.2953935210466));
#37573=CARTESIAN_POINT('Ctrl Pts',(-34.2297220001662,-31.5462480818947,
44.4065233102663));
#37574=CARTESIAN_POINT('Ctrl Pts',(-33.5906179449608,-33.6271095704889,
44.517653099486));
#37575=CARTESIAN_POINT('Ctrl Pts',(-31.4957975960606,-34.2188580254434,
44.6287828887057));
#37576=CARTESIAN_POINT('Ctrl Pts',(-29.8624178193984,-32.7799316780238,
44.7399126779255));
#37577=CARTESIAN_POINT('Ctrl Pts',(-30.1853300733093,-30.6272203168844,
44.8510424671452));
#37578=CARTESIAN_POINT('Ctrl Pts',(-32.1690085648516,-29.7308620345563,
44.9621722563649));
#37579=CARTESIAN_POINT('Ctrl Pts',(-33.9980122506633,-30.9111942104258,
45.0733020455847));
#37580=CARTESIAN_POINT('Ctrl Pts',(-33.9984567922086,-33.0879896373065,
45.1844318348043));
#37581=CARTESIAN_POINT('Ctrl Pts',(-32.169935349886,-34.2690687468806,45.2955616240241));
#37582=CARTESIAN_POINT('Ctrl Pts',(-30.1858909182199,-33.3735207463354,
45.4066914132438));
#37583=CARTESIAN_POINT('Ctrl Pts',(-29.8620994450051,-31.2209414539564,
45.5178212024635));
#37584=CARTESIAN_POINT('Ctrl Pts',(-31.4948913751556,-29.7813480943783,
45.6289509916833));
#37585=CARTESIAN_POINT('Ctrl Pts',(-33.5899532410887,-30.3722408985472,
45.740080780903));
#37586=CARTESIAN_POINT('Ctrl Pts',(-34.2299071431023,-32.4528411800533,
45.8512105701227));
#37587=CARTESIAN_POINT('Ctrl Pts',(-32.8290742100847,-34.1190061244327,
45.9623403593424));
#37588=CARTESIAN_POINT('Ctrl Pts',(-30.669481550933,-33.8458796433958,46.0734701485622));
#37589=CARTESIAN_POINT('Ctrl Pts',(-29.7275649474956,-31.8834241304543,
46.1845999377818));
#37590=CARTESIAN_POINT('Ctrl Pts',(-30.8653562605783,-30.0276575891083,
46.2957297270017));
#37591=CARTESIAN_POINT('Ctrl Pts',(-33.0415612192808,-29.9769574330476,
46.4068595162213));
#37592=CARTESIAN_POINT('Ctrl Pts',(-34.2645406453585,-31.7777238952787,
46.5179893054411));
#37593=CARTESIAN_POINT('Ctrl Pts',(-33.4150370307248,-33.7819150380667,
46.6291190946608));
#37594=CARTESIAN_POINT('Ctrl Pts',(-31.2705068710094,-34.15531686208,46.7402488838806));
#37595=CARTESIAN_POINT('Ctrl Pts',(-29.7936009119226,-32.5561960673557,
46.8513786731002));
#37596=CARTESIAN_POINT('Ctrl Pts',(-30.3359674708425,-30.4480506634827,
46.96250846232));
#37597=CARTESIAN_POINT('Ctrl Pts',(-32.401238554766,-29.7602324622005,47.0736382515397));
#37598=CARTESIAN_POINT('Ctrl Pts',(-34.0993004646186,-31.1222252222449,
47.1847680407595));
#37599=CARTESIAN_POINT('Ctrl Pts',(-33.8761053552179,-33.2875479398197,
47.2958978299791));
#37600=CARTESIAN_POINT('Ctrl Pts',(-31.935918970237,-34.2745207457474,47.4070276191989));
#37601=CARTESIAN_POINT('Ctrl Pts',(-30.0543788487655,-33.1798768313175,
47.5181574084186));
#37602=CARTESIAN_POINT('Ctrl Pts',(-29.9534501055209,-31.0054224360972,
47.6292871976384));
#37603=CARTESIAN_POINT('Ctrl Pts',(-31.7255016317942,-29.7411946416163,
47.740416986858));
#37604=CARTESIAN_POINT('Ctrl Pts',(-33.7487710878386,-30.5442010154039,
47.8515467760779));
#37605=CARTESIAN_POINT('Ctrl Pts',(-34.1715842089258,-32.6795388324115,
47.9626765652975));
#37606=CARTESIAN_POINT('Ctrl Pts',(-32.6069870118542,-34.1929700792877,
48.0738063545173));
#37607=CARTESIAN_POINT('Ctrl Pts',(-30.4868818840338,-33.6994188913702,
48.184936143737));
#37608=CARTESIAN_POINT('Ctrl Pts',(-29.7515660468629,-31.6505779635011,
48.2960659329567));
#37609=CARTESIAN_POINT('Ctrl Pts',(-31.0739925803522,-29.9215242941116,
48.4071957221765));
#37610=CARTESIAN_POINT('Ctrl Pts',(-33.2438910621709,-30.0946690506208,
48.5183255113961));
#37611=CARTESIAN_POINT('Ctrl Pts',(-34.2753939333276,-32.0115520295481,
48.6294553006159));
#37612=CARTESIAN_POINT('Ctrl Pts',(-33.2244809523226,-33.9178627163095,
48.7405850898355));
#37613=CARTESIAN_POINT('Ctrl Pts',(-31.0529362826949,-34.0689662434596,
48.8517148790554));
#37614=CARTESIAN_POINT('Ctrl Pts',(-29.7481340566664,-32.3265743016,48.962844668275));
#37615=CARTESIAN_POINT('Ctrl Pts',(-30.5042151215077,-30.285305100467,49.0739744574949));
#37616=CARTESIAN_POINT('Ctrl Pts',(-32.6292222860334,-29.8133060762947,
49.1851042467144));
#37617=CARTESIAN_POINT('Ctrl Pts',(-34.1783720380131,-31.3425456173894,
49.2962340359344));
#37618=CARTESIAN_POINT('Ctrl Pts',(-33.7338993242641,-33.4734802796533,
49.4073638251538));
#37619=CARTESIAN_POINT('Ctrl Pts',(-31.7025807523039,-34.2559017692069,
49.5184936143738));
#37620=CARTESIAN_POINT('Ctrl Pts',(-29.9434570504577,-32.9737464238182,
49.6296234035934));
#37621=CARTESIAN_POINT('Ctrl Pts',(-30.066459153753,-30.8004289111914,49.7407531928132));
#37622=CARTESIAN_POINT('Ctrl Pts',(-31.9590168711562,-29.7249458502354,
49.8518829820329));
#37623=CARTESIAN_POINT('Ctrl Pts',(-33.8890819036338,-30.7315676752091,
49.9630127712526));
#37624=CARTESIAN_POINT('Ctrl Pts',(-34.0902796641457,-32.8990450082557,
50.0741425604723));
#37625=CARTESIAN_POINT('Ctrl Pts',(-32.3784761441709,-34.2437260994837,
50.1852723496921));
#37626=CARTESIAN_POINT('Ctrl Pts',(-30.320295361453,-33.5349733966608,50.2964021389118));
#37627=CARTESIAN_POINT('Ctrl Pts',(-29.7993620482965,-31.4214296873067,
50.4075319281315));
#37628=CARTESIAN_POINT('Ctrl Pts',(-31.2924287236113,-29.837387253797,50.5186617173512));
#37629=CARTESIAN_POINT('Ctrl Pts',(-33.4330569577918,-30.2325445530509,
50.629791506571));
#37630=CARTESIAN_POINT('Ctrl Pts',(-34.2621670050455,-32.2452579101021,
50.7409212957906));
#37631=CARTESIAN_POINT('Ctrl Pts',(-33.0209663414834,-34.0335138875278,
50.8520510850105));
#37632=CARTESIAN_POINT('Ctrl Pts',(-30.8453883540707,-33.9607200076503,
50.9631808742301));
#37633=CARTESIAN_POINT('Ctrl Pts',(-29.7264984238575,-32.09349643985,51.0743106634499));
#37634=CARTESIAN_POINT('Ctrl Pts',(-30.6882924808598,-30.1407059443134,
51.1854404526696));
#37635=CARTESIAN_POINT('Ctrl Pts',(-32.8505470348444,-29.889521205163,51.2965702418894));
#37636=CARTESIAN_POINT('Ctrl Pts',(-34.234390165663,-31.5698237722019,51.407700031109));
#37637=CARTESIAN_POINT('Ctrl Pts',(-33.5733436491552,-33.6438189571738,
51.5188298203288));
#37638=CARTESIAN_POINT('Ctrl Pts',(-31.4723900844973,-34.2134088603623,
51.6299596095485));
#37639=CARTESIAN_POINT('Ctrl Pts',(-29.8542993980512,-32.757310975299,51.7410893987683));
#37640=CARTESIAN_POINT('Ctrl Pts',(-30.1999306229919,-30.6081303036183,
51.8522191879879));
#37641=CARTESIAN_POINT('Ctrl Pts',(-32.1929658413439,-29.7327736734147,
51.9633489772077));
#37642=CARTESIAN_POINT('Ctrl Pts',(-34.0094007737198,-30.9323580109484,
52.0744787664274));
#37643=CARTESIAN_POINT('Ctrl Pts',(-33.9868539894103,-33.1090366778066,
52.1856085556471));
#37644=CARTESIAN_POINT('Ctrl Pts',(-32.1459598214163,-34.2707370852193,
52.2967383448669));
#37645=CARTESIAN_POINT('Ctrl Pts',(-30.1714851226906,-33.3542833768571,
52.4078681340866));
#37646=CARTESIAN_POINT('Ctrl Pts',(-29.8704467867951,-31.1984045262985,
52.5189979233063));
#37647=CARTESIAN_POINT('Ctrl Pts',(-31.5183536917345,-29.7761365314191,
52.6301277125261));
#37648=CARTESIAN_POINT('Ctrl Pts',(-33.6070556317504,-30.389125511123,52.7412575017458));
#37649=CARTESIAN_POINT('Ctrl Pts',(-34.2250025213337,-32.4763668894899,
52.8523872909655));
#37650=CARTESIAN_POINT('Ctrl Pts',(-32.8066416597486,-34.1276473347736,
52.9635170801852));
#37651=CARTESIAN_POINT('Ctrl Pts',(-30.6500700482123,-33.8317183562382,
53.074646869405));
#37652=CARTESIAN_POINT('Ctrl Pts',(-29.7289021787684,-31.859439717143,53.1857766586246));
#37653=CARTESIAN_POINT('Ctrl Pts',(-30.8862926583441,-30.0157624865034,
53.2969064478444));
#37654=CARTESIAN_POINT('Ctrl Pts',(-33.062789036591,-29.9881128113017,53.4080362370641));
#37655=CARTESIAN_POINT('Ctrl Pts',(-34.2669233725645,-31.801572199307,53.5191660262839));
#37656=CARTESIAN_POINT('Ctrl Pts',(-33.3958180021451,-33.796924145646,53.6302958155035));
#37657=CARTESIAN_POINT('Ctrl Pts',(-31.2484161557996,-34.1471685063634,
53.7414256047234));
#37658=CARTESIAN_POINT('Ctrl Pts',(-29.7865875496927,-32.5335110893457,
53.852555393943));
#37659=CARTESIAN_POINT('Ctrl Pts',(-30.3550525544307,-30.4291551763249,
53.9636851831628));
#37660=CARTESIAN_POINT('Ctrl Pts',(-31.7306127536042,-29.9891675732325,
54.0377717093093));
#37661=CARTESIAN_POINT('Ctrl Pts',(-32.359471878548,-30.1086918117405,54.0748149723825));
#37662=CARTESIAN_POINT('Ctrl Pts',(-33.5652001142718,-30.6687801966679,
40.7755550828525));
#37663=CARTESIAN_POINT('Ctrl Pts',(-34.0078301022494,-31.1892085331669,
40.8125983459258));
#37664=CARTESIAN_POINT('Ctrl Pts',(-34.3252182709644,-32.6976032677414,
40.8866848720723));
#37665=CARTESIAN_POINT('Ctrl Pts',(-32.6725910229935,-34.3351199627491,
40.997814661292));
#37666=CARTESIAN_POINT('Ctrl Pts',(-30.4042470891071,-33.8300053267349,
41.1089444505117));
#37667=CARTESIAN_POINT('Ctrl Pts',(-29.596435798908,-31.652807918168,41.2200742397314));
#37668=CARTESIAN_POINT('Ctrl Pts',(-30.9882785852064,-29.7919911926234,
41.3312040289512));
#37669=CARTESIAN_POINT('Ctrl Pts',(-33.3060692951901,-29.9526095058617,
41.4423338181709));
#37670=CARTESIAN_POINT('Ctrl Pts',(-34.4285436397314,-31.9866292178594,
41.5534636073906));
#37671=CARTESIAN_POINT('Ctrl Pts',(-33.3284492207144,-34.0330616120671,
41.6645933966103));
#37672=CARTESIAN_POINT('Ctrl Pts',(-31.0125684200493,-34.218769212662,41.7757231858301));
#37673=CARTESIAN_POINT('Ctrl Pts',(-29.6003763447824,-32.3739281782754,
41.8868529750497));
#37674=CARTESIAN_POINT('Ctrl Pts',(-30.384292779475,-30.1868494543942,41.9979827642696));
#37675=CARTESIAN_POINT('Ctrl Pts',(-32.646887464373,-29.6591579023516,42.1091125534892));
#37676=CARTESIAN_POINT('Ctrl Pts',(-34.3174574925706,-31.2737738657493,
42.220242342709));
#37677=CARTESIAN_POINT('Ctrl Pts',(-33.8671156889712,-33.553027035053,42.3313721319286));
#37678=CARTESIAN_POINT('Ctrl Pts',(-31.7080097873483,-34.4109652269018,
42.4425019211485));
#37679=CARTESIAN_POINT('Ctrl Pts',(-29.8161301959435,-33.0624149349904,
42.5536317103682));
#37680=CARTESIAN_POINT('Ctrl Pts',(-29.9229045489022,-30.741553639088,42.6647614995879));
#37681=CARTESIAN_POINT('Ctrl Pts',(-31.9306141422462,-29.57240899581,42.7758912888076));
#37682=CARTESIAN_POINT('Ctrl Pts',(-34.0018249157517,-30.6249692172527,
42.8870210780274));
#37683=CARTESIAN_POINT('Ctrl Pts',(-34.2409872374696,-32.9359427480687,
42.9981508672471));
#37684=CARTESIAN_POINT('Ctrl Pts',(-32.4292223408278,-34.3903516011817,
43.1092806564668));
#37685=CARTESIAN_POINT('Ctrl Pts',(-30.2246378131498,-33.6571366035775,
43.2204104456865));
#37686=CARTESIAN_POINT('Ctrl Pts',(-29.6448455055895,-31.4073281510128,
43.3315402349062));
#37687=CARTESIAN_POINT('Ctrl Pts',(-31.2204650508714,-29.6999265505474,
43.442670024126));
#37688=CARTESIAN_POINT('Ctrl Pts',(-33.5095065278182,-30.0975272261643,
43.5537998133457));
#37689=CARTESIAN_POINT('Ctrl Pts',(-34.4170640004594,-32.2362503537452,
43.6649296025654));
#37690=CARTESIAN_POINT('Ctrl Pts',(-33.1125507118291,-34.1587597191989,
43.7760593917852));
#37691=CARTESIAN_POINT('Ctrl Pts',(-30.7898430768523,-34.1055956006222,
43.8871891810049));
#37692=CARTESIAN_POINT('Ctrl Pts',(-29.5746579343302,-32.1254132224854,
43.9983189702246));
#37693=CARTESIAN_POINT('Ctrl Pts',(-30.579119548572,-30.0304540232323,44.1094487594443));
#37694=CARTESIAN_POINT('Ctrl Pts',(-32.8839555431527,-29.7380019430538,
44.2205785486641));
#37695=CARTESIAN_POINT('Ctrl Pts',(-34.3798050107393,-31.5157059542584,
44.3317083378838));
#37696=CARTESIAN_POINT('Ctrl Pts',(-33.6976827404077,-33.7366306241687,
44.4428381271036));
#37697=CARTESIAN_POINT('Ctrl Pts',(-31.4618596366578,-34.3682097798181,
44.5539679163232));
#37698=CARTESIAN_POINT('Ctrl Pts',(-29.7185367575494,-32.832429027142,44.665097705543));
#37699=CARTESIAN_POINT('Ctrl Pts',(-30.0631842964932,-30.5348182561432,
44.7762274947627));
#37700=CARTESIAN_POINT('Ctrl Pts',(-32.1803845633948,-29.5781259278874,
44.8873572839824));
#37701=CARTESIAN_POINT('Ctrl Pts',(-34.1324988340666,-30.8379064862986,
44.9984870732022));
#37702=CARTESIAN_POINT('Ctrl Pts',(-34.1329732977875,-33.1612224260699,
45.1096168624218));
#37703=CARTESIAN_POINT('Ctrl Pts',(-32.1813737305056,-34.4218001944348,
45.2207466516416));
#37704=CARTESIAN_POINT('Ctrl Pts',(-30.0637828919811,-33.4659726881825,
45.3318764408613));
#37705=CARTESIAN_POINT('Ctrl Pts',(-29.7181969533154,-31.1685028755174,
45.4430062300811));
#37706=CARTESIAN_POINT('Ctrl Pts',(-31.4608924178518,-29.6320102139679,
45.5541360193008));
#37707=CARTESIAN_POINT('Ctrl Pts',(-33.6969732951919,-30.2626761248151,
45.6652658085205));
#37708=CARTESIAN_POINT('Ctrl Pts',(-34.3800026156816,-32.4833220057386,
45.7763955977402));
#37709=CARTESIAN_POINT('Ctrl Pts',(-32.8848793523529,-34.2616368284191,
45.88752538696));
#37710=CARTESIAN_POINT('Ctrl Pts',(-30.579924101868,-33.9701261521605,45.9986551761797));
#37711=CARTESIAN_POINT('Ctrl Pts',(-29.5746069132715,-31.8755773865731,
46.1097849653994));
#37712=CARTESIAN_POINT('Ctrl Pts',(-30.7889831753562,-29.8948988474869,
46.2209147546191));
#37713=CARTESIAN_POINT('Ctrl Pts',(-33.1116689024243,-29.8407860543094,
46.3320445438389));
#37714=CARTESIAN_POINT('Ctrl Pts',(-34.4169673055408,-31.7627624485277,
46.4431743330586));
#37715=CARTESIAN_POINT('Ctrl Pts',(-33.5102834415455,-33.9018560771194,
46.5543041222783));
#37716=CARTESIAN_POINT('Ctrl Pts',(-31.2214045501895,-34.3003916487017,
46.665433911498));
#37717=CARTESIAN_POINT('Ctrl Pts',(-29.6450877709841,-32.5936337301009,
46.7765637007178));
#37718=CARTESIAN_POINT('Ctrl Pts',(-30.2239611258143,-30.3435886594015,
46.8876934899375));
#37719=CARTESIAN_POINT('Ctrl Pts',(-32.4282459979597,-29.6094732845848,
46.9988232791572));
#37720=CARTESIAN_POINT('Ctrl Pts',(-34.2406047769068,-31.0631420355334,
47.109953068377));
#37721=CARTESIAN_POINT('Ctrl Pts',(-34.0023863623759,-33.3742130357603,
47.2210828575967));
#37722=CARTESIAN_POINT('Ctrl Pts',(-31.9316056639743,-34.4276191683791,
47.3322126468164));
#37723=CARTESIAN_POINT('Ctrl Pts',(-29.9234187201979,-33.2592945645311,
47.4433424360361));
#37724=CARTESIAN_POINT('Ctrl Pts',(-29.8156964441101,-30.938477231705,47.5544722252559));
#37725=CARTESIAN_POINT('Ctrl Pts',(-31.707025094587,-29.5891540246876,47.6656020144756));
#37726=CARTESIAN_POINT('Ctrl Pts',(-33.8664812013175,-30.44621090974,47.7767318036953));
#37727=CARTESIAN_POINT('Ctrl Pts',(-34.3177539537478,-32.7252787200575,
47.887861592915));
#37728=CARTESIAN_POINT('Ctrl Pts',(-32.6478434227033,-34.3405793110984,
47.9989913821348));
#37729=CARTESIAN_POINT('Ctrl Pts',(-30.38503361677,-33.8138070991479,48.1101211713545));
#37730=CARTESIAN_POINT('Ctrl Pts',(-29.6002235311877,-31.627058299976,48.2212509605742));
#37731=CARTESIAN_POINT('Ctrl Pts',(-31.0116628453703,-29.7816217002818,
48.3323807497939));
#37732=CARTESIAN_POINT('Ctrl Pts',(-33.3276176053999,-29.9664208631788,
48.4435105390137));
#37733=CARTESIAN_POINT('Ctrl Pts',(-34.4285511303809,-32.0123295988471,
48.5546403282334));
#37734=CARTESIAN_POINT('Ctrl Pts',(-33.3069009973776,-34.0469544193595,
48.6657701174531));
#37735=CARTESIAN_POINT('Ctrl Pts',(-30.9891892443255,-34.2082287535704,
48.7768999066729));
#37736=CARTESIAN_POINT('Ctrl Pts',(-29.5965605330805,-32.3485560797573,
48.8880296958926));
#37737=CARTESIAN_POINT('Ctrl Pts',(-30.4035335577445,-30.1698886616836,
48.9991594851123));
#37738=CARTESIAN_POINT('Ctrl Pts',(-32.6715753574031,-29.6661192937061,
49.110289274332));
#37739=CARTESIAN_POINT('Ctrl Pts',(-34.3249986728979,-31.2982922382464,
49.2214190635518));
#37740=CARTESIAN_POINT('Ctrl Pts',(-33.8506084165172,-33.5726605166398,
49.3325488527714));
#37741=CARTESIAN_POINT('Ctrl Pts',(-31.6825614063526,-34.4077469449976,
49.4436786419912));
#37742=CARTESIAN_POINT('Ctrl Pts',(-29.8050307546158,-33.0392894802219,
49.5548084312109));
#37743=CARTESIAN_POINT('Ctrl Pts',(-29.9363121528045,-30.7196855537722,
49.6659382204306));
#37744=CARTESIAN_POINT('Ctrl Pts',(-31.9562582889836,-29.5718115240782,
49.7770680096504));
#37745=CARTESIAN_POINT('Ctrl Pts',(-34.0162363647259,-30.6461892549403,
49.8881977988701));
#37746=CARTESIAN_POINT('Ctrl Pts',(-34.2309767846438,-32.9595598982149,
49.9993275880899));
#37747=CARTESIAN_POINT('Ctrl Pts',(-32.4039514451918,-34.3947517286369,
50.1104573773095));
#37748=CARTESIAN_POINT('Ctrl Pts',(-30.2072341237705,-33.6382927470118,
50.2215871665293));
#37749=CARTESIAN_POINT('Ctrl Pts',(-29.6512366905396,-31.3824860098658,
50.332716955749));
#37750=CARTESIAN_POINT('Ctrl Pts',(-31.2448019668464,-29.6918213798318,
50.4438467449688));
#37751=CARTESIAN_POINT('Ctrl Pts',(-33.5295162933197,-30.1135767918179,
50.5549765341885));
#37752=CARTESIAN_POINT('Ctrl Pts',(-34.4144338950484,-32.2617662665304,
50.6661063234082));
#37753=CARTESIAN_POINT('Ctrl Pts',(-33.0896877794978,-34.1703900928393,
50.7772361126279));
#37754=CARTESIAN_POINT('Ctrl Pts',(-30.7676712252758,-34.0926964431059,
50.8883659018477));
#37755=CARTESIAN_POINT('Ctrl Pts',(-29.5734686017252,-32.0997897029427,
50.9994956910673));
#37756=CARTESIAN_POINT('Ctrl Pts',(-30.6000011990546,-30.0155565089142,
51.1106254802872));
#37757=CARTESIAN_POINT('Ctrl Pts',(-32.9077975170184,-29.7474644773485,
51.2217552695068));
#37758=CARTESIAN_POINT('Ctrl Pts',(-34.3847873913407,-31.54086852875,51.3328850587266));
#37759=CARTESIAN_POINT('Ctrl Pts',(-33.6792457084763,-33.7544647228394,
51.4440148479463));
#37760=CARTESIAN_POINT('Ctrl Pts',(-31.4368765610531,-34.3623938304022,
51.5551446371661));
#37761=CARTESIAN_POINT('Ctrl Pts',(-29.7098718837221,-32.808285720628,51.6662744263857));
#37762=CARTESIAN_POINT('Ctrl Pts',(-30.0787676119431,-30.5144432904648,
51.7774042156055));
#37763=CARTESIAN_POINT('Ctrl Pts',(-32.2059544087099,-29.5801662395198,
51.8885340048252));
#37764=CARTESIAN_POINT('Ctrl Pts',(-34.1446539207691,-30.8604948262468,
51.9996637940449));
#37765=CARTESIAN_POINT('Ctrl Pts',(-34.1205895081331,-33.1836861468564,
52.1107935832646));
#37766=CARTESIAN_POINT('Ctrl Pts',(-32.1557844046688,-34.4235808289435,
52.2219233724844));
#37767=CARTESIAN_POINT('Ctrl Pts',(-30.0484074396236,-33.4454404477173,
52.333053161704));
#37768=CARTESIAN_POINT('Ctrl Pts',(-29.7271061562637,-31.1444489829859,
52.4441829509239));
#37769=CARTESIAN_POINT('Ctrl Pts',(-31.4859339874079,-29.6264478597178,
52.5553127401435));
#37770=CARTESIAN_POINT('Ctrl Pts',(-33.7152268510116,-30.2806972438647,
52.6664425293633));
#37771=CARTESIAN_POINT('Ctrl Pts',(-34.3747678628917,-32.5084312351377,
52.777572318583));
#37772=CARTESIAN_POINT('Ctrl Pts',(-32.8609368628007,-34.2708596802663,
52.8887021078028));
#37773=CARTESIAN_POINT('Ctrl Pts',(-30.5592060072189,-33.9550116660794,
52.9998318970225));
#37774=CARTESIAN_POINT('Ctrl Pts',(-29.5760341538348,-31.8499785778545,
53.1109616862422));
#37775=CARTESIAN_POINT('Ctrl Pts',(-30.811328806025,-29.8822030832705,53.2220914754619));
#37776=CARTESIAN_POINT('Ctrl Pts',(-33.1343255681424,-29.8526923031888,
53.3332212646816));
#37777=CARTESIAN_POINT('Ctrl Pts',(-34.4195104145668,-31.7882159864216,
53.4443510539014));
#37778=CARTESIAN_POINT('Ctrl Pts',(-33.4897707765082,-33.9178754505755,
53.555480843121));
#37779=CARTESIAN_POINT('Ctrl Pts',(-31.1978269047507,-34.2916948256168,
53.6666106323409));
#37780=CARTESIAN_POINT('Ctrl Pts',(-29.6376023380129,-32.5694218219201,
53.7777404215605));
#37781=CARTESIAN_POINT('Ctrl Pts',(-30.2443308299973,-30.3234213134206,
53.8888702107803));
#37782=CARTESIAN_POINT('Ctrl Pts',(-31.7124802469751,-29.853818061345,53.9629567369268));
#37783=CARTESIAN_POINT('Ctrl Pts',(-32.3836679988468,-29.9813874990081,
54.));
#37784=CARTESIAN_POINT('Ctrl Pts',(-33.2690708798524,-30.9206413469515,
41.));
#37785=CARTESIAN_POINT('Ctrl Pts',(-33.3144021339049,-30.9629305958324,
41.));
#37786=CARTESIAN_POINT('Ctrl Pts',(-33.3570035121663,-31.0077888080552,
41.));
#37787=CARTESIAN_POINT('Ctrl Pts',(-33.3968764064509,-31.0548709990206,
41.));
#37788=CARTESIAN_POINT('Ctrl Pts',(-33.4393774015784,-31.1050564697451,
41.));
#37789=CARTESIAN_POINT('Ctrl Pts',(-33.4787791039696,-31.1577689887107,
41.));
#37790=CARTESIAN_POINT('Ctrl Pts',(-33.5150543778823,-31.2126454611912,
41.));
#37791=CARTESIAN_POINT('Ctrl Pts',(-33.5467952425558,-31.2606623746115,
41.));
#37792=CARTESIAN_POINT('Ctrl Pts',(-33.5761421922477,-31.3103372901136,
41.));
#37793=CARTESIAN_POINT('Ctrl Pts',(-33.6030541620467,-31.3614545089767,
41.));
#37794=CARTESIAN_POINT('Ctrl Pts',(-33.6165537378605,-31.3870959160009,
41.));
#37795=CARTESIAN_POINT('Ctrl Pts',(-33.6294402577063,-31.4131005944397,
41.));
#37796=CARTESIAN_POINT('Ctrl Pts',(-33.6417061981854,-31.4394431592821,
41.));
#37797=CARTESIAN_POINT('Ctrl Pts',(-33.6473173626409,-31.4514938017715,
41.));
#37798=CARTESIAN_POINT('Ctrl Pts',(-33.6527992406224,-31.4636168448061,
41.));
#37799=CARTESIAN_POINT('Ctrl Pts',(-33.6581425910225,-31.4757898827236,
41.));
#37800=CARTESIAN_POINT('Ctrl Pts',(-33.6850641954014,-31.5371217599846,
41.));
#37801=CARTESIAN_POINT('Ctrl Pts',(-33.7085245215074,-31.5998290858622,
41.));
#37802=CARTESIAN_POINT('Ctrl Pts',(-33.7284999672539,-31.6635541553473,
41.));
#37803=CARTESIAN_POINT('Ctrl Pts',(-33.7488294277261,-31.7284085920203,
41.));
#37804=CARTESIAN_POINT('Ctrl Pts',(-33.7655499493255,-31.7943180072714,
41.));
#37805=CARTESIAN_POINT('Ctrl Pts',(-33.778597337887,-31.8609418493504,41.));
#37806=CARTESIAN_POINT('Ctrl Pts',(-33.7895089410008,-31.9166597364401,
41.));
#37807=CARTESIAN_POINT('Ctrl Pts',(-33.79785097422,-31.9728782395951,41.));
#37808=CARTESIAN_POINT('Ctrl Pts',(-33.8035610724783,-32.0294104457794,
41.));
#37809=CARTESIAN_POINT('Ctrl Pts',(-33.8061908595079,-32.0554463659775,
41.));
#37810=CARTESIAN_POINT('Ctrl Pts',(-33.8082620610742,-32.0815489376605,
41.));
#37811=CARTESIAN_POINT('Ctrl Pts',(-33.8097667846064,-32.1077003030272,
41.));
#37812=CARTESIAN_POINT('Ctrl Pts',(-33.810424820059,-32.1191366401208,41.));
#37813=CARTESIAN_POINT('Ctrl Pts',(-33.8109744041467,-32.1305821183287,
41.));
#37814=CARTESIAN_POINT('Ctrl Pts',(-33.8114145404549,-32.1420210826457,
41.));
#37815=CARTESIAN_POINT('Ctrl Pts',(-33.8141127124152,-32.2121454786513,
41.));
#37816=CARTESIAN_POINT('Ctrl Pts',(-33.8127099139614,-32.2821564492406,
41.));
#37817=CARTESIAN_POINT('Ctrl Pts',(-33.8071514190027,-32.3516932928698,
41.));
#37818=CARTESIAN_POINT('Ctrl Pts',(-33.8021840417643,-32.4138352461935,
41.));
#37819=CARTESIAN_POINT('Ctrl Pts',(-33.7938974934504,-32.4755995156626,
41.));
#37820=CARTESIAN_POINT('Ctrl Pts',(-33.7822196326176,-32.5367407937649,
41.));
#37821=CARTESIAN_POINT('Ctrl Pts',(-33.7694915938875,-32.6033804435122,
41.));
#37822=CARTESIAN_POINT('Ctrl Pts',(-33.7527359516846,-32.6692808462158,
41.));
#37823=CARTESIAN_POINT('Ctrl Pts',(-33.7321979940556,-32.7342283571542,
41.));
#37824=CARTESIAN_POINT('Ctrl Pts',(-33.724265767216,-32.759312564588,41.));
#37825=CARTESIAN_POINT('Ctrl Pts',(-33.7157687851902,-32.7842545839253,
41.));
#37826=CARTESIAN_POINT('Ctrl Pts',(-33.7067191665299,-32.8090417859885,
41.));
#37827=CARTESIAN_POINT('Ctrl Pts',(-33.70275069803,-32.8199115512552,41.));
#37828=CARTESIAN_POINT('Ctrl Pts',(-33.6986760523364,-32.8307509911782,
41.));
#37829=CARTESIAN_POINT('Ctrl Pts',(-33.6945013450319,-32.8415464817173,
41.));
#37830=CARTESIAN_POINT('Ctrl Pts',(-33.6692787045914,-32.9067704019559,
41.));
#37831=CARTESIAN_POINT('Ctrl Pts',(-33.6403651464208,-32.9705093076493,
41.));
#37832=CARTESIAN_POINT('Ctrl Pts',(-33.6080733761304,-33.032544316927,41.));
#37833=CARTESIAN_POINT('Ctrl Pts',(-33.5750332258155,-33.0960170226008,
41.));
#37834=CARTESIAN_POINT('Ctrl Pts',(-33.5384561627934,-33.1577067585806,
41.));
#37835=CARTESIAN_POINT('Ctrl Pts',(-33.498621001724,-33.217375363133,41.));
#37836=CARTESIAN_POINT('Ctrl Pts',(-33.4681150091642,-33.2630699193408,
41.));
#37837=CARTESIAN_POINT('Ctrl Pts',(-33.4356970622739,-33.3075791992015,
41.));
#37838=CARTESIAN_POINT('Ctrl Pts',(-33.4014728035091,-33.3507901304747,
41.));
#37839=CARTESIAN_POINT('Ctrl Pts',(-33.3801641715878,-33.3776940244585,
41.));
#37840=CARTESIAN_POINT('Ctrl Pts',(-33.3581549933686,-33.4040944868308,
41.));
#37841=CARTESIAN_POINT('Ctrl Pts',(-33.3354678533328,-33.429962533573,41.));
#37842=CARTESIAN_POINT('Ctrl Pts',(-33.3228125188513,-33.444392240596,41.));
#37843=CARTESIAN_POINT('Ctrl Pts',(-33.3099417870806,-33.4586607850949,
41.));
#37844=CARTESIAN_POINT('Ctrl Pts',(-33.296883176771,-33.4727378235807,41.));
#37845=CARTESIAN_POINT('Ctrl Pts',(-33.2460103594919,-33.5275781618508,
41.));
#37846=CARTESIAN_POINT('Ctrl Pts',(-33.1922409760063,-33.5795735763044,
41.));
#37847=CARTESIAN_POINT('Ctrl Pts',(-33.1358600432967,-33.6284600523803,
41.));
#37848=CARTESIAN_POINT('Ctrl Pts',(-33.0937060761678,-33.665010687613,41.));
#37849=CARTESIAN_POINT('Ctrl Pts',(-33.0500910944577,-33.6998232253623,
41.));
#37850=CARTESIAN_POINT('Ctrl Pts',(-33.0051178395859,-33.7327775840894,
41.));
#37851=CARTESIAN_POINT('Ctrl Pts',(-32.9910336310623,-33.7430978524666,
41.));
#37852=CARTESIAN_POINT('Ctrl Pts',(-32.9768161177428,-33.753235803731,41.));
#37853=CARTESIAN_POINT('Ctrl Pts',(-32.9624682127011,-33.7631875218369,
41.));
#37854=CARTESIAN_POINT('Ctrl Pts',(-32.9486861828198,-33.772746748491,41.));
#37855=CARTESIAN_POINT('Ctrl Pts',(-32.9347908997058,-33.7821291855208,
41.));
#37856=CARTESIAN_POINT('Ctrl Pts',(-32.9207902802946,-33.7913286466319,
41.));
#37857=CARTESIAN_POINT('Ctrl Pts',(-32.8578346063116,-33.8326952646019,
41.));
#37858=CARTESIAN_POINT('Ctrl Pts',(-32.7927216231867,-33.8703859566203,
41.));
#37859=CARTESIAN_POINT('Ctrl Pts',(-32.7257126837587,-33.904121456021,41.));
#37860=CARTESIAN_POINT('Ctrl Pts',(-32.6745222121957,-33.9298931834572,
41.));
#37861=CARTESIAN_POINT('Ctrl Pts',(-32.6222242930451,-33.9533562649217,
41.));
#37862=CARTESIAN_POINT('Ctrl Pts',(-32.5689216133098,-33.9743709796003,
41.));
#37863=CARTESIAN_POINT('Ctrl Pts',(-32.5564364973219,-33.9792932677764,
41.));
#37864=CARTESIAN_POINT('Ctrl Pts',(-32.5438962117701,-33.9840811613941,
41.));
#37865=CARTESIAN_POINT('Ctrl Pts',(-32.5313027126548,-33.9887352548077,
41.));
#37866=CARTESIAN_POINT('Ctrl Pts',(-30.3326929969897,-32.0013037885424,
42.1285196366098));
#37867=CARTESIAN_POINT('Ctrl Pts',(-30.3319567887293,-32.0869536137603,
42.1227790551389));
#37868=CARTESIAN_POINT('Ctrl Pts',(-30.3379868491816,-32.1724994374198,
42.1170384736681));
#37869=CARTESIAN_POINT('Ctrl Pts',(-30.3511439931895,-32.2569345889072,
42.1112978921972));
#37870=CARTESIAN_POINT('Ctrl Pts',(-30.4360454181153,-32.8017841908275,
42.074254629124));
#37871=CARTESIAN_POINT('Ctrl Pts',(-30.8177158561077,-33.3003858314631,
42.0372113660508));
#37872=CARTESIAN_POINT('Ctrl Pts',(-31.3215054015757,-33.5245912336367,
42.0001681029776));
#37873=CARTESIAN_POINT('Ctrl Pts',(-31.8252949470438,-33.7487966358103,
41.9631248399043));
#37874=CARTESIAN_POINT('Ctrl Pts',(-32.4512035999874,-33.6986057995218,
41.9260815768311));
#37875=CARTESIAN_POINT('Ctrl Pts',(-32.9128181285992,-33.3969677063766,
41.8890383137578));
#37876=CARTESIAN_POINT('Ctrl Pts',(-33.374432657211,-33.0953296132314,41.8519950506846));
#37877=CARTESIAN_POINT('Ctrl Pts',(-33.6717530614909,-32.5422442632293,
41.8149517876114));
#37878=CARTESIAN_POINT('Ctrl Pts',(-33.6687287717619,-31.9908362891094,
41.7779085245381));
#37879=CARTESIAN_POINT('Ctrl Pts',(-33.665704482033,-31.4394283149894,41.7408652614649));
#37880=CARTESIAN_POINT('Ctrl Pts',(-33.3623354982951,-30.8896977167514,
41.7038219983916));
#37881=CARTESIAN_POINT('Ctrl Pts',(-32.897438586194,-30.5931274162247,41.6667787353184));
#37882=CARTESIAN_POINT('Ctrl Pts',(-32.4325416740929,-30.296557115698,41.6297354722451));
#37883=CARTESIAN_POINT('Ctrl Pts',(-31.8061168336285,-30.2531471128826,
41.5926922091719));
#37884=CARTESIAN_POINT('Ctrl Pts',(-31.3048190760095,-30.482901791465,41.5556489460986));
#37885=CARTESIAN_POINT('Ctrl Pts',(-30.8035213183905,-30.7126564700473,
41.5186056830254));
#37886=CARTESIAN_POINT('Ctrl Pts',(-30.4273506436169,-31.2155758300274,
41.4815624199522));
#37887=CARTESIAN_POINT('Ctrl Pts',(-30.3484281086368,-31.7612489895707,
41.4445191568789));
#37888=CARTESIAN_POINT('Ctrl Pts',(-30.3370655144398,-31.8398103621579,
41.4391859834559));
#37889=CARTESIAN_POINT('Ctrl Pts',(-30.3318642164196,-31.9192579264029,
41.4338528100328));
#37890=CARTESIAN_POINT('Ctrl Pts',(-30.3325261502749,-31.9987897978733,
41.4285196366098));
#37891=CARTESIAN_POINT('Ctrl Pts',(-31.4698297828114,-33.9851743256717,
41.));
#37892=CARTESIAN_POINT('Ctrl Pts',(-30.8097602092473,-33.8088929660699,
41.0370432630732));
#37893=CARTESIAN_POINT('Ctrl Pts',(-29.6907568933951,-32.7487864588875,
41.1111297892197));
#37894=CARTESIAN_POINT('Ctrl Pts',(-30.1186157833437,-30.4619638323954,
41.2222595784395));
#37895=CARTESIAN_POINT('Ctrl Pts',(-32.2715961806528,-29.5872035622868,
41.3333893676592));
#37896=CARTESIAN_POINT('Ctrl Pts',(-34.1743722595742,-30.9184415569553,
41.444519156879));
#37897=CARTESIAN_POINT('Ctrl Pts',(-34.0880140492357,-33.2405968969734,
41.5556489460986));
#37898=CARTESIAN_POINT('Ctrl Pts',(-32.090310165188,-34.4268231234318,41.6667787353184));
#37899=CARTESIAN_POINT('Ctrl Pts',(-30.0101664395875,-33.3923240254871,
41.7779085245381));
#37900=CARTESIAN_POINT('Ctrl Pts',(-29.7509902158367,-31.0834452339837,
41.8890383137579));
#37901=CARTESIAN_POINT('Ctrl Pts',(-31.5501371962138,-29.6134580581644,
42.0001681029775));
#37902=CARTESIAN_POINT('Ctrl Pts',(-33.7609665425501,-30.3275725104634,
42.1112978921973));
#37903=CARTESIAN_POINT('Ctrl Pts',(-34.3601921411462,-32.5722924840244,
42.2224276814169));
#37904=CARTESIAN_POINT('Ctrl Pts',(-32.7993885499411,-34.2932474809962,
42.3335574706367));
#37905=CARTESIAN_POINT('Ctrl Pts',(-30.5069967308568,-33.9154518496341,
42.4446872598564));
#37906=CARTESIAN_POINT('Ctrl Pts',(-29.580983542908,-31.7846531357871,42.5558170490762));
#37907=CARTESIAN_POINT('Ctrl Pts',(-30.8688288772728,-29.8509387094972,
42.6669468382958));
#37908=CARTESIAN_POINT('Ctrl Pts',(-33.1919093046072,-29.8840212783247,
42.7780766275157));
#37909=CARTESIAN_POINT('Ctrl Pts',(-34.4241674901357,-31.8536249255854,
42.8892064167353));
#37910=CARTESIAN_POINT('Ctrl Pts',(-33.4378537625072,-33.9571893024616,
43.0003362059551));
#37911=CARTESIAN_POINT('Ctrl Pts',(-31.1356319224862,-34.2695553308866,
43.1114659951748));
#37912=CARTESIAN_POINT('Ctrl Pts',(-29.6244703439387,-32.5048488942348,
43.2225957843946));
#37913=CARTESIAN_POINT('Ctrl Pts',(-30.2873677599144,-30.2781102439097,
43.3337255736142));
#37914=CARTESIAN_POINT('Ctrl Pts',(-32.5176476217965,-29.6272264154066,
43.444855362834));
#37915=CARTESIAN_POINT('Ctrl Pts',(-34.2741819976516,-31.1478792448328,
43.5559851520537));
#37916=CARTESIAN_POINT('Ctrl Pts',(-33.9494096698203,-33.4483837460143,
43.6671149412734));
#37917=CARTESIAN_POINT('Ctrl Pts',(-31.8405587536029,-34.4233431511784,
43.7782447304932));
#37918=CARTESIAN_POINT('Ctrl Pts',(-29.877626736532,-33.1804851838061,43.8893745197129));
#37919=CARTESIAN_POINT('Ctrl Pts',(-29.8570677142538,-30.8572599783665,
44.0005043089327));
#37920=CARTESIAN_POINT('Ctrl Pts',(-31.7976970806331,-29.5798580480631,
44.1116340981523));
#37921=CARTESIAN_POINT('Ctrl Pts',(-33.923471884996,-30.5173437869082,44.2227638873721));
#37922=CARTESIAN_POINT('Ctrl Pts',(-34.2889060793629,-32.8117404131962,
44.3338936765918));
#37923=CARTESIAN_POINT('Ctrl Pts',(-32.5595582520656,-34.3632410163062,
44.4450234658115));
#37924=CARTESIAN_POINT('Ctrl Pts',(-30.3181087806264,-33.7519290695639,
44.5561532550312));
#37925=CARTESIAN_POINT('Ctrl Pts',(-29.6159079138112,-31.5372706372416,
44.667283044251));
#37926=CARTESIAN_POINT('Ctrl Pts',(-31.0956022698719,-29.7460970996221,
44.7784128334707));
#37927=CARTESIAN_POINT('Ctrl Pts',(-33.4029916207618,-30.0176710538707,
44.8895426226904));
#37928=CARTESIAN_POINT('Ctrl Pts',(-34.4263782551407,-32.1034509621539,
45.0006724119102));
#37929=CARTESIAN_POINT('Ctrl Pts',(-33.2291698233915,-34.0945536717531,
45.1118022011298));
#37930=CARTESIAN_POINT('Ctrl Pts',(-30.907038499066,-34.1687435754524,45.2229319903497));
#37931=CARTESIAN_POINT('Ctrl Pts',(-29.5851736877214,-32.2581228779425,
45.3340617795693));
#37932=CARTESIAN_POINT('Ctrl Pts',(-30.4733317296733,-30.1112709217656,
45.4451915687891));
#37933=CARTESIAN_POINT('Ctrl Pts',(-32.7586800166002,-29.6929633355749,
45.5563213580088));
#37934=CARTESIAN_POINT('Ctrl Pts',(-34.3496925798768,-31.3860306858952,
45.6674511472285));
#37935=CARTESIAN_POINT('Ctrl Pts',(-33.7902919754051,-33.6409960942643,
45.7785809364483));
#37936=CARTESIAN_POINT('Ctrl Pts',(-31.5924355699507,-34.3941396730243,
45.889710725668));
#37937=CARTESIAN_POINT('Ctrl Pts',(-29.7675777110252,-32.9561925863961,
46.0008405148877));
#37938=CARTESIAN_POINT('Ctrl Pts',(-29.9858085213579,-30.643148414175,46.1119703041075));
#37939=CARTESIAN_POINT('Ctrl Pts',(-32.0474055299468,-29.5718800988582,
46.2231000933271));
#37940=CARTESIAN_POINT('Ctrl Pts',(-34.06561751162,-30.7228007852025,46.3342298825469));
#37941=CARTESIAN_POINT('Ctrl Pts',(-34.1933987473477,-33.0426003422808,
46.4453596717667));
#37942=CARTESIAN_POINT('Ctrl Pts',(-32.3138052359217,-34.4082233726336,
46.5564894609863));
#37943=CARTESIAN_POINT('Ctrl Pts',(-30.1470205756562,-33.5698664884471,
46.6676192502061));
#37944=CARTESIAN_POINT('Ctrl Pts',(-29.6760625898251,-31.294784818527,46.7787490394258));
#37945=CARTESIAN_POINT('Ctrl Pts',(-31.3319469197342,-29.6651084349508,
46.8898788286455));
#37946=CARTESIAN_POINT('Ctrl Pts',(-33.5992261839687,-30.172299490863,47.0010086178653));
#37947=CARTESIAN_POINT('Ctrl Pts',(-34.4029109875207,-32.3521822321507,
47.1121384070849));
#37948=CARTESIAN_POINT('Ctrl Pts',(-33.0074777137784,-34.2097516138314,
47.2232681963047));
#37949=CARTESIAN_POINT('Ctrl Pts',(-30.6900117620269,-34.0449802822919,
47.3343979855244));
#37950=CARTESIAN_POINT('Ctrl Pts',(-29.5714328394375,-32.0086651732867,
47.4455277747442));
#37951=CARTESIAN_POINT('Ctrl Pts',(-30.6754522454808,-29.9644197916593,
47.5566575639639));
#37952=CARTESIAN_POINT('Ctrl Pts',(-32.9916833923377,-29.7831153417573,
47.6677873531836));
#37953=CARTESIAN_POINT('Ctrl Pts',(-34.4003366528858,-31.6306796899659,
47.7789171424033));
#37954=CARTESIAN_POINT('Ctrl Pts',(-33.6122278392798,-33.8162419808058,
47.890046931623));
#37955=CARTESIAN_POINT('Ctrl Pts',(-31.3486255910479,-34.3395993071363,
48.0011767208428));
#37956=CARTESIAN_POINT('Ctrl Pts',(-29.6811541380276,-32.7217807194736,
48.1123065100625));
#37957=CARTESIAN_POINT('Ctrl Pts',(-30.1358652710482,-30.4433962447347,
48.2234362992822));
#37958=CARTESIAN_POINT('Ctrl Pts',(-32.2966122923061,-29.5895986461497,
48.334566088502));
#37959=CARTESIAN_POINT('Ctrl Pts',(-34.1859029602719,-30.9417742268944,
48.4456958777216));
#37960=CARTESIAN_POINT('Ctrl Pts',(-34.0746789441273,-33.2624265592047,
48.5568256669415));
#37961=CARTESIAN_POINT('Ctrl Pts',(-32.0647312572736,-34.4277197949768,
48.6679554561611));
#37962=CARTESIAN_POINT('Ctrl Pts',(-29.9955422257445,-33.3711902019111,
48.7790852453809));
#37963=CARTESIAN_POINT('Ctrl Pts',(-29.7608112117745,-31.0597622059948,
48.8902150346006));
#37964=CARTESIAN_POINT('Ctrl Pts',(-31.5753614937973,-29.6088296426979,
49.0013448238204));
#37965=CARTESIAN_POINT('Ctrl Pts',(-33.7785363316839,-30.346270259241,49.11247461304));
#37966=CARTESIAN_POINT('Ctrl Pts',(-34.3540140062368,-32.5971864005746,
49.2236044022598));
#37967=CARTESIAN_POINT('Ctrl Pts',(-32.7751235905007,-34.3015640243191,
49.3347341914795));
#37968=CARTESIAN_POINT('Ctrl Pts',(-30.4868484706035,-33.8995752124292,
49.4458639806993));
#37969=CARTESIAN_POINT('Ctrl Pts',(-29.5833932209651,-31.7591157661596,
49.5569937699189));
#37970=CARTESIAN_POINT('Ctrl Pts',(-30.8915902884901,-29.8391109584199,
49.6681235591387));
#37971=CARTESIAN_POINT('Ctrl Pts',(-33.2141919037862,-29.8967283676685,
49.7792533483584));
#37972=CARTESIAN_POINT('Ctrl Pts',(-34.4255782561001,-31.8792371657958,
49.8903831375781));
#37973=CARTESIAN_POINT('Ctrl Pts',(-33.417101692732,-33.9722668001683,50.0015129267978));
#37974=CARTESIAN_POINT('Ctrl Pts',(-31.1117090280035,-34.2602992473698,
50.1126427160177));
#37975=CARTESIAN_POINT('Ctrl Pts',(-29.6192706277318,-32.4797303353027,
50.2237725052373));
#37976=CARTESIAN_POINT('Ctrl Pts',(-30.3056499310248,-30.2601174228259,
50.3349022944571));
#37977=CARTESIAN_POINT('Ctrl Pts',(-32.5426800429829,-29.6328261767372,
50.4460320836768));
#37978=CARTESIAN_POINT('Ctrl Pts',(-34.2830552647223,-31.1719467427689,
50.5571618728965));
#37979=CARTESIAN_POINT('Ctrl Pts',(-33.9340030668927,-33.4688926699519,
50.6682916621162));
#37980=CARTESIAN_POINT('Ctrl Pts',(-31.8149722356298,-34.4215239550785,
50.7794214513359));
#37981=CARTESIAN_POINT('Ctrl Pts',(-29.8652768077821,-33.1580027768393,
50.8905512405557));
#37982=CARTESIAN_POINT('Ctrl Pts',(-29.8692568953308,-30.8346900152772,
51.0016810297753));
#37983=CARTESIAN_POINT('Ctrl Pts',(-31.8232699653508,-29.5778563144268,
51.1128108189952));
#37984=CARTESIAN_POINT('Ctrl Pts',(-33.9390244464751,-30.5377422476497,
51.2239406082148));
#37985=CARTESIAN_POINT('Ctrl Pts',(-34.2802047821274,-32.8358706181179,
51.3350703974346));
#37986=CARTESIAN_POINT('Ctrl Pts',(-32.5345664287748,-34.3690192638818,
51.4462001866543));
#37987=CARTESIAN_POINT('Ctrl Pts',(-30.2996986773214,-33.7340671695768,
51.557329975874));
#37988=CARTESIAN_POINT('Ctrl Pts',(-29.6209282566264,-31.5121156082528,
51.6684597650938));
#37989=CARTESIAN_POINT('Ctrl Pts',(-31.119458497007,-29.7366705485938,51.7795895543135));
#37990=CARTESIAN_POINT('Ctrl Pts',(-33.4238507688844,-30.0326000635722,
51.8907193435332));
#37991=CARTESIAN_POINT('Ctrl Pts',(-34.4251502639725,-32.1290726539236,
52.001849132753));
#37992=CARTESIAN_POINT('Ctrl Pts',(-33.2069785255006,-34.1074193726832,
52.1129789219726));
#37993=CARTESIAN_POINT('Ctrl Pts',(-30.8841931526569,-34.1570786929198,
52.2241087111924));
#37994=CARTESIAN_POINT('Ctrl Pts',(-29.5825820604857,-32.2326030703908,
52.3352385004121));
#37995=CARTESIAN_POINT('Ctrl Pts',(-30.4933657410223,-30.0952514731161,
52.4463682896319));
#37996=CARTESIAN_POINT('Ctrl Pts',(-32.7830045778855,-29.7011054025381,
52.5574980788515));
#37997=CARTESIAN_POINT('Ctrl Pts',(-34.3560464702414,-31.4108820816923,
52.6686278680714));
#37998=CARTESIAN_POINT('Ctrl Pts',(-33.7728594827364,-33.6598143885419,
52.779757657291));
#37999=CARTESIAN_POINT('Ctrl Pts',(-31.5671721094895,-34.389699997922,52.8908874465108));
#38000=CARTESIAN_POINT('Ctrl Pts',(-29.7576013817629,-32.9325631706899,
53.0020172357305));
#38001=CARTESIAN_POINT('Ctrl Pts',(-30.0002549884253,-30.6219445728053,
53.1131470249502));
#38002=CARTESIAN_POINT('Ctrl Pts',(-32.0730427793273,-29.5725272947448,
53.2242768141699));
#38003=CARTESIAN_POINT('Ctrl Pts',(-34.0790039218848,-30.7446672388737,
53.3354066033898));
#38004=CARTESIAN_POINT('Ctrl Pts',(-34.1822410279863,-33.0657522628949,
53.4465363926093));
#38005=CARTESIAN_POINT('Ctrl Pts',(-32.2883983467057,-34.4113176464284,
53.5576661818292));
#38006=CARTESIAN_POINT('Ctrl Pts',(-30.1304512362118,-33.5503776154227,
53.6687959710488));
#38007=CARTESIAN_POINT('Ctrl Pts',(-29.6838223376843,-31.2699421765937,
53.7799257602686));
#38008=CARTESIAN_POINT('Ctrl Pts',(-31.3562856770569,-29.6588500676751,
53.8910555494883));
#38009=CARTESIAN_POINT('Ctrl Pts',(-33.6191546587482,-30.1879569501259,
54.002185338708));
#38010=CARTESIAN_POINT('Ctrl Pts',(-34.3976272254265,-32.3803532230823,
54.1133151279277));
#38011=CARTESIAN_POINT('Ctrl Pts',(-33.4572031808897,-33.6016627022545,
54.1874016540742));
#38012=CARTESIAN_POINT('Ctrl Pts',(-32.8326019491389,-33.878502477185,54.2244449171475));
#38013=CARTESIAN_POINT('Ctrl Pts',(-31.5032651029123,-33.8599788000028,
40.9251850276175));
#38014=CARTESIAN_POINT('Ctrl Pts',(-30.8848229855226,-33.6948146693493,
40.9622282906908));
#38015=CARTESIAN_POINT('Ctrl Pts',(-29.8363898994693,-32.7015640496904,
41.0363148168372));
#38016=CARTESIAN_POINT('Ctrl Pts',(-30.2372657592897,-30.5589604759703,
41.147444606057));
#38017=CARTESIAN_POINT('Ctrl Pts',(-32.2544678981807,-29.7393671856248,
41.2585743952767));
#38018=CARTESIAN_POINT('Ctrl Pts',(-34.0372449179009,-30.9866503162908,
41.3697041844964));
#38019=CARTESIAN_POINT('Ctrl Pts',(-33.9563329101449,-33.162358336938,41.4808339737161));
#38020=CARTESIAN_POINT('Ctrl Pts',(-32.084614731564,-34.2737749035779,41.5919637629359));
#38021=CARTESIAN_POINT('Ctrl Pts',(-30.1356558010849,-33.3045167553556,
41.7030935521555));
#38022=CARTESIAN_POINT('Ctrl Pts',(-29.8928245920533,-31.1412479943015,
41.8142233413754));
#38023=CARTESIAN_POINT('Ctrl Pts',(-31.5785079087858,-29.763965935017,41.925353130595));
#38024=CARTESIAN_POINT('Ctrl Pts',(-33.6499107379646,-30.4330445770664,
42.0364829198149));
#38025=CARTESIAN_POINT('Ctrl Pts',(-34.2113460212012,-32.5362007124115,
42.1476127090345));
#38026=CARTESIAN_POINT('Ctrl Pts',(-32.7489749069529,-34.1486232431348,
42.2587424982543));
#38027=CARTESIAN_POINT('Ctrl Pts',(-30.6011533631931,-33.7946533897167,
42.3698722874739));
#38028=CARTESIAN_POINT('Ctrl Pts',(-29.7335394333561,-31.7982340407573,
42.4810020766937));
#38029=CARTESIAN_POINT('Ctrl Pts',(-30.9401664729187,-29.9864698084441,
42.5921318659134));
#38030=CARTESIAN_POINT('Ctrl Pts',(-33.1167412400144,-30.0174660166224,
42.7032616551331));
#38031=CARTESIAN_POINT('Ctrl Pts',(-34.2712867484736,-31.8628561070233,
42.8143914443529));
#38032=CARTESIAN_POINT('Ctrl Pts',(-33.3471751478867,-33.8337586594261,
42.9255212335726));
#38033=CARTESIAN_POINT('Ctrl Pts',(-31.1901435159702,-34.1264252445205,
43.0366510227923));
#38034=CARTESIAN_POINT('Ctrl Pts',(-29.7742837281775,-32.4730104698306,
43.147780812012));
#38035=CARTESIAN_POINT('Ctrl Pts',(-30.3953753493751,-30.3867016609807,
43.2589106012318));
#38036=CARTESIAN_POINT('Ctrl Pts',(-32.4850020423711,-29.7768659872946,
43.3700403904515));
#38037=CARTESIAN_POINT('Ctrl Pts',(-34.1307601293648,-31.2016184578062,
43.4811701796712));
#38038=CARTESIAN_POINT('Ctrl Pts',(-33.8264696513034,-33.3570410552955,
43.592299968891));
#38039=CARTESIAN_POINT('Ctrl Pts',(-31.8506139565128,-34.2705143966632,
43.7034297581107));
#38040=CARTESIAN_POINT('Ctrl Pts',(-30.0114747482403,-33.1060375843082,
43.8145595473304));
#38041=CARTESIAN_POINT('Ctrl Pts',(-29.9922122859509,-30.9293271695755,
43.9256893365501));
#38042=CARTESIAN_POINT('Ctrl Pts',(-31.8104553658915,-29.7324849181309,
44.0368191257699));
#38043=CARTESIAN_POINT('Ctrl Pts',(-33.8021676395011,-30.610847879513,44.1479489149896));
#38044=CARTESIAN_POINT('Ctrl Pts',(-34.1445556331039,-32.7605477967984,
44.2590787042093));
#38045=CARTESIAN_POINT('Ctrl Pts',(-32.5242695680424,-34.2142026182709,
44.370208493429));
#38046=CARTESIAN_POINT('Ctrl Pts',(-30.4241776797676,-33.6414432155195,
44.4813382826488));
#38047=CARTESIAN_POINT('Ctrl Pts',(-29.766261289892,-31.56645278264,44.5924680718685));
#38048=CARTESIAN_POINT('Ctrl Pts',(-31.1526383436176,-29.8882400614621,
44.7035978610882));
#38049=CARTESIAN_POINT('Ctrl Pts',(-33.3145115960109,-30.1426871349524,
44.8147276503079));
#38050=CARTESIAN_POINT('Ctrl Pts',(-34.2733580910192,-32.0969268008144,
44.9258574395277));
#38051=CARTESIAN_POINT('Ctrl Pts',(-33.1516519146688,-33.9624601096987,
45.0369872287474));
#38052=CARTESIAN_POINT('Ctrl Pts',(-30.9759663951584,-34.0319712081804,
45.1481170179671));
#38053=CARTESIAN_POINT('Ctrl Pts',(-29.7374653256171,-32.2418442927456,
45.2592468071868));
#38054=CARTESIAN_POINT('Ctrl Pts',(-30.5696114539041,-30.2303841032822,
45.3703765964066));
#38055=CARTESIAN_POINT('Ctrl Pts',(-32.7108336676603,-29.8384571918097,
45.4815063856263));
#38056=CARTESIAN_POINT('Ctrl Pts',(-34.2015086174439,-31.4247508174373,
45.5926361748461));
#38057=CARTESIAN_POINT('Ctrl Pts',(-33.6773867549097,-33.5375062566287,
45.7037659640658));
#38058=CARTESIAN_POINT('Ctrl Pts',(-31.618138724784,-34.2431526433146,45.8148957532855));
#38059=CARTESIAN_POINT('Ctrl Pts',(-29.908365992623,-32.8958900568164,45.9260255425052));
#38060=CARTESIAN_POINT('Ctrl Pts',(-30.1128340211871,-30.728718605843,46.037155331725));
#38061=CARTESIAN_POINT('Ctrl Pts',(-32.044415888098,-29.7250101003294,46.1482851209446));
#38062=CARTESIAN_POINT('Ctrl Pts',(-33.9353488158918,-30.8033476797562,
46.2594149101645));
#38063=CARTESIAN_POINT('Ctrl Pts',(-34.0550714953655,-32.9768484855161,
46.3705446993841));
#38064=CARTESIAN_POINT('Ctrl Pts',(-32.294015028603,-34.2563481508123,46.4816744886038));
#38065=CARTESIAN_POINT('Ctrl Pts',(-30.2638791961233,-33.4708624575619,
46.5928042778236));
#38066=CARTESIAN_POINT('Ctrl Pts',(-29.8226222959054,-31.3392593939899,
46.7039340670433));
#38067=CARTESIAN_POINT('Ctrl Pts',(-31.374077857797,-29.8123589676049,46.815063856263));
#38068=CARTESIAN_POINT('Ctrl Pts',(-33.4983705763898,-30.2875638900887,
46.9261936454827));
#38069=CARTESIAN_POINT('Ctrl Pts',(-34.2513707926229,-32.329971769767,47.0373234347024));
#38070=CARTESIAN_POINT('Ctrl Pts',(-32.9439408745472,-34.0703930641495,
47.1484532239223));
#38071=CARTESIAN_POINT('Ctrl Pts',(-30.7726265046983,-33.9160130787,47.2595830131419));
#38072=CARTESIAN_POINT('Ctrl Pts',(-29.7245910474383,-32.0081187019211,
47.3707128023617));
#38073=CARTESIAN_POINT('Ctrl Pts',(-30.7589851877802,-30.0927941771875,
47.4818425915813));
#38074=CARTESIAN_POINT('Ctrl Pts',(-32.9291426260204,-29.9229237387061,
47.5929723808012));
#38075=CARTESIAN_POINT('Ctrl Pts',(-34.248958809059,-31.6539709696068,47.7041021700208));
#38076=CARTESIAN_POINT('Ctrl Pts',(-33.5105522789894,-33.7017002165947,
47.8152319592406));
#38077=CARTESIAN_POINT('Ctrl Pts',(-31.3897046844462,-34.1920518795256,
47.9263617484603));
#38078=CARTESIAN_POINT('Ctrl Pts',(-29.8273927443206,-32.6762614341274,
48.03749153768));
#38079=CARTESIAN_POINT('Ctrl Pts',(-30.2534274036483,-30.5415638579657,
48.1486213268997));
#38080=CARTESIAN_POINT('Ctrl Pts',(-32.2779063623659,-29.7416112229124,
48.2597511161195));
#38081=CARTESIAN_POINT('Ctrl Pts',(-34.0480484320153,-31.0085115054432,
48.3708809053392));
#38082=CARTESIAN_POINT('Ctrl Pts',(-33.9438387868447,-33.1828113059475,
48.482010694559));
#38083=CARTESIAN_POINT('Ctrl Pts',(-32.0606489640076,-34.274615026303,48.5931404837787));
#38084=CARTESIAN_POINT('Ctrl Pts',(-30.1219538670215,-33.2847157417589,
48.7042702729984));
#38085=CARTESIAN_POINT('Ctrl Pts',(-29.902026224375,-31.1190585425191,48.8154000622181));
#38086=CARTESIAN_POINT('Ctrl Pts',(-31.6021414296023,-29.7596294117535,
48.9265298514378));
#38087=CARTESIAN_POINT('Ctrl Pts',(-33.6663724838611,-30.4505631475438,
49.0376596406575));
#38088=CARTESIAN_POINT('Ctrl Pts',(-34.2055575119472,-32.559524687759,49.1487894298773));
#38089=CARTESIAN_POINT('Ctrl Pts',(-32.7262402233745,-34.1564153015298,
49.259919219097));
#38090=CARTESIAN_POINT('Ctrl Pts',(-30.5822757581167,-33.7797780166906,
49.3710490083167));
#38091=CARTESIAN_POINT('Ctrl Pts',(-29.7357971444513,-31.7743071918651,
49.4821787975364));
#38092=CARTESIAN_POINT('Ctrl Pts',(-30.9614924299265,-29.9753879775081,
49.5933085867562));
#38093=CARTESIAN_POINT('Ctrl Pts',(-33.1376185813874,-30.0293717301325,
49.7044383759759));
#38094=CARTESIAN_POINT('Ctrl Pts',(-34.2726085441223,-31.886853104766,49.8155681651957));
#38095=CARTESIAN_POINT('Ctrl Pts',(-33.3277318126898,-33.8478852908906,
49.9266979544153));
#38096=CARTESIAN_POINT('Ctrl Pts',(-31.1677293249357,-34.1177528982737,
50.0378277436351));
#38097=CARTESIAN_POINT('Ctrl Pts',(-29.7694119334007,-32.4494760192304,
50.1489575328548));
#38098=CARTESIAN_POINT('Ctrl Pts',(-30.412504550697,-30.3698435617522,50.2600873220745));
#38099=CARTESIAN_POINT('Ctrl Pts',(-32.5084557875245,-29.7821125982472,
50.3712171112943));
#38100=CARTESIAN_POINT('Ctrl Pts',(-34.1390738015822,-31.2241681328405,
50.482346900514));
#38101=CARTESIAN_POINT('Ctrl Pts',(-33.8120346697228,-33.3762565787091,
50.5934766897338));
#38102=CARTESIAN_POINT('Ctrl Pts',(-31.8266410588278,-34.2688099286297,
50.7046064789534));
#38103=CARTESIAN_POINT('Ctrl Pts',(-29.9999036709001,-33.0849730360767,
50.8157362681733));
#38104=CARTESIAN_POINT('Ctrl Pts',(-30.0036327532113,-30.9081805869706,
50.9268660573928));
#38105=CARTESIAN_POINT('Ctrl Pts',(-31.8344154901056,-29.7306094243374,
51.0379958466127));
#38106=CARTESIAN_POINT('Ctrl Pts',(-33.8167393747198,-30.6299599061201,
51.1491256358324));
#38107=CARTESIAN_POINT('Ctrl Pts',(-34.1364030854,-32.7831562241863,51.2602554250521));
#38108=CARTESIAN_POINT('Ctrl Pts',(-32.5008538604679,-34.2196164591879,
51.3713852142718));
#38109=CARTESIAN_POINT('Ctrl Pts',(-30.4069286143277,-33.6247077808154,
51.4825150034915));
#38110=CARTESIAN_POINT('Ctrl Pts',(-29.7709650235058,-31.5428841619766,
51.5936447927113));
#38111=CARTESIAN_POINT('Ctrl Pts',(-31.1749900716979,-29.8794079982809,
51.704774581931));
#38112=CARTESIAN_POINT('Ctrl Pts',(-33.3340552566317,-30.1566746428456,
51.8159043711507));
#38113=CARTESIAN_POINT('Ctrl Pts',(-34.2722075434275,-32.1209326540513,
51.9270341603704));
#38114=CARTESIAN_POINT('Ctrl Pts',(-33.130860116645,-33.974514431915,52.0381639495902));
#38115=CARTESIAN_POINT('Ctrl Pts',(-30.9545617963531,-34.0210419744427,
52.1492937388099));
#38116=CARTESIAN_POINT('Ctrl Pts',(-29.7350371400147,-32.2179338983725,
52.2604235280296));
#38117=CARTESIAN_POINT('Ctrl Pts',(-30.5883820152126,-30.2153749252516,
52.3715533172494));
#38118=CARTESIAN_POINT('Ctrl Pts',(-32.7336241942779,-29.8460857772412,
52.482683106469));
#38119=CARTESIAN_POINT('Ctrl Pts',(-34.2074617980904,-31.4480349536138,
52.5938128956888));
#38120=CARTESIAN_POINT('Ctrl Pts',(-33.6610536468417,-33.5551377703734,
52.7049426849085));
#38121=CARTESIAN_POINT('Ctrl Pts',(-31.5944685109066,-34.238992957456,52.8160724741283));
#38122=CARTESIAN_POINT('Ctrl Pts',(-29.8990188231126,-32.8737508362444,
52.9272022633479));
#38123=CARTESIAN_POINT('Ctrl Pts',(-30.1263694181206,-30.7088519901427,
53.0383320525678));
#38124=CARTESIAN_POINT('Ctrl Pts',(-32.068436317801,-29.7256164806422,53.1494618417873));
#38125=CARTESIAN_POINT('Ctrl Pts',(-33.9478910087757,-30.823835119944,53.2605916310073));
#38126=CARTESIAN_POINT('Ctrl Pts',(-34.0446174404242,-32.9985403243459,
53.3717214202267));
#38127=CARTESIAN_POINT('Ctrl Pts',(-32.2702104313418,-34.2592472834404,
53.4828512094467));
#38128=CARTESIAN_POINT('Ctrl Pts',(-30.2483548063011,-33.4526026552904,
53.5939809986663));
#38129=CARTESIAN_POINT('Ctrl Pts',(-29.8298926732848,-31.3159834596125,
53.7051107878861));
#38130=CARTESIAN_POINT('Ctrl Pts',(-31.3968816851753,-29.8064952858593,
53.8162405771058));
#38131=CARTESIAN_POINT('Ctrl Pts',(-33.5170422568196,-30.3022339076858,
53.9273703663255));
#38132=CARTESIAN_POINT('Ctrl Pts',(-34.2464202523342,-32.3563661499634,
54.0385001555453));
#38133=CARTESIAN_POINT('Ctrl Pts',(-33.3653042902589,-33.5006534350279,
54.1125866816917));
#38134=CARTESIAN_POINT('Ctrl Pts',(-32.7800936946509,-33.7600342388745,
54.149629944765));
#38135=CARTESIAN_POINT('Ctrl Pts',(-31.5367004230132,-33.7347832743338,
40.850370055235));
#38136=CARTESIAN_POINT('Ctrl Pts',(-30.9598857617979,-33.5807363726288,
40.8874133183083));
#38137=CARTESIAN_POINT('Ctrl Pts',(-29.9820229055434,-32.6543416404935,
40.9614998444548));
#38138=CARTESIAN_POINT('Ctrl Pts',(-30.3559157352357,-30.6559571195451,
41.0726296336744));
#38139=CARTESIAN_POINT('Ctrl Pts',(-32.2373396157086,-29.8915308089627,
41.1837594228943));
#38140=CARTESIAN_POINT('Ctrl Pts',(-33.9001175762276,-31.0548590756262,
41.2948892121139));
#38141=CARTESIAN_POINT('Ctrl Pts',(-33.8246517710542,-33.0841197769025,
41.4060190013337));
#38142=CARTESIAN_POINT('Ctrl Pts',(-32.0789192979399,-34.1207266837241,
41.5171487905534));
#38143=CARTESIAN_POINT('Ctrl Pts',(-30.2611451625824,-33.2167094852241,
41.6282785797731));
#38144=CARTESIAN_POINT('Ctrl Pts',(-30.03465896827,-31.1990507546193,41.7394083689928));
#38145=CARTESIAN_POINT('Ctrl Pts',(-31.6068786213577,-29.9144738118696,
41.8505381582125));
#38146=CARTESIAN_POINT('Ctrl Pts',(-33.5388549333791,-30.5385166436693,
41.9616679474323));
#38147=CARTESIAN_POINT('Ctrl Pts',(-34.0624999012563,-32.5001089407987,
42.072797736652));
#38148=CARTESIAN_POINT('Ctrl Pts',(-32.6985612639648,-34.0039990052734,
42.1839275258718));
#38149=CARTESIAN_POINT('Ctrl Pts',(-30.6953099955295,-33.6738549297995,
42.2950573150914));
#38150=CARTESIAN_POINT('Ctrl Pts',(-29.8860953238041,-31.8118149457275,
42.4061871043112));
#38151=CARTESIAN_POINT('Ctrl Pts',(-31.0115040685646,-30.1220009073909,
42.5173168935309));
#38152=CARTESIAN_POINT('Ctrl Pts',(-33.0415731754216,-30.15091075492,42.6284466827507));
#38153=CARTESIAN_POINT('Ctrl Pts',(-34.1184060068116,-31.8720872884612,
42.7395764719704));
#38154=CARTESIAN_POINT('Ctrl Pts',(-33.2564965332661,-33.7103280163905,
42.8507062611901));
#38155=CARTESIAN_POINT('Ctrl Pts',(-31.2446551094542,-33.9832951581544,
42.9618360504098));
#38156=CARTESIAN_POINT('Ctrl Pts',(-29.9240971124162,-32.4411720454263,
43.0729658396296));
#38157=CARTESIAN_POINT('Ctrl Pts',(-30.5033829388359,-30.4952930780518,
43.1840956288492));
#38158=CARTESIAN_POINT('Ctrl Pts',(-32.4523564629456,-29.9265055591826,
43.2952254180691));
#38159=CARTESIAN_POINT('Ctrl Pts',(-33.987338261078,-31.2553576707796,43.4063552072887));
#38160=CARTESIAN_POINT('Ctrl Pts',(-33.7035296327865,-33.2656983645767,
43.5174849965085));
#38161=CARTESIAN_POINT('Ctrl Pts',(-31.8606691594226,-34.1176856421479,
43.6286147857282));
#38162=CARTESIAN_POINT('Ctrl Pts',(-30.1453227599487,-33.0315899848104,
43.7397445749479));
#38163=CARTESIAN_POINT('Ctrl Pts',(-30.127356857648,-31.0013943607845,43.8508743641676));
#38164=CARTESIAN_POINT('Ctrl Pts',(-31.8232136511498,-29.8851117881987,
43.9620041533874));
#38165=CARTESIAN_POINT('Ctrl Pts',(-33.6808633940062,-30.7043519721179,
44.0731339426071));
#38166=CARTESIAN_POINT('Ctrl Pts',(-34.0002051868448,-32.7093551804006,
44.1842637318269));
#38167=CARTESIAN_POINT('Ctrl Pts',(-32.4889808840191,-34.0651642202357,
44.2953935210465));
#38168=CARTESIAN_POINT('Ctrl Pts',(-30.5302465789089,-33.5309573614752,
44.4065233102663));
#38169=CARTESIAN_POINT('Ctrl Pts',(-29.9166146659727,-31.5956349280385,
44.517653099486));
#38170=CARTESIAN_POINT('Ctrl Pts',(-31.2096744173634,-30.030383023302,44.6287828887057));
#38171=CARTESIAN_POINT('Ctrl Pts',(-33.2260315712599,-30.2677032160341,
44.7399126779254));
#38172=CARTESIAN_POINT('Ctrl Pts',(-34.1203379268977,-32.0904026394748,
44.8510424671452));
#38173=CARTESIAN_POINT('Ctrl Pts',(-33.0741340059462,-33.8303665476442,
44.9621722563649));
#38174=CARTESIAN_POINT('Ctrl Pts',(-31.044894291251,-33.8951988409082,45.0733020455846));
#38175=CARTESIAN_POINT('Ctrl Pts',(-29.8897569635127,-32.2255657075486,
45.1844318348043));
#38176=CARTESIAN_POINT('Ctrl Pts',(-30.6658911781349,-30.3494972847988,
45.2955616240241));
#38177=CARTESIAN_POINT('Ctrl Pts',(-32.6629873187203,-29.9839510480444,
45.4066914132438));
#38178=CARTESIAN_POINT('Ctrl Pts',(-34.053324655011,-31.4634709489793,45.5178212024635));
#38179=CARTESIAN_POINT('Ctrl Pts',(-33.5644815344143,-33.4340164189931,
45.6289509916833));
#38180=CARTESIAN_POINT('Ctrl Pts',(-31.6438418796174,-34.0921656136048,
45.740080780903));
#38181=CARTESIAN_POINT('Ctrl Pts',(-30.0491542742207,-32.8355875272368,
45.8512105701227));
#38182=CARTESIAN_POINT('Ctrl Pts',(-30.2398595210163,-30.814288797511,45.9623403593425));
#38183=CARTESIAN_POINT('Ctrl Pts',(-32.0414262462491,-29.8781401018006,
46.0734701485621));
#38184=CARTESIAN_POINT('Ctrl Pts',(-33.8050801201637,-30.8838945743099,
46.1845999377819));
#38185=CARTESIAN_POINT('Ctrl Pts',(-33.9167442433832,-32.9110966287515,
46.2957297270016));
#38186=CARTESIAN_POINT('Ctrl Pts',(-32.2742248212842,-34.1044729289912,
46.4068595162214));
#38187=CARTESIAN_POINT('Ctrl Pts',(-30.3807378165902,-33.3718584266768,
46.517989305441));
#38188=CARTESIAN_POINT('Ctrl Pts',(-29.9691820019857,-31.3837339694529,
46.6291190946608));
#38189=CARTESIAN_POINT('Ctrl Pts',(-31.4162087958597,-29.959609500259,46.7402488838805));
#38190=CARTESIAN_POINT('Ctrl Pts',(-33.397514968811,-30.4028282893144,46.8513786731003));
#38191=CARTESIAN_POINT('Ctrl Pts',(-34.0998305977251,-32.3077613073833,
46.96250846232));
#38192=CARTESIAN_POINT('Ctrl Pts',(-32.8804040353159,-33.9310345144675,
47.0736382515397));
#38193=CARTESIAN_POINT('Ctrl Pts',(-30.8552412473697,-33.7870458751082,
47.1847680407594));
#38194=CARTESIAN_POINT('Ctrl Pts',(-29.8777492554391,-32.0075722305555,
47.2958978299792));
#38195=CARTESIAN_POINT('Ctrl Pts',(-30.8425181300796,-30.2211685627158,
47.4070276191989));
#38196=CARTESIAN_POINT('Ctrl Pts',(-32.8666018597031,-30.062732135655,47.5181574084186));
#38197=CARTESIAN_POINT('Ctrl Pts',(-34.0975809652322,-31.6772622492475,
47.6292871976383));
#38198=CARTESIAN_POINT('Ctrl Pts',(-33.408876718699,-33.5871584523836,47.7404169868581));
#38199=CARTESIAN_POINT('Ctrl Pts',(-31.4307837778444,-34.0445044519149,
47.8515467760778));
#38200=CARTESIAN_POINT('Ctrl Pts',(-29.9736313506136,-32.6307421487812,
47.9626765652975));
#38201=CARTESIAN_POINT('Ctrl Pts',(-30.3709895362484,-30.6397314711967,
48.0738063545172));
#38202=CARTESIAN_POINT('Ctrl Pts',(-32.2592004324257,-29.8936237996751,
48.184936143737));
#38203=CARTESIAN_POINT('Ctrl Pts',(-33.9101939037587,-31.075248783992,48.2960659329567));
#38204=CARTESIAN_POINT('Ctrl Pts',(-33.8129986295621,-33.1031960526903,
48.4071957221765));
#38205=CARTESIAN_POINT('Ctrl Pts',(-32.0565666707416,-34.1215102576292,
48.5183255113961));
#38206=CARTESIAN_POINT('Ctrl Pts',(-30.2483655082985,-33.1982412816068,
48.6294553006159));
#38207=CARTESIAN_POINT('Ctrl Pts',(-30.0432412369755,-31.1783548790433,
48.7405850898356));
#38208=CARTESIAN_POINT('Ctrl Pts',(-31.6289213654074,-29.9104291808092,
48.8517148790554));
#38209=CARTESIAN_POINT('Ctrl Pts',(-33.5542086360382,-30.5548560358465,
48.962844668275));
#38210=CARTESIAN_POINT('Ctrl Pts',(-34.0571010176577,-32.5218629749434,
49.0739744574949));
#38211=CARTESIAN_POINT('Ctrl Pts',(-32.6773568562484,-34.0112665787405,
49.1851042467145));
#38212=CARTESIAN_POINT('Ctrl Pts',(-30.6777030456298,-33.659980820952,49.2962340359343));
#38213=CARTESIAN_POINT('Ctrl Pts',(-29.8882010679375,-31.7894986175706,
49.407363825154));
#38214=CARTESIAN_POINT('Ctrl Pts',(-31.0313945713629,-30.1116649965963,
49.5184936143737));
#38215=CARTESIAN_POINT('Ctrl Pts',(-33.0610452589886,-30.1620150925965,
49.6296234035934));
#38216=CARTESIAN_POINT('Ctrl Pts',(-34.1196388321445,-31.8944690437362,
49.7407531928132));
#38217=CARTESIAN_POINT('Ctrl Pts',(-33.2383619326478,-33.7235037816128,
49.8518829820328));
#38218=CARTESIAN_POINT('Ctrl Pts',(-31.2237496218677,-33.9752065491778,
49.9630127712527));
#38219=CARTESIAN_POINT('Ctrl Pts',(-29.9195532390696,-32.4192217031581,
50.0741425604723));
#38220=CARTESIAN_POINT('Ctrl Pts',(-30.5193591703691,-30.4795697006785,
50.1852723496921));
#38221=CARTESIAN_POINT('Ctrl Pts',(-32.4742315320661,-29.9313990197574,
50.2964021389118));
#38222=CARTESIAN_POINT('Ctrl Pts',(-33.9950923384422,-31.276389522912,50.4075319281315));
#38223=CARTESIAN_POINT('Ctrl Pts',(-33.6900662725529,-33.2836204874662,
50.5186617173512));
#38224=CARTESIAN_POINT('Ctrl Pts',(-31.8383098820259,-34.116095902181,50.629791506571));
#38225=CARTESIAN_POINT('Ctrl Pts',(-30.134530534018,-33.011943295314,50.7409212957907));
#38226=CARTESIAN_POINT('Ctrl Pts',(-30.1380086110919,-30.981671158664,50.8520510850104));
#38227=CARTESIAN_POINT('Ctrl Pts',(-31.8455610148604,-29.883362534248,50.9631808742302));
#38228=CARTESIAN_POINT('Ctrl Pts',(-33.6944543029646,-30.7221775645905,
51.0743106634498));
#38229=CARTESIAN_POINT('Ctrl Pts',(-33.9926013886726,-32.7304418302546,
51.1854404526696));
#38230=CARTESIAN_POINT('Ctrl Pts',(-32.4671412921609,-34.0702136544941,
51.2965702418893));
#38231=CARTESIAN_POINT('Ctrl Pts',(-30.5141585513341,-33.5153483920539,
51.407700031109));
#38232=CARTESIAN_POINT('Ctrl Pts',(-29.9210017903852,-31.5736527157003,
51.5188298203288));
#38233=CARTESIAN_POINT('Ctrl Pts',(-31.2305216463888,-30.0221454479681,
51.6299596095485));
#38234=CARTESIAN_POINT('Ctrl Pts',(-33.244259744379,-30.280749222119,51.7410893987682));
#38235=CARTESIAN_POINT('Ctrl Pts',(-34.1192648228826,-32.112792654179,51.852219187988));
#38236=CARTESIAN_POINT('Ctrl Pts',(-33.0547417077894,-33.8416094911468,
51.9633489772076));
#38237=CARTESIAN_POINT('Ctrl Pts',(-31.0249304400494,-33.8850052559656,
52.0744787664275));
#38238=CARTESIAN_POINT('Ctrl Pts',(-29.8874922195436,-32.203264726354,52.1856085556471));
#38239=CARTESIAN_POINT('Ctrl Pts',(-30.683398289403,-30.335498377387,52.2967383448669));
#38240=CARTESIAN_POINT('Ctrl Pts',(-32.6842438106703,-29.9910661519442,
52.4078681340866));
#38241=CARTESIAN_POINT('Ctrl Pts',(-34.0588771259395,-31.4851878255353,
52.5189979233063));
#38242=CARTESIAN_POINT('Ctrl Pts',(-33.549247810947,-33.4504611522048,52.630127712526));
#38243=CARTESIAN_POINT('Ctrl Pts',(-31.6217649123239,-34.0882859169901,
52.7412575017457));
#38244=CARTESIAN_POINT('Ctrl Pts',(-30.0404362644622,-32.8149385017989,
52.8523872909655));
#38245=CARTESIAN_POINT('Ctrl Pts',(-30.2524838478161,-30.79575940748,52.9635170801852));
#38246=CARTESIAN_POINT('Ctrl Pts',(-32.0638298562746,-29.8787056665396,
53.0746468694049));
#38247=CARTESIAN_POINT('Ctrl Pts',(-33.8167780956667,-30.9030030010144,
53.1857766586247));
#38248=CARTESIAN_POINT('Ctrl Pts',(-33.9069938528621,-32.931328385797,53.2969064478444));
#38249=CARTESIAN_POINT('Ctrl Pts',(-32.252022515978,-34.1071769204523,53.4080362370642));
#38250=CARTESIAN_POINT('Ctrl Pts',(-30.3662583763903,-33.3548276951581,
53.5191660262838));
#38251=CARTESIAN_POINT('Ctrl Pts',(-29.9759630088853,-31.3620247426314,
53.6302958155036));
#38252=CARTESIAN_POINT('Ctrl Pts',(-31.4374776932937,-29.9541405040433,
53.7414256047233));
#38253=CARTESIAN_POINT('Ctrl Pts',(-33.414929854891,-30.4165108652457,53.852555393943));
#38254=CARTESIAN_POINT('Ctrl Pts',(-34.0952132792418,-32.3323790768444,
53.9636851831628));
#38255=CARTESIAN_POINT('Ctrl Pts',(-33.2734053996281,-33.3996441678013,
54.0377717093093));
#38256=CARTESIAN_POINT('Ctrl Pts',(-32.7275854401629,-33.6415660005639,
54.0748149723825));
#38257=CARTESIAN_POINT('Ctrl Pts',(-31.5701357431141,-33.6095877486649,
40.7755550828525));
#38258=CARTESIAN_POINT('Ctrl Pts',(-31.0349485380732,-33.4666580759082,
40.8125983459258));
#38259=CARTESIAN_POINT('Ctrl Pts',(-30.1276559116176,-32.6071192312965,
40.8866848720723));
#38260=CARTESIAN_POINT('Ctrl Pts',(-30.4745657111817,-30.75295376312,40.997814661292));
#38261=CARTESIAN_POINT('Ctrl Pts',(-32.2202113332364,-30.0436944323007,
41.1089444505117));
#38262=CARTESIAN_POINT('Ctrl Pts',(-33.7629902345544,-31.1230678349617,
41.2200742397315));
#38263=CARTESIAN_POINT('Ctrl Pts',(-33.6929706319633,-33.0058812168671,
41.3312040289511));
#38264=CARTESIAN_POINT('Ctrl Pts',(-32.073223864316,-33.9676784638702,41.4423338181709));
#38265=CARTESIAN_POINT('Ctrl Pts',(-30.3866345240797,-33.1289022150926,
41.5534636073906));
#38266=CARTESIAN_POINT('Ctrl Pts',(-30.1764933444867,-31.256853514937,41.6645933966103));
#38267=CARTESIAN_POINT('Ctrl Pts',(-31.6352493339297,-30.0649816887222,
41.7757231858301));
#38268=CARTESIAN_POINT('Ctrl Pts',(-33.4277991287936,-30.6439887102723,
41.8868529750498));
#38269=CARTESIAN_POINT('Ctrl Pts',(-33.9136537813114,-32.4640171691859,
41.9979827642695));
#38270=CARTESIAN_POINT('Ctrl Pts',(-32.6481476209767,-33.8593747674119,
42.1091125534893));
#38271=CARTESIAN_POINT('Ctrl Pts',(-30.7894666278659,-33.5530564698822,
42.220242342709));
#38272=CARTESIAN_POINT('Ctrl Pts',(-30.0386512142522,-31.8253958506977,
42.3313721319287));
#38273=CARTESIAN_POINT('Ctrl Pts',(-31.0828416642105,-30.2575320063377,
42.4425019211484));
#38274=CARTESIAN_POINT('Ctrl Pts',(-32.9664051108288,-30.2843554932176,
42.5536317103682));
#38275=CARTESIAN_POINT('Ctrl Pts',(-33.9655252651496,-31.8813184698992,
42.6647614995879));
#38276=CARTESIAN_POINT('Ctrl Pts',(-33.1658179186456,-33.5868973733549,
42.7758912888076));
#38277=CARTESIAN_POINT('Ctrl Pts',(-31.2991667029381,-33.8401650717883,
42.8870210780273));
#38278=CARTESIAN_POINT('Ctrl Pts',(-30.073910496655,-32.4093336210221,42.9981508672471));
#38279=CARTESIAN_POINT('Ctrl Pts',(-30.6113905282966,-30.6038844951228,
43.1092806564668));
#38280=CARTESIAN_POINT('Ctrl Pts',(-32.4197108835201,-30.0761451310706,
43.2204104456865));
#38281=CARTESIAN_POINT('Ctrl Pts',(-33.8439163927912,-31.309096883753,43.3315402349062));
#38282=CARTESIAN_POINT('Ctrl Pts',(-33.5805896142696,-33.174355673858,43.442670024126));
#38283=CARTESIAN_POINT('Ctrl Pts',(-31.8707243623324,-33.9648568876327,
43.5537998133457));
#38284=CARTESIAN_POINT('Ctrl Pts',(-30.279170771657,-32.9571423853126,43.6649296025654));
#38285=CARTESIAN_POINT('Ctrl Pts',(-30.2625014293451,-31.0734615519935,
43.7760593917852));
#38286=CARTESIAN_POINT('Ctrl Pts',(-31.8359719364082,-30.0377386582665,
43.8871891810048));
#38287=CARTESIAN_POINT('Ctrl Pts',(-33.5595591485112,-30.7978560647227,
43.9983189702246));
#38288=CARTESIAN_POINT('Ctrl Pts',(-33.8558547405858,-32.6581625640029,
44.1094487594443));
#38289=CARTESIAN_POINT('Ctrl Pts',(-32.4536921999958,-33.9161258222004,
44.2205785486641));
#38290=CARTESIAN_POINT('Ctrl Pts',(-30.6363154780501,-33.4204715074308,
44.3317083378838));
#38291=CARTESIAN_POINT('Ctrl Pts',(-30.0669680420535,-31.6248170734369,
44.4428381271035));
#38292=CARTESIAN_POINT('Ctrl Pts',(-31.2667104911091,-30.172525985142,44.5539679163232));
#38293=CARTESIAN_POINT('Ctrl Pts',(-33.1375515465089,-30.3927192971158,
44.665097705543));
#38294=CARTESIAN_POINT('Ctrl Pts',(-33.9673177627762,-32.0838784781352,
44.7762274947627));
#38295=CARTESIAN_POINT('Ctrl Pts',(-32.9966160972236,-33.6982729855898,
44.8873572839825));
#38296=CARTESIAN_POINT('Ctrl Pts',(-31.1138221873434,-33.7584264736361,
44.9984870732021));
#38297=CARTESIAN_POINT('Ctrl Pts',(-30.0420486014084,-32.2092871223517,
45.1096168624219));
#38298=CARTESIAN_POINT('Ctrl Pts',(-30.7621709023656,-30.4686104663154,
45.2207466516416));
#38299=CARTESIAN_POINT('Ctrl Pts',(-32.6151409697803,-30.1294449042792,
45.3318764408613));
#38300=CARTESIAN_POINT('Ctrl Pts',(-33.905140692578,-31.5021910805214,45.443006230081));
#38301=CARTESIAN_POINT('Ctrl Pts',(-33.4515763139189,-33.3305265813575,
45.5541360193008));
#38302=CARTESIAN_POINT('Ctrl Pts',(-31.6695450344508,-33.9411785838951,
45.6652658085205));
#38303=CARTESIAN_POINT('Ctrl Pts',(-30.1899425558184,-32.7752849976571,
45.7763955977402));
#38304=CARTESIAN_POINT('Ctrl Pts',(-30.3668850208455,-30.899858989179,45.88752538696));
#38305=CARTESIAN_POINT('Ctrl Pts',(-32.0384366044002,-30.0312701032718,
45.9986551761797));
#38306=CARTESIAN_POINT('Ctrl Pts',(-33.6748114244356,-30.9644414688636,
46.1097849653994));
#38307=CARTESIAN_POINT('Ctrl Pts',(-33.778416991401,-32.8453447719867,46.2209147546191));
#38308=CARTESIAN_POINT('Ctrl Pts',(-32.2544346139655,-33.95259770717,46.3320445438389));
#38309=CARTESIAN_POINT('Ctrl Pts',(-30.4975964370572,-33.2728543957916,
46.4431743330586));
#38310=CARTESIAN_POINT('Ctrl Pts',(-30.115741708066,-31.4282085449159,46.5543041222783));
#38311=CARTESIAN_POINT('Ctrl Pts',(-31.4583397339225,-30.106860032913,46.6654339114981));
#38312=CARTESIAN_POINT('Ctrl Pts',(-33.2966593612321,-30.5180926885401,
46.7765637007177));
#38313=CARTESIAN_POINT('Ctrl Pts',(-33.9482904028273,-32.2855508449996,
46.8876934899375));
#38314=CARTESIAN_POINT('Ctrl Pts',(-32.8168671960847,-33.7916759647855,
46.9988232791572));
#38315=CARTESIAN_POINT('Ctrl Pts',(-30.937855990041,-33.6580786715164,47.1099530683769));
#38316=CARTESIAN_POINT('Ctrl Pts',(-30.0309074634399,-32.0070257591899,
47.2210828575967));
#38317=CARTESIAN_POINT('Ctrl Pts',(-30.926051072379,-30.349542948244,47.3322126468164));
#38318=CARTESIAN_POINT('Ctrl Pts',(-32.8040610933859,-30.2025405326038,
47.4433424360361));
#38319=CARTESIAN_POINT('Ctrl Pts',(-33.9462031214054,-31.7005535288883,
47.5544722252559));
#38320=CARTESIAN_POINT('Ctrl Pts',(-33.3072011584087,-33.4726166881725,
47.6656020144756));
#38321=CARTESIAN_POINT('Ctrl Pts',(-31.4718628712426,-33.8969570243042,
47.7767318036953));
#38322=CARTESIAN_POINT('Ctrl Pts',(-30.1198699569067,-32.585222863435,47.8878615929151));
#38323=CARTESIAN_POINT('Ctrl Pts',(-30.4885516688484,-30.7378990844278,
47.9989913821347));
#38324=CARTESIAN_POINT('Ctrl Pts',(-32.2404945024855,-30.0456363764377,
48.1101211713545));
#38325=CARTESIAN_POINT('Ctrl Pts',(-33.7723393755021,-31.1419860625409,
48.2212509605742));
#38326=CARTESIAN_POINT('Ctrl Pts',(-33.6821584722794,-33.023580799433,48.3323807497939));
#38327=CARTESIAN_POINT('Ctrl Pts',(-32.0524843774755,-33.9684054889555,
48.4435105390136));
#38328=CARTESIAN_POINT('Ctrl Pts',(-30.3747771495755,-33.1117668214546,
48.5546403282334));
#38329=CARTESIAN_POINT('Ctrl Pts',(-30.184456249576,-31.2376512155675,48.6657701174531));
#38330=CARTESIAN_POINT('Ctrl Pts',(-31.6557013012125,-30.0612289498648,
48.7768999066729));
#38331=CARTESIAN_POINT('Ctrl Pts',(-33.4420447882153,-30.6591489241492,
48.8880296958926));
#38332=CARTESIAN_POINT('Ctrl Pts',(-33.9086445233681,-32.4842012621279,
48.9991594851123));
#38333=CARTESIAN_POINT('Ctrl Pts',(-32.6284734891223,-33.8661178559511,
49.1102892743321));
#38334=CARTESIAN_POINT('Ctrl Pts',(-30.773130333143,-33.5401836252133,49.2214190635517));
#38335=CARTESIAN_POINT('Ctrl Pts',(-30.0406049914237,-31.8046900432762,
49.3325488527715));
#38336=CARTESIAN_POINT('Ctrl Pts',(-31.1012967127994,-30.2479420156844,
49.4436786419912));
#38337=CARTESIAN_POINT('Ctrl Pts',(-32.9844719365898,-30.2946584550606,
49.554808431211));
#38338=CARTESIAN_POINT('Ctrl Pts',(-33.9666691201668,-31.9020849827063,
49.6659382204307));
#38339=CARTESIAN_POINT('Ctrl Pts',(-33.1489920526057,-33.5991222723351,
49.7770680096504));
#38340=CARTESIAN_POINT('Ctrl Pts',(-31.2797699187998,-33.8326602000818,
49.8881977988701));
#38341=CARTESIAN_POINT('Ctrl Pts',(-30.0696945447384,-32.3889673870857,
49.9993275880899));
#38342=CARTESIAN_POINT('Ctrl Pts',(-30.6262137900413,-30.5892958396048,
50.1104573773095));
#38343=CARTESIAN_POINT('Ctrl Pts',(-32.4400072766077,-30.0806854412674,
50.2215871665294));
#38344=CARTESIAN_POINT('Ctrl Pts',(-33.8511108753022,-31.3286109129836,
50.3327169557489));
#38345=CARTESIAN_POINT('Ctrl Pts',(-33.5680978753831,-33.1909843962233,
50.4438467449688));
#38346=CARTESIAN_POINT('Ctrl Pts',(-31.849978705224,-33.9633818757322,50.5549765341884));
#38347=CARTESIAN_POINT('Ctrl Pts',(-30.2691573971359,-32.9389135545513,
50.6661063234082));
#38348=CARTESIAN_POINT('Ctrl Pts',(-30.2723844689724,-31.0551617303574,
50.7772361126279));
#38349=CARTESIAN_POINT('Ctrl Pts',(-31.8567065396152,-30.0361156441587,
50.8883659018477));
#38350=CARTESIAN_POINT('Ctrl Pts',(-33.5721692312094,-30.8143952230609,
50.9994956910673));
#38351=CARTESIAN_POINT('Ctrl Pts',(-33.8487996919451,-32.6777274363229,
51.1106254802872));
#38352=CARTESIAN_POINT('Ctrl Pts',(-32.4334287238539,-33.9208108498002,
51.2217552695068));
#38353=CARTESIAN_POINT('Ctrl Pts',(-30.6213884883404,-33.4059890032924,
51.3328850587266));
#38354=CARTESIAN_POINT('Ctrl Pts',(-30.0710385572647,-31.6044212694241,
51.4440148479462));
#38355=CARTESIAN_POINT('Ctrl Pts',(-31.2860532210798,-30.1648828976553,
51.5551446371661));
#38356=CARTESIAN_POINT('Ctrl Pts',(-33.1544642321263,-30.4048238013925,
51.6662744263857));
#38357=CARTESIAN_POINT('Ctrl Pts',(-33.9663221023376,-32.1046526543067,
51.7774042156056));
#38358=CARTESIAN_POINT('Ctrl Pts',(-32.9786232989337,-33.7087045503785,
51.8885340048251));
#38359=CARTESIAN_POINT('Ctrl Pts',(-31.0952990837456,-33.7489685374884,
51.9996637940449));
#38360=CARTESIAN_POINT('Ctrl Pts',(-30.0399472990725,-32.1885955543356,
52.1107935832646));
#38361=CARTESIAN_POINT('Ctrl Pts',(-30.7784145635932,-30.4556218295225,
52.2219233724844));
#38362=CARTESIAN_POINT('Ctrl Pts',(-32.6348634270627,-30.1360465266472,
52.3330531617041));
#38363=CARTESIAN_POINT('Ctrl Pts',(-33.9102924537887,-31.5223406974568,
52.4441829509238));
#38364=CARTESIAN_POINT('Ctrl Pts',(-33.4374419750523,-33.3457845340362,
52.5553127401435));
#38365=CARTESIAN_POINT('Ctrl Pts',(-31.6490613137411,-33.9375788765242,
52.6664425293633));
#38366=CARTESIAN_POINT('Ctrl Pts',(-30.1818537058118,-32.7561261673534,
52.777572318583));
#38367=CARTESIAN_POINT('Ctrl Pts',(-30.3785982775114,-30.8826668248174,
52.8887021078027));
#38368=CARTESIAN_POINT('Ctrl Pts',(-32.0592233947483,-30.0317948524369,
52.9998318970224));
#38369=CARTESIAN_POINT('Ctrl Pts',(-33.6856651825576,-30.9821708820847,
53.1109616862422));
#38370=CARTESIAN_POINT('Ctrl Pts',(-33.7693702652999,-32.864116447248,53.2220914754619));
#38371=CARTESIAN_POINT('Ctrl Pts',(-32.2338346006141,-33.9551065574643,
53.3332212646817));
#38372=CARTESIAN_POINT('Ctrl Pts',(-30.4841619464795,-33.2570527350258,
53.4443510539013));
#38373=CARTESIAN_POINT('Ctrl Pts',(-30.1220333444858,-31.4080660256503,
53.5554808431211));
#38374=CARTESIAN_POINT('Ctrl Pts',(-31.4780737014122,-30.1017857222274,
53.6666106323408));
#38375=CARTESIAN_POINT('Ctrl Pts',(-33.3128174529624,-30.5307878228056,
53.7777404215605));
#38376=CARTESIAN_POINT('Ctrl Pts',(-33.9440063061494,-32.3083920037255,
53.8888702107803));
#38377=CARTESIAN_POINT('Ctrl Pts',(-33.1815065089974,-33.2986349005747,
53.9629567369268));
#38378=CARTESIAN_POINT('Ctrl Pts',(-32.6750771856749,-33.5230977622534,
54.));
#38379=CARTESIAN_POINT('Ctrl Pts',(-30.336158884875,-31.9990545752999,41.6214803633902));
#38380=CARTESIAN_POINT('Ctrl Pts',(-30.3350387011371,-31.7834963203764,
41.6358513744636));
#38381=CARTESIAN_POINT('Ctrl Pts',(-30.3739090865848,-31.5683253856938,
41.650222385537));
#38382=CARTESIAN_POINT('Ctrl Pts',(-30.4546428726593,-31.3702163272604,
41.6645933966103));
#38383=CARTESIAN_POINT('Ctrl Pts',(-30.6627453409677,-30.8595629061987,
41.7016366596836));
#38384=CARTESIAN_POINT('Ctrl Pts',(-31.1489973374487,-30.4622722974605,
41.7386799227568));
#38385=CARTESIAN_POINT('Ctrl Pts',(-31.6908816348332,-30.3601281633497,
41.7757231858301));
#38386=CARTESIAN_POINT('Ctrl Pts',(-32.2327659322177,-30.2579840292389,
41.8127664489033));
#38387=CARTESIAN_POINT('Ctrl Pts',(-32.8302825305056,-30.4509863697556,
41.8498097119765));
#38388=CARTESIAN_POINT('Ctrl Pts',(-33.2100166050692,-30.8508256164995,
41.8868529750498));
#38389=CARTESIAN_POINT('Ctrl Pts',(-33.5897506796328,-31.2506648632435,
41.923896238123));
#38390=CARTESIAN_POINT('Ctrl Pts',(-33.7517022304721,-31.8573410162147,
41.9609395011963));
#38391=CARTESIAN_POINT('Ctrl Pts',(-33.6217603125026,-32.3932386924046,
41.9979827642695));
#38392=CARTESIAN_POINT('Ctrl Pts',(-33.4918183945331,-32.9291363685945,
42.0350260273428));
#38393=CARTESIAN_POINT('Ctrl Pts',(-33.0699830077549,-33.3942555680032,
42.072069290416));
#38394=CARTESIAN_POINT('Ctrl Pts',(-32.5492851488473,-33.5757621181193,
42.1091125534892));
#38395=CARTESIAN_POINT('Ctrl Pts',(-32.0285872899397,-33.7572686682353,
42.1461558165625));
#38396=CARTESIAN_POINT('Ctrl Pts',(-31.4090269589028,-33.6551625690588,
42.1831990796357));
#38397=CARTESIAN_POINT('Ctrl Pts',(-30.9741108911154,-33.3161660829397,
42.220242342709));
#38398=CARTESIAN_POINT('Ctrl Pts',(-30.5779071173622,-33.0073439973986,
42.2539883496027));
#38399=CARTESIAN_POINT('Ctrl Pts',(-30.3349398101202,-32.5019263328413,
42.2877343564965));
#38400=CARTESIAN_POINT('Ctrl Pts',(-30.3317921677919,-31.9991447210974,
42.3214803633902));
#38401=CARTESIAN_POINT('Ctrl Pts',(-31.4698297828114,-33.9851743256717,
41.));
#38402=CARTESIAN_POINT('Ctrl Pts',(-31.4011629206477,-33.9597495324007,
41.));
#38403=CARTESIAN_POINT('Ctrl Pts',(-31.3341994075765,-33.9304353968824,
41.));
#38404=CARTESIAN_POINT('Ctrl Pts',(-31.2691282231929,-33.8975258421853,
41.));
#38405=CARTESIAN_POINT('Ctrl Pts',(-31.2022479171691,-33.8637013296902,
41.));
#38406=CARTESIAN_POINT('Ctrl Pts',(-31.1373658528129,-33.8260780092996,
41.));
#38407=CARTESIAN_POINT('Ctrl Pts',(-31.0747184293343,-33.7849303663298,
41.));
#38408=CARTESIAN_POINT('Ctrl Pts',(-31.0217877705273,-33.7501648208402,
41.));
#38409=CARTESIAN_POINT('Ctrl Pts',(-30.970452648882,-33.7128823799464,41.));
#38410=CARTESIAN_POINT('Ctrl Pts',(-30.9208783808178,-33.6732305849818,
41.));
#38411=CARTESIAN_POINT('Ctrl Pts',(-30.8988476542381,-33.6556093898059,
41.));
#38412=CARTESIAN_POINT('Ctrl Pts',(-30.8771649817797,-33.6375200920571,
41.));
#38413=CARTESIAN_POINT('Ctrl Pts',(-30.8558464259774,-33.6189749164796,
41.));
#38414=CARTESIAN_POINT('Ctrl Pts',(-30.8441323514957,-33.6087847530367,
41.));
#38415=CARTESIAN_POINT('Ctrl Pts',(-30.8325282309531,-33.598456941651,41.));
#38416=CARTESIAN_POINT('Ctrl Pts',(-30.821036863453,-33.5879934687363,41.));
#38417=CARTESIAN_POINT('Ctrl Pts',(-30.8104448788549,-33.5783489295678,
41.));
#38418=CARTESIAN_POINT('Ctrl Pts',(-30.7999472574529,-33.5685876204844,
41.));
#38419=CARTESIAN_POINT('Ctrl Pts',(-30.7895620725801,-33.5587265457271,
41.));
#38420=CARTESIAN_POINT('Ctrl Pts',(-30.7364770283431,-33.508320549481,41.));
#38421=CARTESIAN_POINT('Ctrl Pts',(-30.68623196656,-33.4552262597685,41.));
#38422=CARTESIAN_POINT('Ctrl Pts',(-30.6390455793197,-33.3997030109773,
41.));
#38423=CARTESIAN_POINT('Ctrl Pts',(-30.5922257616164,-33.344611097001,41.));
#38424=CARTESIAN_POINT('Ctrl Pts',(-30.5484167718099,-33.2871269332147,
41.));
#38425=CARTESIAN_POINT('Ctrl Pts',(-30.5078770353379,-33.2274796163432,
41.));
#38426=CARTESIAN_POINT('Ctrl Pts',(-30.4741909267921,-33.1779162455506,
41.));
#38427=CARTESIAN_POINT('Ctrl Pts',(-30.4427627578091,-33.1268586479626,
41.));
#38428=CARTESIAN_POINT('Ctrl Pts',(-30.4137683914513,-33.0744317875342,
41.));
#38429=CARTESIAN_POINT('Ctrl Pts',(-30.4016605159042,-33.0525386413428,
41.));
#38430=CARTESIAN_POINT('Ctrl Pts',(-30.3899773803102,-33.0304066773724,
41.));
#38431=CARTESIAN_POINT('Ctrl Pts',(-30.3787332334151,-33.0080449125542,
41.));
#38432=CARTESIAN_POINT('Ctrl Pts',(-30.3735336402044,-32.9977042365018,
41.));
#38433=CARTESIAN_POINT('Ctrl Pts',(-30.3684279320372,-32.9873144202456,
41.));
#38434=CARTESIAN_POINT('Ctrl Pts',(-30.36341758307,-32.9768763573879,41.));
#38435=CARTESIAN_POINT('Ctrl Pts',(-30.3581837835811,-32.9659727799311,
41.));
#38436=CARTESIAN_POINT('Ctrl Pts',(-30.3530576442939,-32.9550240006742,
41.));
#38437=CARTESIAN_POINT('Ctrl Pts',(-30.3480422353361,-32.9440353490892,
41.));
#38438=CARTESIAN_POINT('Ctrl Pts',(-30.319501876602,-32.8815040458843,41.));
#38439=CARTESIAN_POINT('Ctrl Pts',(-30.2945225097578,-32.8176393566208,
41.));
#38440=CARTESIAN_POINT('Ctrl Pts',(-30.273327611576,-32.7526456143523,41.));
#38441=CARTESIAN_POINT('Ctrl Pts',(-30.2541304481184,-32.6937778866872,
41.));
#38442=CARTESIAN_POINT('Ctrl Pts',(-30.238038284882,-32.6339833166677,41.));
#38443=CARTESIAN_POINT('Ctrl Pts',(-30.2252538389208,-32.5734089087092,
41.));
#38444=CARTESIAN_POINT('Ctrl Pts',(-30.2101196528407,-32.5017011190627,
41.));
#38445=CARTESIAN_POINT('Ctrl Pts',(-30.1996202129508,-32.4288989655352,
41.));
#38446=CARTESIAN_POINT('Ctrl Pts',(-30.1936803700894,-32.3554256399494,
41.));
#38447=CARTESIAN_POINT('Ctrl Pts',(-30.1923734295127,-32.3392593418243,
41.));
#38448=CARTESIAN_POINT('Ctrl Pts',(-30.1912874562889,-32.3230606319689,
41.));
#38449=CARTESIAN_POINT('Ctrl Pts',(-30.1904220188582,-32.3068341825425,
41.));
#38450=CARTESIAN_POINT('Ctrl Pts',(-30.1895243797817,-32.2900039709495,
41.));
#38451=CARTESIAN_POINT('Ctrl Pts',(-30.1888639831893,-32.2731376890812,
41.));
#38452=CARTESIAN_POINT('Ctrl Pts',(-30.1884409105021,-32.2562749512595,
41.));
#38453=CARTESIAN_POINT('Ctrl Pts',(-30.1867207285335,-32.1877123178837,
41.));
#38454=CARTESIAN_POINT('Ctrl Pts',(-30.1889121731841,-32.119121789089,41.));
#38455=CARTESIAN_POINT('Ctrl Pts',(-30.1948946640324,-32.0508418040844,
41.));
#38456=CARTESIAN_POINT('Ctrl Pts',(-30.2008758819965,-31.9825763468949,
41.));
#38457=CARTESIAN_POINT('Ctrl Pts',(-30.2106469868098,-31.9146202295201,
41.));
#38458=CARTESIAN_POINT('Ctrl Pts',(-30.2241370789842,-31.8473267076867,
41.));
#38459=CARTESIAN_POINT('Ctrl Pts',(-30.2338950669342,-31.7986502889733,
41.));
#38460=CARTESIAN_POINT('Ctrl Pts',(-30.2455999819607,-31.7503208244277,
41.));
#38461=CARTESIAN_POINT('Ctrl Pts',(-30.2592391795709,-31.7024816531862,
41.));
#38462=CARTESIAN_POINT('Ctrl Pts',(-30.2694738036972,-31.6665839449658,
41.));
#38463=CARTESIAN_POINT('Ctrl Pts',(-30.2807978226536,-31.6309624632629,
41.));
#38464=CARTESIAN_POINT('Ctrl Pts',(-30.2932098063328,-31.5956819460291,
41.));
#38465=CARTESIAN_POINT('Ctrl Pts',(-30.2973425061779,-31.5839349286404,
41.));
#38466=CARTESIAN_POINT('Ctrl Pts',(-30.3015926355275,-31.572234881057,41.));
#38467=CARTESIAN_POINT('Ctrl Pts',(-30.305959527106,-31.5605844299902,41.));
#38468=CARTESIAN_POINT('Ctrl Pts',(-30.3290832944906,-31.498892419655,41.));
#38469=CARTESIAN_POINT('Ctrl Pts',(-30.3554795854277,-31.4385839314187,
41.));
#38470=CARTESIAN_POINT('Ctrl Pts',(-30.3850984048383,-31.3799931438224,
41.));
#38471=CARTESIAN_POINT('Ctrl Pts',(-30.4059238341125,-31.3387970959215,
41.));
#38472=CARTESIAN_POINT('Ctrl Pts',(-30.4283432407334,-31.2984507577224,
41.));
#38473=CARTESIAN_POINT('Ctrl Pts',(-30.4523496359434,-31.2590816244303,
41.));
#38474=CARTESIAN_POINT('Ctrl Pts',(-30.460063473454,-31.2464313662597,41.));
#38475=CARTESIAN_POINT('Ctrl Pts',(-30.4679423137434,-31.2338804122318,
41.));
#38476=CARTESIAN_POINT('Ctrl Pts',(-30.4759826345042,-31.2214385753381,
41.));
#38477=CARTESIAN_POINT('Ctrl Pts',(-30.5102255955582,-31.1684499758944,
41.));
#38478=CARTESIAN_POINT('Ctrl Pts',(-30.5473242690744,-31.1175452556629,
41.));
#38479=CARTESIAN_POINT('Ctrl Pts',(-30.5872444101701,-31.0690397081128,
41.));
#38480=CARTESIAN_POINT('Ctrl Pts',(-30.6240203632449,-31.0243545519083,
41.));
#38481=CARTESIAN_POINT('Ctrl Pts',(-30.6631914251233,-30.9817054320841,
41.));
#38482=CARTESIAN_POINT('Ctrl Pts',(-30.7047522428173,-30.9413717231824,
41.));
#38483=CARTESIAN_POINT('Ctrl Pts',(-30.7125940811408,-30.9337614199751,
41.));
#38484=CARTESIAN_POINT('Ctrl Pts',(-30.7205210515567,-30.926233652583,41.));
#38485=CARTESIAN_POINT('Ctrl Pts',(-30.7285315473809,-30.9187890928311,
41.));
#38486=CARTESIAN_POINT('Origin',(-32.,-32.,48.));
#38487=CARTESIAN_POINT('Origin',(-32.,32.,54.));
#38488=CARTESIAN_POINT('Ctrl Pts',(-32.6750771856749,30.4769022377466,54.));
#38489=CARTESIAN_POINT('Ctrl Pts',(-32.7347606915771,30.4954885176555,54.));
#38490=CARTESIAN_POINT('Ctrl Pts',(-32.7931316468243,30.5176493824028,54.));
#38491=CARTESIAN_POINT('Ctrl Pts',(-32.8500334991629,30.5430859583899,54.));
#38492=CARTESIAN_POINT('Ctrl Pts',(-32.8861162422491,30.5592158627536,54.));
#38493=CARTESIAN_POINT('Ctrl Pts',(-32.9216082931908,30.5766640695137,54.));
#38494=CARTESIAN_POINT('Ctrl Pts',(-32.9564688344476,30.5953648077861,54.));
#38495=CARTESIAN_POINT('Ctrl Pts',(-32.9802311105381,30.6081119450911,54.));
#38496=CARTESIAN_POINT('Ctrl Pts',(-33.0036999498365,30.6214412122672,54.));
#38497=CARTESIAN_POINT('Ctrl Pts',(-33.0268619608851,30.6353337365551,54.));
#38498=CARTESIAN_POINT('Ctrl Pts',(-33.0392110030252,30.6427406654053,54.));
#38499=CARTESIAN_POINT('Ctrl Pts',(-33.0514726639847,30.650307779206,54.));
#38500=CARTESIAN_POINT('Ctrl Pts',(-33.0636328281387,30.6580243195221,54.));
#38501=CARTESIAN_POINT('Ctrl Pts',(-33.1193346579069,30.6933713271479,54.));
#38502=CARTESIAN_POINT('Ctrl Pts',(-33.1729727156271,30.7318877508992,54.));
#38503=CARTESIAN_POINT('Ctrl Pts',(-33.2243651773974,30.7732711116722,54.));
#38504=CARTESIAN_POINT('Ctrl Pts',(-33.2614339884367,30.8031204694929,54.));
#38505=CARTESIAN_POINT('Ctrl Pts',(-33.2973344258717,30.8344625918461,54.));
#38506=CARTESIAN_POINT('Ctrl Pts',(-33.3319929726109,30.8671998395399,54.));
#38507=CARTESIAN_POINT('Ctrl Pts',(-33.3414619332501,30.8761438876612,54.));
#38508=CARTESIAN_POINT('Ctrl Pts',(-33.3508381622407,30.8851921406493,54.));
#38509=CARTESIAN_POINT('Ctrl Pts',(-33.360120076321,30.89434275958,54.));
#38510=CARTESIAN_POINT('Ctrl Pts',(-33.3696838750555,30.9037712758313,54.));
#38511=CARTESIAN_POINT('Ctrl Pts',(-33.3791418362518,30.9133029001982,54.));
#38512=CARTESIAN_POINT('Ctrl Pts',(-33.3884887348017,30.9229312087312,54.));
#38513=CARTESIAN_POINT('Ctrl Pts',(-33.435751083172,30.9716164993304,54.));
#38514=CARTESIAN_POINT('Ctrl Pts',(-33.4802065476745,31.0228007164435,54.));
#38515=CARTESIAN_POINT('Ctrl Pts',(-33.5216714229955,31.0761767682427,54.));
#38516=CARTESIAN_POINT('Ctrl Pts',(-33.5637355354488,31.1303241936916,54.));
#38517=CARTESIAN_POINT('Ctrl Pts',(-33.6027228866653,31.1867278444332,54.));
#38518=CARTESIAN_POINT('Ctrl Pts',(-33.6384173336076,31.2451140319467,54.));
#38519=CARTESIAN_POINT('Ctrl Pts',(-33.6605280372079,31.2812809933946,54.));
#38520=CARTESIAN_POINT('Ctrl Pts',(-33.6813746887815,31.3182095673848,54.));
#38521=CARTESIAN_POINT('Ctrl Pts',(-33.7008990002285,31.3558419756537,54.));
#38522=CARTESIAN_POINT('Ctrl Pts',(-33.7168832701209,31.3866510811169,54.));
#38523=CARTESIAN_POINT('Ctrl Pts',(-33.7319811659046,31.4179320443681,54.));
#38524=CARTESIAN_POINT('Ctrl Pts',(-33.7461573794449,31.4496553736956,54.));
#38525=CARTESIAN_POINT('Ctrl Pts',(-33.7519693974655,31.462661425079,54.));
#38526=CARTESIAN_POINT('Ctrl Pts',(-33.7576273458872,31.4757443280942,54.));
#38527=CARTESIAN_POINT('Ctrl Pts',(-33.7631196222834,31.4888795631979,54.));
#38528=CARTESIAN_POINT('Ctrl Pts',(-33.7903102098283,31.5539081113344,54.));
#38529=CARTESIAN_POINT('Ctrl Pts',(-33.8134950874387,31.6203284923708,54.));
#38530=CARTESIAN_POINT('Ctrl Pts',(-33.8324626822549,31.6878455732216,54.));
#38531=CARTESIAN_POINT('Ctrl Pts',(-33.8345627116769,31.6953208413115,54.));
#38532=CARTESIAN_POINT('Ctrl Pts',(-33.836611009148,31.7028095915747,54.));
#38533=CARTESIAN_POINT('Ctrl Pts',(-33.8386072594899,31.710311451093,54.));
#38534=CARTESIAN_POINT('Ctrl Pts',(-33.855945393719,31.7754677316278,54.));
#38535=CARTESIAN_POINT('Ctrl Pts',(-33.8693612283885,31.8416108585899,54.));
#38536=CARTESIAN_POINT('Ctrl Pts',(-33.8790088087618,31.9084363750645,54.));
#38537=CARTESIAN_POINT('Ctrl Pts',(-33.8893872742774,31.9803244849798,54.));
#38538=CARTESIAN_POINT('Ctrl Pts',(-33.8954055239578,32.0530030863577,54.));
#38539=CARTESIAN_POINT('Ctrl Pts',(-33.8971951879124,32.1261156983931,54.));
#38540=CARTESIAN_POINT('Ctrl Pts',(-33.8975152604702,32.1391915278981,54.));
#38541=CARTESIAN_POINT('Ctrl Pts',(-33.8976999206002,32.1522812739254,54.));
#38542=CARTESIAN_POINT('Ctrl Pts',(-33.897749714621,32.1653829318895,54.));
#38543=CARTESIAN_POINT('Ctrl Pts',(-33.8977946808874,32.177214325139,54.));
#38544=CARTESIAN_POINT('Ctrl Pts',(-33.8977296105587,32.1890468266652,54.));
#38545=CARTESIAN_POINT('Ctrl Pts',(-33.8975554553278,32.2008754645531,54.));
#38546=CARTESIAN_POINT('Ctrl Pts',(-33.8965092280538,32.2719353087169,54.));
#38547=CARTESIAN_POINT('Ctrl Pts',(-33.8915304228521,32.3428930409877,54.));
#38548=CARTESIAN_POINT('Ctrl Pts',(-33.8827991703013,32.4134130591355,54.));
#38549=CARTESIAN_POINT('Ctrl Pts',(-33.8738836831824,32.4854210911754,54.));
#38550=CARTESIAN_POINT('Ctrl Pts',(-33.8610557741427,32.5569736774994,54.));
#38551=CARTESIAN_POINT('Ctrl Pts',(-33.8444545204575,32.6277297102758,54.));
#38552=CARTESIAN_POINT('Ctrl Pts',(-33.8277523485976,32.6989158653678,54.));
#38553=CARTESIAN_POINT('Ctrl Pts',(-33.8072307379804,32.7692968235389,54.));
#38554=CARTESIAN_POINT('Ctrl Pts',(-33.7829789156768,32.8385261464761,54.));
#38555=CARTESIAN_POINT('Ctrl Pts',(-33.7769979005134,32.8555995698689,54.));
#38556=CARTESIAN_POINT('Ctrl Pts',(-33.7707897613597,32.8726029088931,54.));
#38557=CARTESIAN_POINT('Ctrl Pts',(-33.7643553594181,32.8895308570373,54.));
#38558=CARTESIAN_POINT('Ctrl Pts',(-33.7592863747482,32.9028665967708,54.));
#38559=CARTESIAN_POINT('Ctrl Pts',(-33.7540761916856,32.9161571498072,54.));
#38560=CARTESIAN_POINT('Ctrl Pts',(-33.7487336714912,32.9293797191499,54.));
#38561=CARTESIAN_POINT('Ctrl Pts',(-33.7205084932337,32.9992361470419,54.));
#38562=CARTESIAN_POINT('Ctrl Pts',(-33.6885470824167,33.0673216292728,54.));
#38563=CARTESIAN_POINT('Ctrl Pts',(-33.6530075460646,33.1332788252052,54.));
#38564=CARTESIAN_POINT('Ctrl Pts',(-33.6174290020438,33.1993084147791,54.));
#38565=CARTESIAN_POINT('Ctrl Pts',(-33.5782643022281,33.2632061589058,54.));
#38566=CARTESIAN_POINT('Ctrl Pts',(-33.5356203080281,33.3246091157058,54.));
#38567=CARTESIAN_POINT('Ctrl Pts',(-33.4939464336363,33.3846151999615,54.));
#38568=CARTESIAN_POINT('Ctrl Pts',(-33.4489494285267,33.4422396978105,54.));
#38569=CARTESIAN_POINT('Ctrl Pts',(-33.4006836910636,33.497124259357,54.));
#38570=CARTESIAN_POINT('Ctrl Pts',(-33.3903484920103,33.5088767549854,54.));
#38571=CARTESIAN_POINT('Ctrl Pts',(-33.3798632561248,33.5205035150137,54.));
#38572=CARTESIAN_POINT('Ctrl Pts',(-33.3692282611413,33.532000833948,54.));
#38573=CARTESIAN_POINT('Ctrl Pts',(-33.360117214453,33.5418506373343,54.));
#38574=CARTESIAN_POINT('Ctrl Pts',(-33.3508962513759,33.5516054369775,54.));
#38575=CARTESIAN_POINT('Ctrl Pts',(-33.3415672325379,33.5612648174638,54.));
#38576=CARTESIAN_POINT('Ctrl Pts',(-32.3836679988468,34.0186125009919,54.));
#38577=CARTESIAN_POINT('Ctrl Pts',(-32.3093502844899,34.0256330949372,54.));
#38578=CARTESIAN_POINT('Ctrl Pts',(-32.2347844706668,34.0282517480001,54.));
#38579=CARTESIAN_POINT('Ctrl Pts',(-32.1602926743779,34.0266320545354,54.));
#38580=CARTESIAN_POINT('Ctrl Pts',(-32.0877589864994,34.025054936704,54.));
#38581=CARTESIAN_POINT('Ctrl Pts',(-32.0152946934488,34.0194587142989,54.));
#38582=CARTESIAN_POINT('Ctrl Pts',(-31.9432103734882,34.0099505607399,54.));
#38583=CARTESIAN_POINT('Ctrl Pts',(-31.9271201946013,34.0078282144137,54.));
#38584=CARTESIAN_POINT('Ctrl Pts',(-31.9110468943986,34.0055104663305,54.));
#38585=CARTESIAN_POINT('Ctrl Pts',(-31.8950008955345,34.0029993250679,54.));
#38586=CARTESIAN_POINT('Ctrl Pts',(-31.821367329252,33.9914759360805,54.));
#38587=CARTESIAN_POINT('Ctrl Pts',(-31.7484534135904,33.9759080373483,54.));
#38588=CARTESIAN_POINT('Ctrl Pts',(-31.6765910812025,33.9564351190568,54.));
#38589=CARTESIAN_POINT('Ctrl Pts',(-31.6261438367467,33.942765161004,54.));
#38590=CARTESIAN_POINT('Ctrl Pts',(-31.5762150883091,33.9271697110659,54.));
#38591=CARTESIAN_POINT('Ctrl Pts',(-31.526927605364,33.9096838836821,54.));
#38592=CARTESIAN_POINT('Ctrl Pts',(-31.5082001959596,33.9030399199691,54.));
#38593=CARTESIAN_POINT('Ctrl Pts',(-31.4895654503424,33.8961229364477,54.));
#38594=CARTESIAN_POINT('Ctrl Pts',(-31.4710304367965,33.8889344969223,54.));
#38595=CARTESIAN_POINT('Ctrl Pts',(-31.4533429023197,33.882074735443,54.));
#38596=CARTESIAN_POINT('Ctrl Pts',(-31.4357407268156,33.8749653206272,54.));
#38597=CARTESIAN_POINT('Ctrl Pts',(-31.4182609664101,33.8676208388457,54.));
#38598=CARTESIAN_POINT('Ctrl Pts',(-31.3513338147382,33.8395000159774,54.));
#38599=CARTESIAN_POINT('Ctrl Pts',(-31.2861267881216,33.8079111496751,54.));
#38600=CARTESIAN_POINT('Ctrl Pts',(-31.2229480924711,33.7729813893192,54.));
#38601=CARTESIAN_POINT('Ctrl Pts',(-31.1611264019049,33.7388018796912,54.));
#38602=CARTESIAN_POINT('Ctrl Pts',(-31.1012461490794,33.7014228251959,54.));
#38603=CARTESIAN_POINT('Ctrl Pts',(-31.043628468054,33.6609265400657,54.));
#38604=CARTESIAN_POINT('Ctrl Pts',(-30.987274236897,33.6213182640535,54.));
#38605=CARTESIAN_POINT('Ctrl Pts',(-30.9330838755882,33.5787274426741,54.));
#38606=CARTESIAN_POINT('Ctrl Pts',(-30.8813982876013,33.5332038702195,54.));
#38607=CARTESIAN_POINT('Ctrl Pts',(-30.8645714462744,33.5183831443622,54.));
#38608=CARTESIAN_POINT('Ctrl Pts',(-30.8480104467711,33.5032513889838,54.));
#38609=CARTESIAN_POINT('Ctrl Pts',(-30.8317281562672,33.4878098190582,54.));
#38610=CARTESIAN_POINT('Ctrl Pts',(-30.8225975555259,33.4791506681987,54.));
#38611=CARTESIAN_POINT('Ctrl Pts',(-30.8135537775277,33.4703931298114,54.));
#38612=CARTESIAN_POINT('Ctrl Pts',(-30.8046115462315,33.4615500351139,54.));
#38613=CARTESIAN_POINT('Ctrl Pts',(-30.7560461054599,33.4135230072332,54.));
#38614=CARTESIAN_POINT('Ctrl Pts',(-30.7103849708301,33.3628934275024,54.));
#38615=CARTESIAN_POINT('Ctrl Pts',(-30.667920505939,33.3097422848648,54.));
#38616=CARTESIAN_POINT('Ctrl Pts',(-30.6618145678856,33.3020997163021,54.));
#38617=CARTESIAN_POINT('Ctrl Pts',(-30.6557747947556,33.2944049635008,54.));
#38618=CARTESIAN_POINT('Ctrl Pts',(-30.6498021315748,33.2866582187114,54.));
#38619=CARTESIAN_POINT('Ctrl Pts',(-30.6074436612194,33.2317178596821,54.));
#38620=CARTESIAN_POINT('Ctrl Pts',(-30.5684565753518,33.1741638225229,54.));
#38621=CARTESIAN_POINT('Ctrl Pts',(-30.5329081125672,33.1143583196404,54.));
#38622=CARTESIAN_POINT('Ctrl Pts',(-30.4997462774684,33.0585679965369,54.));
#38623=CARTESIAN_POINT('Ctrl Pts',(-30.4695772466851,33.0008173969119,54.));
#38624=CARTESIAN_POINT('Ctrl Pts',(-30.4424953173611,32.9413951242111,54.));
#38625=CARTESIAN_POINT('Ctrl Pts',(-30.4366015041344,32.92846311436,54.));
#38626=CARTESIAN_POINT('Ctrl Pts',(-30.4308540497917,32.9154519378522,54.));
#38627=CARTESIAN_POINT('Ctrl Pts',(-30.4252541718586,32.9023645968498,54.));
#38628=CARTESIAN_POINT('Ctrl Pts',(-30.4207268719756,32.8917839523971,54.));
#38629=CARTESIAN_POINT('Ctrl Pts',(-30.4162962542086,32.8811538243346,54.));
#38630=CARTESIAN_POINT('Ctrl Pts',(-30.4119679861992,32.8704888342707,54.));
#38631=CARTESIAN_POINT('Ctrl Pts',(-30.3862552098172,32.8071317353044,54.));
#38632=CARTESIAN_POINT('Ctrl Pts',(-30.3640997288972,32.7424289154671,54.));
#38633=CARTESIAN_POINT('Ctrl Pts',(-30.3455478113908,32.6767304436005,54.));
#38634=CARTESIAN_POINT('Ctrl Pts',(-30.3270815332802,32.6113352491414,54.));
#38635=CARTESIAN_POINT('Ctrl Pts',(-30.3121856182907,32.5449524378339,54.));
#38636=CARTESIAN_POINT('Ctrl Pts',(-30.3009567584366,32.4779246219716,54.));
#38637=CARTESIAN_POINT('Ctrl Pts',(-30.2899684808235,32.412332900455,54.));
#38638=CARTESIAN_POINT('Ctrl Pts',(-30.2824919357175,32.3461225531827,54.));
#38639=CARTESIAN_POINT('Ctrl Pts',(-30.2786656210298,32.279627521379,54.));
#38640=CARTESIAN_POINT('Ctrl Pts',(-30.2775523223255,32.2602802280194,54.));
#38641=CARTESIAN_POINT('Ctrl Pts',(-30.276748348819,32.2409089692141,54.));
#38642=CARTESIAN_POINT('Ctrl Pts',(-30.2762578731991,32.2215223570683,54.));
#38643=CARTESIAN_POINT('Ctrl Pts',(-30.2759857301979,32.2107655924154,54.));
#38644=CARTESIAN_POINT('Ctrl Pts',(-30.2758103549668,32.2000138517791,54.));
#38645=CARTESIAN_POINT('Ctrl Pts',(-30.2757319784298,32.189268592358,54.));
#38646=CARTESIAN_POINT('Ctrl Pts',(-30.2752558367538,32.1239905637135,54.));
#38647=CARTESIAN_POINT('Ctrl Pts',(-30.2783554890008,32.058949723192,54.));
#38648=CARTESIAN_POINT('Ctrl Pts',(-30.2851111704578,31.9944559018851,54.));
#38649=CARTESIAN_POINT('Ctrl Pts',(-30.292024200112,31.9284599395171,54.));
#38650=CARTESIAN_POINT('Ctrl Pts',(-30.3027653489992,31.8630356306402,54.));
#38651=CARTESIAN_POINT('Ctrl Pts',(-30.3174745268228,31.7985356931485,54.));
#38652=CARTESIAN_POINT('Ctrl Pts',(-30.3311068214881,31.7387579024165,54.));
#38653=CARTESIAN_POINT('Ctrl Pts',(-30.3481479575203,31.679773639241,54.));
#38654=CARTESIAN_POINT('Ctrl Pts',(-30.3687510878919,31.6218918797604,54.));
#38655=CARTESIAN_POINT('Ctrl Pts',(-30.3703786322379,31.6173195099952,54.));
#38656=CARTESIAN_POINT('Ctrl Pts',(-30.372028424917,31.612754037598,54.));
#38657=CARTESIAN_POINT('Ctrl Pts',(-30.373700552093,31.6081956242523,54.));
#38658=CARTESIAN_POINT('Ctrl Pts',(-30.3774632060968,31.597938191401,54.));
#38659=CARTESIAN_POINT('Ctrl Pts',(-30.3813389495473,31.5877164997064,54.));
#38660=CARTESIAN_POINT('Ctrl Pts',(-30.3853267261146,31.5775319120267,54.));
#38661=CARTESIAN_POINT('Origin',(-32.,32.,39.4540747194623));
#38662=CARTESIAN_POINT('Ctrl Pts',(-29.9434322456991,32.0014925908821,41.2040747194623));
#38663=CARTESIAN_POINT('Ctrl Pts',(-29.9426158532448,32.09958269322,41.2094078928853));
#38664=CARTESIAN_POINT('Ctrl Pts',(-29.9935881745736,32.8781627954851,41.2517843293816));
#38665=CARTESIAN_POINT('Ctrl Pts',(-30.9882785960482,34.2080088094421,41.3312040289512));
#38666=CARTESIAN_POINT('Ctrl Pts',(-33.3060692860357,34.0473904772534,41.4423338181709));
#38667=CARTESIAN_POINT('Ctrl Pts',(-34.4285436298619,32.0133707862788,41.5534636073906));
#38668=CARTESIAN_POINT('Ctrl Pts',(-33.3284492137394,29.9669383950752,41.6645933966104));
#38669=CARTESIAN_POINT('Ctrl Pts',(-31.0125684250491,29.7812307990702,41.7757231858301));
#38670=CARTESIAN_POINT('Ctrl Pts',(-29.9981580758837,31.1064229367225,41.8555502934474));
#38671=CARTESIAN_POINT('Ctrl Pts',(-29.9427300285746,31.8927563400753,41.8983341379915));
#38672=CARTESIAN_POINT('Ctrl Pts',(-29.9436380261218,31.9983919808556,41.9040747194623));
#38673=CARTESIAN_POINT('Ctrl Pts',(-29.9473238061977,31.9976393779993,41.1459252805377));
#38674=CARTESIAN_POINT('Ctrl Pts',(-29.9508741641786,32.4677619363521,41.1713700465049));
#38675=CARTESIAN_POINT('Ctrl Pts',(-30.3433201135815,33.6293341735692,41.2338580755455));
#38676=CARTESIAN_POINT('Ctrl Pts',(-32.2715961695763,34.4127962262488,41.3333893676592));
#38677=CARTESIAN_POINT('Ctrl Pts',(-34.1743722121293,33.0815585185448,41.4445191568789));
#38678=CARTESIAN_POINT('Ctrl Pts',(-34.088014018114,30.7594030715832,41.5556489460986));
#38679=CARTESIAN_POINT('Ctrl Pts',(-32.0903101568642,29.5731769531958,41.6667787353184));
#38680=CARTESIAN_POINT('Ctrl Pts',(-30.2791651722886,30.473897298874,41.7635375134647));
#38681=CARTESIAN_POINT('Ctrl Pts',(-29.9500923049499,31.5817394200461,41.8232530285378));
#38682=CARTESIAN_POINT('Ctrl Pts',(-29.9479126851747,32.0011660315207,41.8459252805377));
#38683=CARTESIAN_POINT('Ctrl Pts',(-33.2690708798524,33.0793586530485,41.));
#38684=CARTESIAN_POINT('Ctrl Pts',(-33.6279571482407,32.6573931542737,41.0370432630732));
#38685=CARTESIAN_POINT('Ctrl Pts',(-33.8852969018116,31.4343804031744,41.1111297892197));
#38686=CARTESIAN_POINT('Ctrl Pts',(-32.545339605534,30.1066748127004,41.2222595784395));
#38687=CARTESIAN_POINT('Ctrl Pts',(-30.7061568094468,30.5162239665622,41.3333893676592));
#38688=CARTESIAN_POINT('Ctrl Pts',(-30.0511799680217,32.2815047919735,41.4445191568789));
#38689=CARTESIAN_POINT('Ctrl Pts',(-31.1796920019547,33.7902628916075,41.5556489460986));
#38690=CARTESIAN_POINT('Ctrl Pts',(-33.0589665071349,33.6600328677963,41.6667787353184));
#38691=CARTESIAN_POINT('Ctrl Pts',(-33.9690734577686,32.010841090128,41.7779085245381));
#38692=CARTESIAN_POINT('Ctrl Pts',(-33.0771122472757,30.3515850425576,41.8890383137579));
#38693=CARTESIAN_POINT('Ctrl Pts',(-31.199386298154,30.2010125374138,42.0001681029776));
#38694=CARTESIAN_POINT('Ctrl Pts',(-30.0543749890887,31.6968174506273,42.1112978921972));
#38695=CARTESIAN_POINT('Ctrl Pts',(-30.6899777507586,33.4701101328659,42.222427681417));
#38696=CARTESIAN_POINT('Ctrl Pts',(-32.5244990925998,33.8979646750396,42.3335574706367));
#38697=CARTESIAN_POINT('Ctrl Pts',(-33.8790043385183,32.5888272218981,42.4446872598564));
#38698=CARTESIAN_POINT('Ctrl Pts',(-33.5138652990546,30.7407991101668,42.5558170490762));
#38699=CARTESIAN_POINT('Ctrl Pts',(-31.7632531003825,30.0451791949681,42.6669468382959));
#38700=CARTESIAN_POINT('Ctrl Pts',(-30.2293091244602,31.1385894763683,42.7780766275156));
#38701=CARTESIAN_POINT('Ctrl Pts',(-30.3158822215292,33.0203536330321,42.8892064167354));
#38702=CARTESIAN_POINT('Ctrl Pts',(-31.9437416530102,33.9683010556135,43.000336205955));
#38703=CARTESIAN_POINT('Ctrl Pts',(-33.6230881099971,33.1148807754365,43.1114659951748));
#38704=CARTESIAN_POINT('Ctrl Pts',(-33.8170019321722,31.2411336605529,43.2225957843945));
#38705=CARTESIAN_POINT('Ctrl Pts',(-32.3480152896794,30.0618928098755,43.3337255736143));
#38706=CARTESIAN_POINT('Ctrl Pts',(-30.5605288286001,30.6563866316462,43.444855362834));
#38707=CARTESIAN_POINT('Ctrl Pts',(-30.090430772939,32.4805408423343,43.5559851520537));
#38708=CARTESIAN_POINT('Ctrl Pts',(-31.3679497655855,33.8649092828001,43.6671149412734));
#38709=CARTESIAN_POINT('Ctrl Pts',(-33.2239142784095,33.5425329730427,43.7782447304932));
#38710=CARTESIAN_POINT('Ctrl Pts',(-33.9597657164607,31.8084472137752,43.8893745197128));
#38711=CARTESIAN_POINT('Ctrl Pts',(-32.9020608235662,30.2496684874881,44.0005043089327));
#38712=CARTESIAN_POINT('Ctrl Pts',(-31.0187996473937,30.2927741797298,44.1116340981524));
#38713=CARTESIAN_POINT('Ctrl Pts',(-30.0335223932481,31.8983144286743,44.2227638873721));
#38714=CARTESIAN_POINT('Ctrl Pts',(-30.8479441192419,33.5969162097192,44.3338936765918));
#38715=CARTESIAN_POINT('Ctrl Pts',(-32.7167148937789,33.834037593486,44.4450234658115));
#38716=CARTESIAN_POINT('Ctrl Pts',(-33.9295559699792,32.3926676609928,44.5561532550313));
#38717=CARTESIAN_POINT('Ctrl Pts',(-33.3764883476175,30.5919325434682,44.667283044251));
#38718=CARTESIAN_POINT('Ctrl Pts',(-31.5636735169108,30.0798454923028,44.7784128334707));
#38719=CARTESIAN_POINT('Ctrl Pts',(-30.1501799517637,31.3250630233749,44.8895426226905));
#38720=CARTESIAN_POINT('Ctrl Pts',(-30.4296216342993,33.1879755560667,45.0006724119101));
#38721=CARTESIAN_POINT('Ctrl Pts',(-32.14625656708,33.9636657429052,45.11180220113));
#38722=CARTESIAN_POINT('Ctrl Pts',(-33.7290390757554,32.9422303369048,45.2229319903495));
#38723=CARTESIAN_POINT('Ctrl Pts',(-33.7294237729475,31.0584759446318,45.3340617795694));
#38724=CARTESIAN_POINT('Ctrl Pts',(-32.1470585879579,30.0363941574285,45.4451915687891));
#38725=CARTESIAN_POINT('Ctrl Pts',(-30.4301069780531,30.811383142928,45.5563213580087));
#38726=CARTESIAN_POINT('Ctrl Pts',(-30.1499044370533,32.6741813860068,45.6674511472285));
#38727=CARTESIAN_POINT('Ctrl Pts',(-31.5628892918113,33.9199761358048,45.7785809364482));
#38728=CARTESIAN_POINT('Ctrl Pts',(-33.3759131264354,33.4086295473885,45.889710725668));
#38729=CARTESIAN_POINT('Ctrl Pts',(-33.9297161889023,31.6081204731536,46.0008405148877));
#38730=CARTESIAN_POINT('Ctrl Pts',(-32.7174639221865,30.166255292132,46.1119703041075));
#38731=CARTESIAN_POINT('Ctrl Pts',(-30.8485964544578,30.402613381618,46.2231000933272));
#38732=CARTESIAN_POINT('Ctrl Pts',(-30.0334810251578,32.1008823813106,46.3342298825468));
#38733=CARTESIAN_POINT('Ctrl Pts',(-31.0181024356232,33.7068249196517,46.4453596717667));
#38734=CARTESIAN_POINT('Ctrl Pts',(-32.9013458487704,33.750699801273,46.5564894609863));
#38735=CARTESIAN_POINT('Ctrl Pts',(-33.9596873158118,32.192353210318,46.6676192502061));
#38736=CARTESIAN_POINT('Ctrl Pts',(-33.2245442033461,30.4579670472637,46.7787490394257));
#38737=CARTESIAN_POINT('Ctrl Pts',(-31.3687115156069,30.1348327199026,46.8898788286456));
#38738=CARTESIAN_POINT('Ctrl Pts',(-30.0906272027459,31.5186792603898,47.0010086178652));
#38739=CARTESIAN_POINT('Ctrl Pts',(-30.5599801676459,33.3430253220621,47.112138407085));
#38740=CARTESIAN_POINT('Ctrl Pts',(-32.3472236667517,33.9382491734864,47.2232681963047));
#38741=CARTESIAN_POINT('Ctrl Pts',(-33.8166918315301,32.7596084007729,47.3343979855245));
#38742=CARTESIAN_POINT('Ctrl Pts',(-33.6235433332948,30.8857822572822,47.4455277747441));
#38743=CARTESIAN_POINT('Ctrl Pts',(-31.9445455830223,30.0316761087385,47.5566575639639));
#38744=CARTESIAN_POINT('Ctrl Pts',(-30.3162991137898,30.9789586398936,47.6677873531836));
#38745=CARTESIAN_POINT('Ctrl Pts',(-30.228957436641,32.8606871510856,47.7789171424033));
#38746=CARTESIAN_POINT('Ctrl Pts',(-31.7624547073216,33.9547241153676,47.890046931623));
#38747=CARTESIAN_POINT('Ctrl Pts',(-33.51335085379,33.2598187673654,48.0011767208428));
#38748=CARTESIAN_POINT('Ctrl Pts',(-33.8792447104765,31.4119409456361,48.1123065100625));
#38749=CARTESIAN_POINT('Ctrl Pts',(-32.5252741876951,30.1022483932257,48.2234362992823));
#38750=CARTESIAN_POINT('Ctrl Pts',(-30.6905784246966,30.529357531076,48.3345660885019));
#38751=CARTESIAN_POINT('Ctrl Pts',(-30.05425108733,32.302382708032,48.4456958777217));
#38752=CARTESIAN_POINT('Ctrl Pts',(-31.1986520540708,33.7986705098011,48.5568256669414));
#38753=CARTESIAN_POINT('Ctrl Pts',(-33.0764379706693,33.6488345667696,48.6679554561611));
#38754=CARTESIAN_POINT('Ctrl Pts',(-33.969079529995,31.9900031090969,48.7790852453809));
#38755=CARTESIAN_POINT('Ctrl Pts',(-33.0596408572476,30.3403206975669,48.8902150346006));
#38756=CARTESIAN_POINT('Ctrl Pts',(-31.1804303632738,30.2095587851511,49.0013448238203));
#38757=CARTESIAN_POINT('Ctrl Pts',(-30.0512811129692,31.7173892560386,49.1124746130401));
#38758=CARTESIAN_POINT('Ctrl Pts',(-30.7055782550989,33.4838620150136,49.2236044022597));
#38759=CARTESIAN_POINT('Ctrl Pts',(-32.5445161407428,33.8923203496617,49.3347341914795));
#38760=CARTESIAN_POINT('Ctrl Pts',(-33.8851187594106,32.568947621659,49.4458639806992));
#38761=CARTESIAN_POINT('Ctrl Pts',(-33.5004811327274,30.7248802002941,49.556993769919));
#38762=CARTESIAN_POINT('Ctrl Pts',(-31.7426194454125,30.0477885915216,49.6681235591387));
#38763=CARTESIAN_POINT('Ctrl Pts',(-30.2203096504801,31.1573396929374,49.7792533483584));
#38764=CARTESIAN_POINT('Ctrl Pts',(-30.3267531634902,33.0380843691064,49.8903831375782));
#38765=CARTESIAN_POINT('Ctrl Pts',(-31.9645340356676,33.9687854882254,50.0015129267979));
#38766=CARTESIAN_POINT('Ctrl Pts',(-33.6347729737898,33.0976754791102,50.1126427160176));
#38767=CARTESIAN_POINT('Ctrl Pts',(-33.808885414674,31.2219847753081,50.2237725052373));
#38768=CARTESIAN_POINT('Ctrl Pts',(-32.3275255405944,30.0583251679204,50.334902294457));
#38769=CARTESIAN_POINT('Ctrl Pts',(-30.5464178436287,30.6716653102649,50.4460320836768));
#38770=CARTESIAN_POINT('Ctrl Pts',(-30.0956127727332,32.5006829554657,50.5571618728965));
#38771=CARTESIAN_POINT('Ctrl Pts',(-31.3876822400103,33.8714809895036,50.6682916621163));
#38772=CARTESIAN_POINT('Ctrl Pts',(-33.2401382809253,33.5295199173165,50.7794214513359));
#38773=CARTESIAN_POINT('Ctrl Pts',(-33.9576332158673,31.7877588037492,50.8905512405557));
#38774=CARTESIAN_POINT('Ctrl Pts',(-32.8835234613151,30.2402385313405,51.0016810297754));
#38775=CARTESIAN_POINT('Ctrl Pts',(-31.0008226163421,30.3032328712111,51.1128108189951));
#38776=CARTESIAN_POINT('Ctrl Pts',(-30.0325580773407,31.9190900867144,51.2239406082148));
#38777=CARTESIAN_POINT('Ctrl Pts',(-30.8648750497888,33.6089951773492,51.3350703974346));
#38778=CARTESIAN_POINT('Ctrl Pts',(-32.7360460670478,33.8263653306506,51.4462001866543));
#38779=CARTESIAN_POINT('Ctrl Pts',(-33.9335957052477,32.37226573915,51.557329975874));
#38780=CARTESIAN_POINT('Ctrl Pts',(-33.3615395241336,30.5774725808226,51.6684597650938));
#38781=CARTESIAN_POINT('Ctrl Pts',(-31.5434171335246,30.0845610886922,51.7795895543134));
#38782=CARTESIAN_POINT('Ctrl Pts',(-30.1431544354102,31.3446385184301,51.8907193435332));
#38783=CARTESIAN_POINT('Ctrl Pts',(-30.4422566523871,33.2044956644301,52.0018491327529));
#38784=CARTESIAN_POINT('Ctrl Pts',(-32.1669887058313,33.9620114496039,52.1129789219727));
#38785=CARTESIAN_POINT('Ctrl Pts',(-33.7388944714699,32.9239156153169,52.2241087111924));
#38786=CARTESIAN_POINT('Ctrl Pts',(-33.7193829439153,31.040262264795,52.3352385004122));
#38787=CARTESIAN_POINT('Ctrl Pts',(-32.1263106543069,30.0349504114267,52.4463682896318));
#38788=CARTESIAN_POINT('Ctrl Pts',(-30.4176404962616,30.8280307703727,52.5574980788516));
#38789=CARTESIAN_POINT('Ctrl Pts',(-30.1571280564506,32.693684383792,52.6686278680713));
#38790=CARTESIAN_POINT('Ctrl Pts',(-31.5831931024171,33.9244861162258,52.7797576572911));
#38791=CARTESIAN_POINT('Ctrl Pts',(-33.3907131865728,33.3940179477067,52.8908874465107));
#38792=CARTESIAN_POINT('Ctrl Pts',(-33.9254718294467,31.587761803966,53.0020172357305));
#38793=CARTESIAN_POINT('Ctrl Pts',(-32.6980512499253,30.1587773644109,53.1131470249502));
#38794=CARTESIAN_POINT('Ctrl Pts',(-30.8317981364649,30.4148682716697,53.2242768141699));
#38795=CARTESIAN_POINT('Ctrl Pts',(-30.034638236465,32.1216380022259,53.3354066033897));
#38796=CARTESIAN_POINT('Ctrl Pts',(-31.036220369854,33.7171187017325,53.4465363926093));
#38797=CARTESIAN_POINT('Ctrl Pts',(-32.9197159652556,33.7410461592535,53.5576661818291));
#38798=CARTESIAN_POINT('Ctrl Pts',(-33.961749285671,32.1717153833919,53.6687959710488));
#38799=CARTESIAN_POINT('Ctrl Pts',(-33.2079124381607,30.4449784545928,53.7799257602686));
#38800=CARTESIAN_POINT('Ctrl Pts',(-31.3495946744271,30.1418841716374,53.8910555494884));
#38801=CARTESIAN_POINT('Ctrl Pts',(-30.0845579647649,31.5383103207979,54.0021853387079));
#38802=CARTESIAN_POINT('Ctrl Pts',(-30.5764960375974,33.359377212299,54.1133151279278));
#38803=CARTESIAN_POINT('Ctrl Pts',(-31.7668777668624,33.7401334029927,54.1874016540742));
#38804=CARTESIAN_POINT('Ctrl Pts',(-32.3110796379505,33.6366995627948,54.2244449171475));
#38805=CARTESIAN_POINT('Ctrl Pts',(-33.3677806246589,33.1633123698097,40.9251850276175));
#38806=CARTESIAN_POINT('Ctrl Pts',(-33.7545814662436,32.7085259251269,40.9622282906908));
#38807=CARTESIAN_POINT('Ctrl Pts',(-34.0319373921236,31.3903858817126,41.0363148168372));
#38808=CARTESIAN_POINT('Ctrl Pts',(-32.5877567267128,29.9594098734121,41.147444606057));
#38809=CARTESIAN_POINT('Ctrl Pts',(-30.6055202467562,30.4008142160622,41.2585743952767));
#38810=CARTESIAN_POINT('Ctrl Pts',(-29.8995985779794,32.3034005478518,41.3697041844964));
#38811=CARTESIAN_POINT('Ctrl Pts',(-31.1158875333191,33.9295115308857,41.4808339737162));
#38812=CARTESIAN_POINT('Ctrl Pts',(-33.1413341001019,33.7891520709486,41.5919637629358));
#38813=CARTESIAN_POINT('Ctrl Pts',(-34.1222301817997,32.0116843221782,41.7030935521556));
#38814=CARTESIAN_POINT('Ctrl Pts',(-33.160891236097,30.2233694933969,41.8142233413753));
#38815=CARTESIAN_POINT('Ctrl Pts',(-31.1371136737856,30.0610852912993,41.9253531305951));
#38816=CARTESIAN_POINT('Ctrl Pts',(-29.9030421113392,31.6732355746631,42.0364829198147));
#38817=CARTESIAN_POINT('Ctrl Pts',(-30.5880827628849,33.5844569344168,42.1476127090346));
#38818=CARTESIAN_POINT('Ctrl Pts',(-32.5652952154986,34.0455904788454,42.2587424982542));
#38819=CARTESIAN_POINT('Ctrl Pts',(-34.0251553862571,32.6346268582552,42.369872287474));
#38820=CARTESIAN_POINT('Ctrl Pts',(-33.6316154261069,30.6428570641638,42.4810020766937));
#38821=CARTESIAN_POINT('Ctrl Pts',(-31.7448386631624,29.8931310581221,42.5921318659134));
#38822=CARTESIAN_POINT('Ctrl Pts',(-30.0915828183645,31.0715880075684,42.7032616551331));
#38823=CARTESIAN_POINT('Ctrl Pts',(-30.1848896672314,33.0997178736966,42.8143914443529));
#38824=CARTESIAN_POINT('Ctrl Pts',(-31.9393658161969,34.1213977013457,42.9255212335726));
#38825=CARTESIAN_POINT('Ctrl Pts',(-33.749333708789,33.2015974423935,43.0366510227923));
#38826=CARTESIAN_POINT('Ctrl Pts',(-33.9583303637712,31.1821081924737,43.147780812012));
#38827=CARTESIAN_POINT('Ctrl Pts',(-32.3750843060586,29.9111446765901,43.2589106012318));
#38828=CARTESIAN_POINT('Ctrl Pts',(-30.4485651595561,30.5518788891597,43.3700403904515));
#38829=CARTESIAN_POINT('Ctrl Pts',(-29.9419023541675,32.5179178436264,43.4811701796712));
#38830=CARTESIAN_POINT('Ctrl Pts',(-31.3187881952316,34.0099640014252,43.592299968891));
#38831=CARTESIAN_POINT('Ctrl Pts',(-33.3191116925215,33.6625129036691,43.7034297581106));
#38832=CARTESIAN_POINT('Ctrl Pts',(-34.1121984740185,31.7935480249707,43.8145595473304));
#38833=CARTESIAN_POINT('Ctrl Pts',(-32.9722241179162,30.1135257552974,43.9256893365501));
#38834=CARTESIAN_POINT('Ctrl Pts',(-30.9424807924367,30.1599842562344,44.0368191257698));
#38835=CARTESIAN_POINT('Ctrl Pts',(-29.8805675773967,31.8904052118169,44.1479489149896));
#38836=CARTESIAN_POINT('Ctrl Pts',(-30.7583359312378,33.7211261289926,44.2590787042093));
#38837=CARTESIAN_POINT('Ctrl Pts',(-32.7724617755229,33.9766910777731,44.3702084934291));
#38838=CARTESIAN_POINT('Ctrl Pts',(-34.0796389798491,32.4232097884861,44.4813382826487));
#38839=CARTESIAN_POINT('Ctrl Pts',(-33.4835531425627,30.4824114903015,44.5924680718685));
#38840=CARTESIAN_POINT('Ctrl Pts',(-31.529735557667,29.9304937386279,44.7035978610882));
#38841=CARTESIAN_POINT('Ctrl Pts',(-30.0062988905888,31.2725656745027,44.814727650308));
#38842=CARTESIAN_POINT('Ctrl Pts',(-30.3074758580556,33.2803776163751,44.9258574395276));
#38843=CARTESIAN_POINT('Ctrl Pts',(-32.1576325655698,34.1164018488584,45.0369872287475));
#38844=CARTESIAN_POINT('Ctrl Pts',(-33.8635256585285,33.0155180606887,45.148117017967));
#38845=CARTESIAN_POINT('Ctrl Pts',(-33.8639402778962,30.9852431562115,45.259246807187));
#38846=CARTESIAN_POINT('Ctrl Pts',(-32.1584969685238,29.8836627105899,45.3703765964065));
#38847=CARTESIAN_POINT('Ctrl Pts',(-30.3079989523865,30.718931201514,45.4815063856263));
#38848=CARTESIAN_POINT('Ctrl Pts',(-30.0060019460378,32.7266199642001,45.592636174846));
#38849=CARTESIAN_POINT('Ctrl Pts',(-31.5288903346668,34.0693140155155,45.7037659640658));
#38850=CARTESIAN_POINT('Ctrl Pts',(-33.4829331800372,33.5181943206072,45.8148957532854));
#38851=CARTESIAN_POINT('Ctrl Pts',(-34.0798116607782,31.577639647611,45.9260255425052));
#38852=CARTESIAN_POINT('Ctrl Pts',(-32.7732690641933,30.0236245888139,46.0371553317249));
#38853=CARTESIAN_POINT('Ctrl Pts',(-30.7590390058124,30.2783668734355,46.1482851209447));
#38854=CARTESIAN_POINT('Ctrl Pts',(-29.8805229916505,32.108729125155,46.2594149101643));
#38855=CARTESIAN_POINT('Ctrl Pts',(-30.9417293507589,33.839583660651,46.3705446993842));
#38856=CARTESIAN_POINT('Ctrl Pts',(-32.9714535315855,33.8868711793732,46.4816744886038));
#38857=CARTESIAN_POINT('Ctrl Pts',(-34.1121139752799,32.207314656999,46.5928042778236));
#38858=CARTESIAN_POINT('Ctrl Pts',(-33.3197906137204,30.3380260087731,46.7039340670433));
#38859=CARTESIAN_POINT('Ctrl Pts',(-31.3196091950172,29.9897579339606,46.8150638562631));
#38860=CARTESIAN_POINT('Ctrl Pts',(-29.9421140625033,31.4812415978201,46.9261936454828));
#38861=CARTESIAN_POINT('Ctrl Pts',(-30.4479738231426,33.4474873256539,47.0373234347025));
#38862=CARTESIAN_POINT('Ctrl Pts',(-32.3742311098188,34.0890083503957,47.1484532239222));
#38863=CARTESIAN_POINT('Ctrl Pts',(-33.9579961431562,32.8186915872076,47.259583013142));
#38864=CARTESIAN_POINT('Ctrl Pts',(-33.7498243398611,30.7991171617476,47.3707128023616));
#38865=CARTESIAN_POINT('Ctrl Pts',(-31.9402322767798,29.8785776868242,47.4818425915814));
#38866=CARTESIAN_POINT('Ctrl Pts',(-30.1853389858357,30.8995409070522,47.5929723808011));
#38867=CARTESIAN_POINT('Ctrl Pts',(-30.0912037758755,32.9276323551642,47.7041021700208));
#38868=CARTESIAN_POINT('Ctrl Pts',(-31.743978170201,34.1067647315839,47.8152319592406));
#38869=CARTESIAN_POINT('Ctrl Pts',(-33.6310609667174,33.3578088725702,47.9263617484603));
#38870=CARTESIAN_POINT('Ctrl Pts',(-34.0254144546136,31.3662010582043,48.03749153768));
#38871=CARTESIAN_POINT('Ctrl Pts',(-32.5661305983527,29.9546391621066,48.1486213268998));
#38872=CARTESIAN_POINT('Ctrl Pts',(-30.58873015791,30.4149693238342,48.2597511161195));
#38873=CARTESIAN_POINT('Ctrl Pts',(-29.9029085723639,32.3259023714469,48.3708809053392));
#38874=CARTESIAN_POINT('Ctrl Pts',(-31.1363223193809,33.9385731029754,48.4820106945589));
#38875=CARTESIAN_POINT('Ctrl Pts',(-33.160164513506,33.7770827536107,48.5931404837786));
#38876=CARTESIAN_POINT('Ctrl Pts',(-34.1222367263307,31.9892255398015,48.7042702729984));
#38877=CARTESIAN_POINT('Ctrl Pts',(-33.1420609019164,30.2112289951218,48.8154000622181));
#38878=CARTESIAN_POINT('Ctrl Pts',(-31.1166833252031,30.0702962756928,48.9265298514378));
#38879=CARTESIAN_POINT('Ctrl Pts',(-29.8997075900934,31.6954074779844,49.0376596406576));
#38880=CARTESIAN_POINT('Ctrl Pts',(-30.6048966918075,33.5992784532562,49.1487894298772));
#38881=CARTESIAN_POINT('Ctrl Pts',(-32.586869211914,34.0395071315606,49.259919219097));
#38882=CARTESIAN_POINT('Ctrl Pts',(-34.0317453936084,32.6132010005946,49.3710490083167));
#38883=CARTESIAN_POINT('Ctrl Pts',(-33.6171902244337,30.6256999637723,49.4821787975365));
#38884=CARTESIAN_POINT('Ctrl Pts',(-31.7226000995549,29.8959434164423,49.5933085867562));
#38885=CARTESIAN_POINT('Ctrl Pts',(-30.0818833552869,31.0917966368408,49.7044383759759));
#38886=CARTESIAN_POINT('Ctrl Pts',(-30.1966061631514,33.1188277261472,49.8155681651957));
#38887=CARTESIAN_POINT('Ctrl Pts',(-31.961775453508,34.1219198136651,49.9266979544153));
#38888=CARTESIAN_POINT('Ctrl Pts',(-33.7619274342862,33.183053898979,50.0378277436351));
#38889=CARTESIAN_POINT('Ctrl Pts',(-33.9495825345129,31.1614698856324,50.1489575328548));
#38890=CARTESIAN_POINT('Ctrl Pts',(-32.353000841496,29.9072995394748,50.2600873220746));
#38891=CARTESIAN_POINT('Ctrl Pts',(-30.433356606476,30.5683459603981,50.3712171112943));
#38892=CARTESIAN_POINT('Ctrl Pts',(-29.9474874156704,32.539626632724,50.482346900514));
#38893=CARTESIAN_POINT('Ctrl Pts',(-31.3400554834685,34.0170468627869,50.5934766897337));
#38894=CARTESIAN_POINT('Ctrl Pts',(-33.3365976160012,33.6484876779921,50.7046064789535));
#38895=CARTESIAN_POINT('Ctrl Pts',(-34.1099001051568,31.7712504473981,50.8157362681732));
#38896=CARTESIAN_POINT('Ctrl Pts',(-32.9522448990074,30.1033623266704,50.9268660573929));
#38897=CARTESIAN_POINT('Ctrl Pts',(-30.9231054879113,30.1712564363739,51.0379958466126));
#38898=CARTESIAN_POINT('Ctrl Pts',(-29.8795282559254,31.9127968236512,51.1491256358324));
#38899=CARTESIAN_POINT('Ctrl Pts',(-30.7765837683972,33.7341446121621,51.2602554250521));
#38900=CARTESIAN_POINT('Ctrl Pts',(-32.7932965489535,33.9684220577994,51.3713852142719));
#38901=CARTESIAN_POINT('Ctrl Pts',(-34.0839929302207,32.4012209824662,51.4825150034915));
#38902=CARTESIAN_POINT('Ctrl Pts',(-33.4674415829586,30.4668268156755,51.5936447927113));
#38903=CARTESIAN_POINT('Ctrl Pts',(-31.5079036102468,29.9355761193503,51.7047745819309));
#38904=CARTESIAN_POINT('Ctrl Pts',(-29.9987269217578,31.29366377334,51.8159043711508));
#38905=CARTESIAN_POINT('Ctrl Pts',(-30.321093641906,33.2981826771447,51.9270341603704));
#38906=CARTESIAN_POINT('Ctrl Pts',(-32.1799772731366,34.1146188827839,52.0381639495902));
#38907=CARTESIAN_POINT('Ctrl Pts',(-33.8741476178852,32.9957787996815,52.1492937388098));
#38908=CARTESIAN_POINT('Ctrl Pts',(-33.853118462012,30.9656127960953,52.2604235280297));
#38909=CARTESIAN_POINT('Ctrl Pts',(-32.1361352375125,29.882106668418,52.3715533172493));
#38910=CARTESIAN_POINT('Ctrl Pts',(-30.294562813773,30.736873699941,52.4826831064691));
#38911=CARTESIAN_POINT('Ctrl Pts',(-30.0137874265877,32.7476399268491,52.5938128956888));
#38912=CARTESIAN_POINT('Ctrl Pts',(-31.5507733982484,34.0741747872307,52.7049426849085));
#38913=CARTESIAN_POINT('Ctrl Pts',(-33.4988844053163,33.5024462144477,52.8160724741283));
#38914=CARTESIAN_POINT('Ctrl Pts',(-34.0752371703226,31.5556974584861,52.927202263348));
#38915=CARTESIAN_POINT('Ctrl Pts',(-32.7523464526881,30.0155650195559,53.0383320525678));
#38916=CARTESIAN_POINT('Ctrl Pts',(-30.7409340959589,30.2915749624683,53.1494618417874));
#38917=CARTESIAN_POINT('Ctrl Pts',(-29.8817702121404,32.1310991413546,53.2605916310072));
#38918=CARTESIAN_POINT('Ctrl Pts',(-30.9612565180695,33.8506781045533,53.3717214202268));
#38919=CARTESIAN_POINT('Ctrl Pts',(-32.9912524961666,33.8764666663383,53.4828512094467));
#38920=CARTESIAN_POINT('Ctrl Pts',(-34.1143363274486,32.185071596936,53.5939809986663));
#38921=CARTESIAN_POINT('Ctrl Pts',(-33.301865211337,30.3240271489152,53.7051107878861));
#38922=CARTESIAN_POINT('Ctrl Pts',(-31.2990054246639,29.9973578554558,53.8162405771058));
#38923=CARTESIAN_POINT('Ctrl Pts',(-29.9355727524405,31.5023995839451,53.9273703663255));
#38924=CARTESIAN_POINT('Ctrl Pts',(-30.4657743158319,33.465111084104,54.0385001555453));
#38925=CARTESIAN_POINT('Ctrl Pts',(-31.7487452602333,33.8754829148801,54.1125866816917));
#38926=CARTESIAN_POINT('Ctrl Pts',(-32.3352757582493,33.7640038755272,54.149629944765));
#38927=CARTESIAN_POINT('Ctrl Pts',(-33.4664903694653,33.2472660865709,40.850370055235));
#38928=CARTESIAN_POINT('Ctrl Pts',(-33.8812057842465,32.75965869598,40.8874133183083));
#38929=CARTESIAN_POINT('Ctrl Pts',(-34.1785778824356,31.3463913602508,40.9614998444547));
#38930=CARTESIAN_POINT('Ctrl Pts',(-32.6301738478915,29.8121449341238,41.0726296336745));
#38931=CARTESIAN_POINT('Ctrl Pts',(-30.5048836840657,30.2854044655623,41.1837594228942));
#38932=CARTESIAN_POINT('Ctrl Pts',(-29.7480171879371,32.3252963037301,41.294889212114));
#38933=CARTESIAN_POINT('Ctrl Pts',(-31.0520830646837,34.0687601701639,41.4060190013336));
#38934=CARTESIAN_POINT('Ctrl Pts',(-33.2237016930687,33.918271274101,41.5171487905534));
#38935=CARTESIAN_POINT('Ctrl Pts',(-34.2753869058308,32.0125275542285,41.6282785797731));
#38936=CARTESIAN_POINT('Ctrl Pts',(-33.2446702249182,30.095153944236,41.7394083689928));
#38937=CARTESIAN_POINT('Ctrl Pts',(-31.0748410494174,29.9211580451847,41.8505381582126));
#38938=CARTESIAN_POINT('Ctrl Pts',(-29.7517092335898,31.649653698699,41.9616679474322));
#38939=CARTESIAN_POINT('Ctrl Pts',(-30.4861877750113,33.6988037359677,42.0727977366521));
#38940=CARTESIAN_POINT('Ctrl Pts',(-32.6060913383974,34.1932162826512,42.1839275258717));
#38941=CARTESIAN_POINT('Ctrl Pts',(-34.171306433996,32.6804264946123,42.2950573150915));
#38942=CARTESIAN_POINT('Ctrl Pts',(-33.7493655531593,30.544915018161,42.4061871043112));
#38943=CARTESIAN_POINT('Ctrl Pts',(-31.7264242259422,29.7410829212761,42.5173168935309));
#38944=CARTESIAN_POINT('Ctrl Pts',(-29.9538565122688,31.0045865387686,42.6284466827506));
#38945=CARTESIAN_POINT('Ctrl Pts',(-30.0538971129336,33.1790821143611,42.7395764719704));
#38946=CARTESIAN_POINT('Ctrl Pts',(-31.9349899793838,34.2744943470779,42.8507062611901));
#38947=CARTESIAN_POINT('Ctrl Pts',(-33.8755793075807,33.2883141093505,42.9618360504098));
#38948=CARTESIAN_POINT('Ctrl Pts',(-34.0996587953703,31.1230827243945,43.0729658396296));
#38949=CARTESIAN_POINT('Ctrl Pts',(-32.4021533224376,29.7603965433046,43.1840956288492));
#38950=CARTESIAN_POINT('Ctrl Pts',(-30.3366014905122,30.4473711466732,43.2952254180691));
#38951=CARTESIAN_POINT('Ctrl Pts',(-29.793373935396,32.5552948449183,43.4063552072887));
#38952=CARTESIAN_POINT('Ctrl Pts',(-31.2696266248778,34.1550187200504,43.5174849965085));
#38953=CARTESIAN_POINT('Ctrl Pts',(-33.4143091066335,33.7824928342954,43.6286147857282));
#38954=CARTESIAN_POINT('Ctrl Pts',(-34.2646312315764,31.7786488361662,43.7397445749479));
#38955=CARTESIAN_POINT('Ctrl Pts',(-33.0423874122662,29.9773830231067,43.8508743641677));
#38956=CARTESIAN_POINT('Ctrl Pts',(-30.8661619374796,30.027194332739,43.9620041533873));
#38957=CARTESIAN_POINT('Ctrl Pts',(-29.7276127615454,31.8824959949596,44.0731339426071));
#38958=CARTESIAN_POINT('Ctrl Pts',(-30.6687277432337,33.845336048266,44.1842637318268));
#38959=CARTESIAN_POINT('Ctrl Pts',(-32.8282086572669,34.1193445620604,44.2953935210466));
#38960=CARTESIAN_POINT('Ctrl Pts',(-34.2297219897189,32.4537519159793,44.4065233102662));
#38961=CARTESIAN_POINT('Ctrl Pts',(-33.590617937508,30.3728904371349,44.517653099486));
#38962=CARTESIAN_POINT('Ctrl Pts',(-31.4957975984231,29.781141984953,44.6287828887056));
#38963=CARTESIAN_POINT('Ctrl Pts',(-29.862417829414,31.2200683256305,44.7399126779256));
#38964=CARTESIAN_POINT('Ctrl Pts',(-30.1853300818118,33.3727796766834,44.8510424671451));
#38965=CARTESIAN_POINT('Ctrl Pts',(-32.1690085640597,34.2691379548117,44.962172256365));
#38966=CARTESIAN_POINT('Ctrl Pts',(-33.9980122413016,33.0888057844725,45.0733020455846));
#38967=CARTESIAN_POINT('Ctrl Pts',(-33.9984567828449,30.9120103677913,45.1844318348044));
#38968=CARTESIAN_POINT('Ctrl Pts',(-32.1699353490897,29.7309312637511,45.295561624024));
#38969=CARTESIAN_POINT('Ctrl Pts',(-30.1858909267199,30.6264792601002,45.4066914132438));
#38970=CARTESIAN_POINT('Ctrl Pts',(-29.8620994550223,32.7790585423934,45.5178212024635));
#38971=CARTESIAN_POINT('Ctrl Pts',(-31.4948913775223,34.2186518952262,45.6289509916833));
#38972=CARTESIAN_POINT('Ctrl Pts',(-33.589953233639,33.627759093826,45.740080780903));
#38973=CARTESIAN_POINT('Ctrl Pts',(-34.2299071326541,31.5471588220685,45.8512105701227));
#38974=CARTESIAN_POINT('Ctrl Pts',(-32.8290742062001,29.8809938854959,45.9623403593424));
#38975=CARTESIAN_POINT('Ctrl Pts',(-30.6694815571671,30.154120365253,46.0734701485622));
#38976=CARTESIAN_POINT('Ctrl Pts',(-29.7275649581431,32.1165758689995,46.1845999377818));
#38977=CARTESIAN_POINT('Ctrl Pts',(-30.8653562658947,33.9723424016504,46.2957297270017));
#38978=CARTESIAN_POINT('Ctrl Pts',(-33.0415612144005,34.0230425574734,46.4068595162213));
#38979=CARTESIAN_POINT('Ctrl Pts',(-34.2645406347481,32.2222761036798,46.5179893054411));
#38980=CARTESIAN_POINT('Ctrl Pts',(-33.4150370240947,30.2180849702824,46.6291190946608));
#38981=CARTESIAN_POINT('Ctrl Pts',(-31.2705068744274,29.8446831480187,46.7402488838805));
#38982=CARTESIAN_POINT('Ctrl Pts',(-29.7936009222607,31.4438039352503,46.8513786731003));
#38983=CARTESIAN_POINT('Ctrl Pts',(-30.3359674786392,33.5519493292456,46.96250846232));
#38984=CARTESIAN_POINT('Ctrl Pts',(-32.401238552886,34.2397675273051,47.0736382515397));
#38985=CARTESIAN_POINT('Ctrl Pts',(-34.0993004547824,32.8777747736423,47.1847680407595));
#38986=CARTESIAN_POINT('Ctrl Pts',(-33.8761053464274,30.7124520662131,47.2958978299791));
#38987=CARTESIAN_POINT('Ctrl Pts',(-31.9359189705373,29.7254792649098,47.4070276191989));
#38988=CARTESIAN_POINT('Ctrl Pts',(-30.0543788578817,30.8201231742108,47.5181574084186));
#38989=CARTESIAN_POINT('Ctrl Pts',(-29.95345011511,32.9945775592427,47.6292871976383));
#38990=CARTESIAN_POINT('Ctrl Pts',(-31.7255016330804,34.2588053478002,47.7404169868581));
#38991=CARTESIAN_POINT('Ctrl Pts',(-33.7487710796447,33.4557989777749,47.8515467760777));
#38992=CARTESIAN_POINT('Ctrl Pts',(-34.1715841987509,31.3204611707726,47.9626765652976));
#38993=CARTESIAN_POINT('Ctrl Pts',(-32.6069870090102,29.8070299309874,48.0738063545172));
#38994=CARTESIAN_POINT('Ctrl Pts',(-30.4868818911235,30.3005811165925,48.184936143737));
#38995=CARTESIAN_POINT('Ctrl Pts',(-29.7515660573979,32.3494220348617,48.2960659329567));
#38996=CARTESIAN_POINT('Ctrl Pts',(-31.073992584691,34.0784756961497,48.4071957221765));
#38997=CARTESIAN_POINT('Ctrl Pts',(-33.2438910563427,33.9053309404518,48.5183255113961));
#38998=CARTESIAN_POINT('Ctrl Pts',(-34.2753939226663,31.988447970506,48.6294553006159));
#38999=CARTESIAN_POINT('Ctrl Pts',(-33.2244809465853,30.0821372926766,48.7405850898356));
#39000=CARTESIAN_POINT('Ctrl Pts',(-31.0529362871324,29.9310337662346,48.8517148790553));
#39001=CARTESIAN_POINT('Ctrl Pts',(-29.7481340672176,31.6734256999301,48.9628446682751));
#39002=CARTESIAN_POINT('Ctrl Pts',(-30.5042151285161,33.7146948914988,49.0739744574948));
#39003=CARTESIAN_POINT('Ctrl Pts',(-32.6292222830852,34.1866939134596,49.1851042467145));
#39004=CARTESIAN_POINT('Ctrl Pts',(-34.1783720278063,32.6574543795302,49.2962340359342));
#39005=CARTESIAN_POINT('Ctrl Pts',(-33.7338993161399,30.5265197272506,49.407363825154));
#39006=CARTESIAN_POINT('Ctrl Pts',(-31.7025807536974,29.7440982413631,49.5184936143737));
#39007=CARTESIAN_POINT('Ctrl Pts',(-29.9434570600936,31.0262535807442,49.6296234035934));
#39008=CARTESIAN_POINT('Ctrl Pts',(-30.0664591628126,33.199571083188,49.7407531928132));
#39009=CARTESIAN_POINT('Ctrl Pts',(-31.9590168713483,34.2750541391048,49.8518829820328));
#39010=CARTESIAN_POINT('Ctrl Pts',(-33.8890818947825,33.2684323188477,49.9630127712527));
#39011=CARTESIAN_POINT('Ctrl Pts',(-34.0902796543517,31.1009549959568,50.0741425604723));
#39012=CARTESIAN_POINT('Ctrl Pts',(-32.3784761423976,29.7562739110293,50.1852723496921));
#39013=CARTESIAN_POINT('Ctrl Pts',(-30.3202953693232,30.4650266105312,50.2964021389118));
#39014=CARTESIAN_POINT('Ctrl Pts',(-29.7993620586076,32.5785703099824,50.4075319281315));
#39015=CARTESIAN_POINT('Ctrl Pts',(-31.2924287269267,34.1626127360701,50.5186617173513));
#39016=CARTESIAN_POINT('Ctrl Pts',(-33.4330569510772,33.7674554386677,50.629791506571));
#39017=CARTESIAN_POINT('Ctrl Pts',(-34.2621669944462,31.7547420910471,50.7409212957907));
#39018=CARTESIAN_POINT('Ctrl Pts',(-33.0209663366997,29.9664861220002,50.8520510850105));
#39019=CARTESIAN_POINT('Ctrl Pts',(-30.8453883594806,30.0392800015366,50.9631808742301));
#39020=CARTESIAN_POINT('Ctrl Pts',(-29.72649843451,31.9065035605881,51.0743106634499));
#39021=CARTESIAN_POINT('Ctrl Pts',(-30.6882924870058,33.8592940469749,51.1854404526696));
#39022=CARTESIAN_POINT('Ctrl Pts',(-32.8505470308592,34.1104787849484,51.2965702418894));
#39023=CARTESIAN_POINT('Ctrl Pts',(-34.2343901551937,32.4301762257824,51.407700031109));
#39024=CARTESIAN_POINT('Ctrl Pts',(-33.5733436417835,30.3561810505284,51.5188298203289));
#39025=CARTESIAN_POINT('Ctrl Pts',(-31.472390086969,29.7865911500084,51.6299596095484));
#39026=CARTESIAN_POINT('Ctrl Pts',(-29.8542994081055,31.2426890282499,51.7410893987682));
#39027=CARTESIAN_POINT('Ctrl Pts',(-30.1999306314249,33.3918696898592,51.852219187988));
#39028=CARTESIAN_POINT('Ctrl Pts',(-32.1929658404419,34.2672263159639,51.9633489772077));
#39029=CARTESIAN_POINT('Ctrl Pts',(-34.0094007643006,33.0676419840461,52.0744787664274));
#39030=CARTESIAN_POINT('Ctrl Pts',(-33.9868539801086,30.8909633273957,52.1856085556472));
#39031=CARTESIAN_POINT('Ctrl Pts',(-32.1459598207181,29.7292629254092,52.2967383448669));
#39032=CARTESIAN_POINT('Ctrl Pts',(-30.1714851312844,30.6457166295093,52.4078681340866));
#39033=CARTESIAN_POINT('Ctrl Pts',(-29.8704467967248,32.8015954699061,52.5189979233063));
#39034=CARTESIAN_POINT('Ctrl Pts',(-31.5183536940796,34.2238634582357,52.630127712526));
#39035=CARTESIAN_POINT('Ctrl Pts',(-33.6070556240599,33.6108744811885,52.7412575017458));
#39036=CARTESIAN_POINT('Ctrl Pts',(-34.2250025111984,31.5236331130063,52.8523872909654));
#39037=CARTESIAN_POINT('Ctrl Pts',(-32.8066416554509,29.8723526747009,52.9635170801853));
#39038=CARTESIAN_POINT('Ctrl Pts',(-30.6500700554528,30.168281653267,53.0746468694049));
#39039=CARTESIAN_POINT('Ctrl Pts',(-29.7289021878159,32.1405602804833,53.1857766586248));
#39040=CARTESIAN_POINT('Ctrl Pts',(-30.8862926662849,33.9842375073741,53.2969064478443));
#39041=CARTESIAN_POINT('Ctrl Pts',(-33.0627890270775,34.0118871734231,53.4080362370642));
#39042=CARTESIAN_POINT('Ctrl Pts',(-34.2669233692262,32.1984278104801,53.5191660262838));
#39043=CARTESIAN_POINT('Ctrl Pts',(-33.3958179845133,30.2030758432375,53.6302958155037));
#39044=CARTESIAN_POINT('Ctrl Pts',(-31.2484161749007,29.8528315392741,53.7414256047233));
#39045=CARTESIAN_POINT('Ctrl Pts',(-29.786587540116,31.4664888470924,53.8525553939431));
#39046=CARTESIAN_POINT('Ctrl Pts',(-30.3550525940664,33.5708449559089,53.9636851831627));
#39047=CARTESIAN_POINT('Ctrl Pts',(-31.7306127536042,34.0108324267675,54.0377717093093));
#39048=CARTESIAN_POINT('Ctrl Pts',(-32.359471878548,33.8913081882596,54.0748149723825));
#39049=CARTESIAN_POINT('Ctrl Pts',(-33.5652001142718,33.3312198033321,40.7755550828525));
#39050=CARTESIAN_POINT('Ctrl Pts',(-34.0078301022494,32.8107914668331,40.8125983459258));
#39051=CARTESIAN_POINT('Ctrl Pts',(-34.3252183727475,31.3023968387891,40.8866848720723));
#39052=CARTESIAN_POINT('Ctrl Pts',(-32.6725909690703,29.6648799948355,40.997814661292));
#39053=CARTESIAN_POINT('Ctrl Pts',(-30.4042471213751,30.1699947150623,41.1089444505117));
#39054=CARTESIAN_POINT('Ctrl Pts',(-29.5964357978947,32.3471920596084,41.2200742397314));
#39055=CARTESIAN_POINT('Ctrl Pts',(-30.9882785960482,34.2080088094421,41.3312040289512));
#39056=CARTESIAN_POINT('Ctrl Pts',(-33.3060692860357,34.0473904772534,41.4423338181709));
#39057=CARTESIAN_POINT('Ctrl Pts',(-34.4285436298619,32.0133707862788,41.5534636073906));
#39058=CARTESIAN_POINT('Ctrl Pts',(-33.3284492137394,29.9669383950752,41.6645933966104));
#39059=CARTESIAN_POINT('Ctrl Pts',(-31.0125684250491,29.7812307990702,41.7757231858301));
#39060=CARTESIAN_POINT('Ctrl Pts',(-29.6003763558403,31.6260718227349,41.8868529750497));
#39061=CARTESIAN_POINT('Ctrl Pts',(-30.3842927871376,33.8131505375187,41.9979827642696));
#39062=CARTESIAN_POINT('Ctrl Pts',(-32.6468874612962,34.3408420864571,42.1091125534892));
#39063=CARTESIAN_POINT('Ctrl Pts',(-34.3174574817349,32.7262261309694,42.220242342709));
#39064=CARTESIAN_POINT('Ctrl Pts',(-33.8671156802116,30.446972972158,42.3313721319287));
#39065=CARTESIAN_POINT('Ctrl Pts',(-31.708009788722,29.5890347844302,42.4425019211484));
#39066=CARTESIAN_POINT('Ctrl Pts',(-29.8161302061732,30.9375850699686,42.5536317103681));
#39067=CARTESIAN_POINT('Ctrl Pts',(-29.9229045586358,33.2584463550257,42.6647614995879));
#39068=CARTESIAN_POINT('Ctrl Pts',(-31.9306141425706,34.4275909928101,42.7758912888076));
#39069=CARTESIAN_POINT('Ctrl Pts',(-34.0018249063725,33.3750307763075,42.8870210780274));
#39070=CARTESIAN_POINT('Ctrl Pts',(-34.2409872269693,31.0640572563152,42.998150867247));
#39071=CARTESIAN_POINT('Ctrl Pts',(-32.4292223388168,29.6096484100191,43.1092806564668));
#39072=CARTESIAN_POINT('Ctrl Pts',(-30.2246378214682,30.3428634041866,43.2204104456865));
#39073=CARTESIAN_POINT('Ctrl Pts',(-29.6448455166245,32.5926718462104,43.3315402349062));
#39074=CARTESIAN_POINT('Ctrl Pts',(-31.2204650545239,34.3000734386756,43.442670024126));
#39075=CARTESIAN_POINT('Ctrl Pts',(-33.5095065207455,33.9024727649217,43.5537998133457));
#39076=CARTESIAN_POINT('Ctrl Pts',(-34.4170639891342,31.7637496473617,43.6649296025654));
#39077=CARTESIAN_POINT('Ctrl Pts',(-33.1125507066162,29.841240290916,43.7760593917852));
#39078=CARTESIAN_POINT('Ctrl Pts',(-30.7898430825224,29.8944044092436,43.8871891810048));
#39079=CARTESIAN_POINT('Ctrl Pts',(-29.5746579456941,31.8745867781023,43.9983189702246));
#39080=CARTESIAN_POINT('Ctrl Pts',(-30.5791195552295,33.9695459675394,44.1094487594443));
#39081=CARTESIAN_POINT('Ctrl Pts',(-32.883955539011,34.2619980463476,44.2205785486641));
#39082=CARTESIAN_POINT('Ctrl Pts',(-34.3798049995887,32.4842940434725,44.3317083378838));
#39083=CARTESIAN_POINT('Ctrl Pts',(-33.6976827324532,30.2633693839683,44.4428381271035));
#39084=CARTESIAN_POINT('Ctrl Pts',(-31.4618596391792,29.6317902312781,44.5539679163232));
#39085=CARTESIAN_POINT('Ctrl Pts',(-29.7185367682392,31.1675709767584,44.665097705543));
#39086=CARTESIAN_POINT('Ctrl Pts',(-30.0631843055681,33.4651817369917,44.7762274947626));
#39087=CARTESIAN_POINT('Ctrl Pts',(-32.1803845625496,34.421874060765,44.8873572839825));
#39088=CARTESIAN_POINT('Ctrl Pts',(-34.1324988240748,33.1620935082564,44.9984870732021));
#39089=CARTESIAN_POINT('Ctrl Pts',(-34.1329732877935,30.8387775793711,45.109616862422));
#39090=CARTESIAN_POINT('Ctrl Pts',(-32.1813737296557,29.5781998169125,45.2207466516415));
#39091=CARTESIAN_POINT('Ctrl Pts',(-30.0637829010532,30.5340273186863,45.3318764408613));
#39092=CARTESIAN_POINT('Ctrl Pts',(-29.7181969640068,32.8314971205867,45.4430062300811));
#39093=CARTESIAN_POINT('Ctrl Pts',(-31.4608924203777,34.3679897749369,45.5541360193008));
#39094=CARTESIAN_POINT('Ctrl Pts',(-33.6969732872408,33.7373238670447,45.6652658085205));
#39095=CARTESIAN_POINT('Ctrl Pts',(-34.38000260453,31.5166779965259,45.7763955977402));
#39096=CARTESIAN_POINT('Ctrl Pts',(-32.8848793482069,29.7383631821778,45.88752538696));
#39097=CARTESIAN_POINT('Ctrl Pts',(-30.5799241085217,30.0298738570706,45.9986551761797));
#39098=CARTESIAN_POINT('Ctrl Pts',(-29.5746069246357,32.1244226128439,46.1097849653993));
#39099=CARTESIAN_POINT('Ctrl Pts',(-30.7889831810305,34.1051011426497,46.2209147546192));
#39100=CARTESIAN_POINT('Ctrl Pts',(-33.1116688972156,34.1592139355736,46.3320445438388));
#39101=CARTESIAN_POINT('Ctrl Pts',(-34.4169672942162,32.2372375503608,46.4431743330586));
#39102=CARTESIAN_POINT('Ctrl Pts',(-33.510283434469,30.0981439317918,46.5543041222783));
#39103=CARTESIAN_POINT('Ctrl Pts',(-31.2214045538376,29.6996083620767,46.665433911498));
#39104=CARTESIAN_POINT('Ctrl Pts',(-29.645087782018,31.4063662726806,46.7765637007178));
#39105=CARTESIAN_POINT('Ctrl Pts',(-30.223961134136,33.6564113328374,46.8876934899375));
#39106=CARTESIAN_POINT('Ctrl Pts',(-32.4282459959531,34.3905267042144,46.9988232791572));
#39107=CARTESIAN_POINT('Ctrl Pts',(-34.2406047664085,32.9368579600769,47.109953068377));
#39108=CARTESIAN_POINT('Ctrl Pts',(-34.0023863529936,30.6257869706786,47.2210828575967));
#39109=CARTESIAN_POINT('Ctrl Pts',(-31.9316056642948,29.5723808429954,47.3322126468164));
#39110=CARTESIAN_POINT('Ctrl Pts',(-29.9234187299276,30.7407054413694,47.4433424360361));
#39111=CARTESIAN_POINT('Ctrl Pts',(-29.8156964543446,33.0615227633212,47.5544722252558));
#39112=CARTESIAN_POINT('Ctrl Pts',(-31.7070250959598,34.4108459640165,47.6656020144756));
#39113=CARTESIAN_POINT('Ctrl Pts',(-33.8664811925721,33.5537890829796,47.7767318036953));
#39114=CARTESIAN_POINT('Ctrl Pts',(-34.317753942888,31.2747212833408,47.8878615929151));
#39115=CARTESIAN_POINT('Ctrl Pts',(-32.6478434196678,29.6594206998682,47.9989913821348));
#39116=CARTESIAN_POINT('Ctrl Pts',(-30.3850336243369,30.1861929093508,48.1101211713545));
#39117=CARTESIAN_POINT('Ctrl Pts',(-29.6002235424318,32.3729416982765,48.2212509605743));
#39118=CARTESIAN_POINT('Ctrl Pts',(-31.0116628500012,34.2183782893241,48.3323807497939));
#39119=CARTESIAN_POINT('Ctrl Pts',(-33.3276175991793,34.0335791272928,48.4435105390137));
#39120=CARTESIAN_POINT('Ctrl Pts',(-34.4285511190019,31.9876704012107,48.5546403282334));
#39121=CARTESIAN_POINT('Ctrl Pts',(-33.3069009912542,29.9530455902315,48.6657701174531));
#39122=CARTESIAN_POINT('Ctrl Pts',(-30.9891892490617,29.7917712567763,48.7768999066728));
#39123=CARTESIAN_POINT('Ctrl Pts',(-29.5965605443418,31.6514439218759,48.8880296958926));
#39124=CARTESIAN_POINT('Ctrl Pts',(-30.4035335652247,33.8301113297414,48.9991594851123));
#39125=CARTESIAN_POINT('Ctrl Pts',(-32.6715753542565,34.3338806953585,49.110289274332));
#39126=CARTESIAN_POINT('Ctrl Pts',(-34.3249986620041,32.7017077584658,49.2214190635518));
#39127=CARTESIAN_POINT('Ctrl Pts',(-33.8506084078462,30.4273394907288,49.3325488527714));
#39128=CARTESIAN_POINT('Ctrl Pts',(-31.6825614078399,29.5922530662839,49.4436786419912));
#39129=CARTESIAN_POINT('Ctrl Pts',(-29.8050307649004,30.9607105246476,49.554808431211));
#39130=CARTESIAN_POINT('Ctrl Pts',(-29.9363121624739,33.2803144402289,49.6659382204307));
#39131=CARTESIAN_POINT('Ctrl Pts',(-31.9562582891885,34.4281884645445,49.7770680096504));
#39132=CARTESIAN_POINT('Ctrl Pts',(-34.0162363552789,33.3538107387165,49.8881977988702));
#39133=CARTESIAN_POINT('Ctrl Pts',(-34.2309767741905,31.040440106281,49.9993275880898));
#39134=CARTESIAN_POINT('Ctrl Pts',(-32.4039514432991,29.6052482825838,50.1104573773096));
#39135=CARTESIAN_POINT('Ctrl Pts',(-30.2072341321705,30.3617072606643,50.2215871665293));
#39136=CARTESIAN_POINT('Ctrl Pts',(-29.6512367015448,32.6175139872409,50.332716955749));
#39137=CARTESIAN_POINT('Ctrl Pts',(-31.2448019703849,34.3081786093532,50.4438467449688));
#39138=CARTESIAN_POINT('Ctrl Pts',(-33.5295162861532,33.8864231993434,50.5549765341884));
#39139=CARTESIAN_POINT('Ctrl Pts',(-34.4144338837356,31.738233734696,50.6661063234082));
#39140=CARTESIAN_POINT('Ctrl Pts',(-33.0896877743921,29.8296099173301,50.7772361126279));
#39141=CARTESIAN_POINT('Ctrl Pts',(-30.7676712310498,29.9073035666993,50.8883659018476));
#39142=CARTESIAN_POINT('Ctrl Pts',(-29.5734686130947,31.9002102975249,50.9994956910674));
#39143=CARTESIAN_POINT('Ctrl Pts',(-30.6000012056143,33.9844434817877,51.110625480287));
#39144=CARTESIAN_POINT('Ctrl Pts',(-32.907797512765,34.2525355120973,51.2217552695069));
#39145=CARTESIAN_POINT('Ctrl Pts',(-34.3847873801667,32.4591314690988,51.3328850587265));
#39146=CARTESIAN_POINT('Ctrl Pts',(-33.6792457006084,30.2455352853812,51.4440148479464));
#39147=CARTESIAN_POINT('Ctrl Pts',(-31.4368765636913,29.6376061806665,51.5551446371659));
#39148=CARTESIAN_POINT('Ctrl Pts',(-29.7098718944532,31.1917142831597,51.6662744263858));
#39149=CARTESIAN_POINT('Ctrl Pts',(-30.0787676209438,33.4855567025737,51.7774042156054));
#39150=CARTESIAN_POINT('Ctrl Pts',(-32.2059544077473,34.4198337491439,51.8885340048253));
#39151=CARTESIAN_POINT('Ctrl Pts',(-34.1446539107159,33.1395051684107,51.9996637940449));
#39152=CARTESIAN_POINT('Ctrl Pts',(-34.1205894982053,30.816313858696,52.1107935832648));
#39153=CARTESIAN_POINT('Ctrl Pts',(-32.1557844039238,29.5764191824004,52.2219233724843));
#39154=CARTESIAN_POINT('Ctrl Pts',(-30.0484074487957,30.5545595590777,52.3330531617041));
#39155=CARTESIAN_POINT('Ctrl Pts',(-29.7271061668619,32.8555510129632,52.4441829509238));
#39156=CARTESIAN_POINT('Ctrl Pts',(-31.4859339899109,34.3735521292407,52.5553127401435));
#39157=CARTESIAN_POINT('Ctrl Pts',(-33.7152268428034,33.7193027479294,52.6664425293632));
#39158=CARTESIAN_POINT('Ctrl Pts',(-34.3747678520742,31.4915687675265,52.777572318583));
#39159=CARTESIAN_POINT('Ctrl Pts',(-32.8609368582137,29.729140329846,52.8887021078027));
#39160=CARTESIAN_POINT('Ctrl Pts',(-30.5592060149468,30.0449883440656,52.9998318970225));
#39161=CARTESIAN_POINT('Ctrl Pts',(-29.5760341634913,32.150021419612,53.1109616862422));
#39162=CARTESIAN_POINT('Ctrl Pts',(-30.8113288145004,34.117796910195,53.2220914754619));
#39163=CARTESIAN_POINT('Ctrl Pts',(-33.1343255579885,34.1473076805079,53.3332212646816));
#39164=CARTESIAN_POINT('Ctrl Pts',(-34.4195104110039,32.2117840240242,53.4443510539014));
#39165=CARTESIAN_POINT('Ctrl Pts',(-33.4897707576895,30.0821245375598,53.5554808431211));
#39166=CARTESIAN_POINT('Ctrl Pts',(-31.1978269251376,29.7083052230924,53.6666106323408));
#39167=CARTESIAN_POINT('Ctrl Pts',(-29.6376023277916,31.4305781102398,53.7777404215605));
#39168=CARTESIAN_POINT('Ctrl Pts',(-30.2443308723009,33.6765788277138,53.8888702107803));
#39169=CARTESIAN_POINT('Ctrl Pts',(-31.7124802469751,34.146181938655,53.9629567369268));
#39170=CARTESIAN_POINT('Ctrl Pts',(-32.3836679988468,34.0186125009919,54.));
#39171=CARTESIAN_POINT('Ctrl Pts',(-33.2690708798524,33.0793586530485,41.));
#39172=CARTESIAN_POINT('Ctrl Pts',(-33.3144021367584,33.0370694015056,41.));
#39173=CARTESIAN_POINT('Ctrl Pts',(-33.357003518039,32.9922111868308,41.));
#39174=CARTESIAN_POINT('Ctrl Pts',(-33.396876415392,32.9451289935681,41.));
#39175=CARTESIAN_POINT('Ctrl Pts',(-33.4393774108012,32.8949435239245,41.));
#39176=CARTESIAN_POINT('Ctrl Pts',(-33.478779113966,32.8422310065705,41.));
#39177=CARTESIAN_POINT('Ctrl Pts',(-33.5150543890132,32.7873545360889,41.));
#39178=CARTESIAN_POINT('Ctrl Pts',(-33.5467952546795,32.7393376244174,41.));
#39179=CARTESIAN_POINT('Ctrl Pts',(-33.5761422056407,32.689662710961,41.));
#39180=CARTESIAN_POINT('Ctrl Pts',(-33.6030541769026,32.6385454943499,41.));
#39181=CARTESIAN_POINT('Ctrl Pts',(-33.6165537545645,32.6129040863392,41.));
#39182=CARTESIAN_POINT('Ctrl Pts',(-33.6294402762058,32.5868994069059,41.));
#39183=CARTESIAN_POINT('Ctrl Pts',(-33.641706218416,32.5605568410562,41.));
#39184=CARTESIAN_POINT('Ctrl Pts',(-33.6473173816178,32.5485062024991,41.));
#39185=CARTESIAN_POINT('Ctrl Pts',(-33.6527992584238,32.5363831634529,41.));
#39186=CARTESIAN_POINT('Ctrl Pts',(-33.6581426077326,32.5242101295597,41.));
#39187=CARTESIAN_POINT('Ctrl Pts',(-33.685064215522,32.4628782522786,41.));
#39188=CARTESIAN_POINT('Ctrl Pts',(-33.7085245448721,32.4001709264115,41.));
#39189=CARTESIAN_POINT('Ctrl Pts',(-33.728499993566,32.3364458568814,41.));
#39190=CARTESIAN_POINT('Ctrl Pts',(-33.7488294565481,32.2715914217246,41.));
#39191=CARTESIAN_POINT('Ctrl Pts',(-33.7655499805244,32.205682007983,41.));
#39192=CARTESIAN_POINT('Ctrl Pts',(-33.778597371195,32.139058167292,41.));
#39193=CARTESIAN_POINT('Ctrl Pts',(-33.7895089756291,32.0833402836288,41.));
#39194=CARTESIAN_POINT('Ctrl Pts',(-33.7978510101904,32.0271217838561,41.));
#39195=CARTESIAN_POINT('Ctrl Pts',(-33.8035611097405,31.97058958092,41.));
#39196=CARTESIAN_POINT('Ctrl Pts',(-33.8061908976541,31.9445536593552,41.));
#39197=CARTESIAN_POINT('Ctrl Pts',(-33.8082620999711,31.9184510862623,41.));
#39198=CARTESIAN_POINT('Ctrl Pts',(-33.8097668241107,31.8922997194398,41.));
#39199=CARTESIAN_POINT('Ctrl Pts',(-33.8104248596001,31.880863385687,41.));
#39200=CARTESIAN_POINT('Ctrl Pts',(-33.8109744437721,31.8694179108277,41.));
#39201=CARTESIAN_POINT('Ctrl Pts',(-33.8114145802126,31.8579789498471,41.));
#39202=CARTESIAN_POINT('Ctrl Pts',(-33.8141127536739,31.7878545563686,41.));
#39203=CARTESIAN_POINT('Ctrl Pts',(-33.8127099564223,31.7178435879866,41.));
#39204=CARTESIAN_POINT('Ctrl Pts',(-33.8071514622337,31.6483067461029,41.));
#39205=CARTESIAN_POINT('Ctrl Pts',(-33.8021840858831,31.5861647968351,41.));
#39206=CARTESIAN_POINT('Ctrl Pts',(-33.7938975383786,31.524400531023,41.));
#39207=CARTESIAN_POINT('Ctrl Pts',(-33.7822196781911,31.4632592560481,41.));
#39208=CARTESIAN_POINT('Ctrl Pts',(-33.769491639951,31.3966196085928,41.));
#39209=CARTESIAN_POINT('Ctrl Pts',(-33.7527359979084,31.3307192075773,41.));
#39210=CARTESIAN_POINT('Ctrl Pts',(-33.732198040194,31.2657716978078,41.));
#39211=CARTESIAN_POINT('Ctrl Pts',(-33.7242658128154,31.2406874892254,41.));
#39212=CARTESIAN_POINT('Ctrl Pts',(-33.7157688301419,31.2157454686801,41.));
#39213=CARTESIAN_POINT('Ctrl Pts',(-33.7067192107323,31.1909582653564,41.));
#39214=CARTESIAN_POINT('Ctrl Pts',(-33.7027507419357,31.1800884996244,41.));
#39215=CARTESIAN_POINT('Ctrl Pts',(-33.698676095927,31.1692490592239,41.));
#39216=CARTESIAN_POINT('Ctrl Pts',(-33.6945013882907,31.1584535681983,41.));
#39217=CARTESIAN_POINT('Ctrl Pts',(-33.6692787473599,31.0932296489372,41.));
#39218=CARTESIAN_POINT('Ctrl Pts',(-33.6403651885278,31.0294907437057,41.));
#39219=CARTESIAN_POINT('Ctrl Pts',(-33.6080734174902,30.9674557344658,41.));
#39220=CARTESIAN_POINT('Ctrl Pts',(-33.5750332658763,30.9039830278043,41.));
#39221=CARTESIAN_POINT('Ctrl Pts',(-33.5384562013509,30.8422932904506,41.));
#39222=CARTESIAN_POINT('Ctrl Pts',(-33.4986210386776,30.7826246842389,41.));
#39223=CARTESIAN_POINT('Ctrl Pts',(-33.4681150414624,30.7369301216272,41.));
#39224=CARTESIAN_POINT('Ctrl Pts',(-33.4356970894283,30.6924208354612,41.));
#39225=CARTESIAN_POINT('Ctrl Pts',(-33.401472825112,30.6492098980629,41.));
#39226=CARTESIAN_POINT('Ctrl Pts',(-33.3801641910076,30.6223060018733,41.));
#39227=CARTESIAN_POINT('Ctrl Pts',(-33.3581550105309,30.5959055373049,41.));
#39228=CARTESIAN_POINT('Ctrl Pts',(-33.3354678681772,30.5700374883911,41.));
#39229=CARTESIAN_POINT('Ctrl Pts',(-33.3228125346432,30.5556077827115,41.));
#39230=CARTESIAN_POINT('Ctrl Pts',(-33.3099418038776,30.5413392395066,41.));
#39231=CARTESIAN_POINT('Ctrl Pts',(-33.2968831946259,30.5272622022597,41.));
#39232=CARTESIAN_POINT('Ctrl Pts',(-33.2460103743684,30.4724218611623,41.));
#39233=CARTESIAN_POINT('Ctrl Pts',(-33.1922409878963,30.4204264438423,41.));
#39234=CARTESIAN_POINT('Ctrl Pts',(-33.1358600523127,30.3715399649794,41.));
#39235=CARTESIAN_POINT('Ctrl Pts',(-33.0937060828269,30.3349893274824,41.));
#39236=CARTESIAN_POINT('Ctrl Pts',(-33.0500910988085,30.3001767875303,41.));
#39237=CARTESIAN_POINT('Ctrl Pts',(-33.0051178417279,30.2672224267123,41.));
#39238=CARTESIAN_POINT('Ctrl Pts',(-32.991033633089,30.2569021581027,41.));
#39239=CARTESIAN_POINT('Ctrl Pts',(-32.9768161196749,30.2467642066019,41.));
#39240=CARTESIAN_POINT('Ctrl Pts',(-32.9624682145604,30.2368124882568,41.));
#39241=CARTESIAN_POINT('Ctrl Pts',(-32.9486861836171,30.2272532606847,41.));
#39242=CARTESIAN_POINT('Ctrl Pts',(-32.9347908994425,30.217870822758,41.));
#39243=CARTESIAN_POINT('Ctrl Pts',(-32.9207902789774,30.2086713607756,41.));
#39244=CARTESIAN_POINT('Ctrl Pts',(-32.8578346023933,30.1673047402921,41.));
#39245=CARTESIAN_POINT('Ctrl Pts',(-32.7927216169288,30.1296140460093,41.));
#39246=CARTESIAN_POINT('Ctrl Pts',(-32.7257126755435,30.095878544712,41.));
#39247=CARTESIAN_POINT('Ctrl Pts',(-32.6745222019714,30.0701068155682,41.));
#39248=CARTESIAN_POINT('Ctrl Pts',(-32.6222242810127,30.046643732657,41.));
#39249=CARTESIAN_POINT('Ctrl Pts',(-32.5689215997279,30.0256290168506,41.));
#39250=CARTESIAN_POINT('Ctrl Pts',(-32.5564364835041,30.0207067284604,41.));
#39251=CARTESIAN_POINT('Ctrl Pts',(-32.5438961977317,30.0159188346434,41.));
#39252=CARTESIAN_POINT('Ctrl Pts',(-32.5313026984106,30.0112647410448,41.));
#39253=CARTESIAN_POINT('Ctrl Pts',(-30.3326930047543,31.9986962112692,42.1285196366098));
#39254=CARTESIAN_POINT('Ctrl Pts',(-30.3319567964985,31.9130463864536,42.1227790551389));
#39255=CARTESIAN_POINT('Ctrl Pts',(-30.3379868569258,31.8275005632038,42.1170384736681));
#39256=CARTESIAN_POINT('Ctrl Pts',(-30.3511440008779,31.7430654121314,42.1112978921973));
#39257=CARTESIAN_POINT('Ctrl Pts',(-30.4360454254438,31.1982158128894,42.074254629124));
#39258=CARTESIAN_POINT('Ctrl Pts',(-30.8177158617989,30.6996141751516,42.0372113660508));
#39259=CARTESIAN_POINT('Ctrl Pts',(-31.32150540483,30.4754087738067,42.0001681029776));
#39260=CARTESIAN_POINT('Ctrl Pts',(-31.8252949478612,30.2512033724617,41.9631248399043));
#39261=CARTESIAN_POINT('Ctrl Pts',(-32.4512035975684,30.3013942075097,41.9260815768311));
#39262=CARTESIAN_POINT('Ctrl Pts',(-32.9128181241709,30.6030322996287,41.8890383137578));
#39263=CARTESIAN_POINT('Ctrl Pts',(-33.3744326507733,30.9046703917478,41.8519950506846));
#39264=CARTESIAN_POINT('Ctrl Pts',(-33.671753054271,31.4577557409379,41.8149517876113));
#39265=CARTESIAN_POINT('Ctrl Pts',(-33.6687287642475,32.009163711811,41.7779085245381));
#39266=CARTESIAN_POINT('Ctrl Pts',(-33.665704474224,32.5605716826841,41.7408652614648));
#39267=CARTESIAN_POINT('Ctrl Pts',(-33.3623354906794,33.1103022752402,41.7038219983916));
#39268=CARTESIAN_POINT('Ctrl Pts',(-32.8974385813771,33.4068725754867,41.6667787353184));
#39269=CARTESIAN_POINT('Ctrl Pts',(-32.4325416720748,33.7034428757333,41.6297354722451));
#39270=CARTESIAN_POINT('Ctrl Pts',(-31.8061168370147,33.7468528836704,41.5926922091719));
#39271=CARTESIAN_POINT('Ctrl Pts',(-31.3048190804959,33.5170982043666,41.5556489460986));
#39272=CARTESIAN_POINT('Ctrl Pts',(-30.803521323977,33.2873435250628,41.5186056830254));
#39273=CARTESIAN_POINT('Ctrl Pts',(-30.4273506459994,32.7844241585182,41.4815624199522));
#39274=CARTESIAN_POINT('Ctrl Pts',(-30.3484281139147,32.238751004344,41.4445191568789));
#39275=CARTESIAN_POINT('Ctrl Pts',(-30.3370655201346,32.1601896325297,41.4391859834559));
#39276=CARTESIAN_POINT('Ctrl Pts',(-30.3318642226577,32.080742069305,41.4338528100328));
#39277=CARTESIAN_POINT('Ctrl Pts',(-30.3325261571163,32.001210199007,41.4285196366098));
#39278=CARTESIAN_POINT('Ctrl Pts',(-31.4698297828114,30.0148256743283,41.));
#39279=CARTESIAN_POINT('Ctrl Pts',(-30.8097602092473,30.1911070339301,41.0370432630732));
#39280=CARTESIAN_POINT('Ctrl Pts',(-29.6907568006176,31.251212957076,41.1111297892197));
#39281=CARTESIAN_POINT('Ctrl Pts',(-30.1186158644953,33.5380364303402,41.2222595784395));
#39282=CARTESIAN_POINT('Ctrl Pts',(-32.2715961695763,34.4127962262488,41.3333893676592));
#39283=CARTESIAN_POINT('Ctrl Pts',(-34.1743722121293,33.0815585185448,41.4445191568789));
#39284=CARTESIAN_POINT('Ctrl Pts',(-34.088014018114,30.7594030715832,41.5556489460986));
#39285=CARTESIAN_POINT('Ctrl Pts',(-32.0903101568642,29.5731769531958,41.6667787353184));
#39286=CARTESIAN_POINT('Ctrl Pts',(-30.0101664816534,30.6076759834516,41.777908524538));
#39287=CARTESIAN_POINT('Ctrl Pts',(-29.7509902552198,32.9165547583188,41.8890383137579));
#39288=CARTESIAN_POINT('Ctrl Pts',(-31.5501372064992,34.3865418916543,42.0001681029775));
#39289=CARTESIAN_POINT('Ctrl Pts',(-33.7609665083167,33.6724274609132,42.1112978921974));
#39290=CARTESIAN_POINT('Ctrl Pts',(-34.3601920973369,31.4277075251964,42.2224276814169));
#39291=CARTESIAN_POINT('Ctrl Pts',(-32.7993885345327,29.7067525630187,42.3335574706368));
#39292=CARTESIAN_POINT('Ctrl Pts',(-30.5069967591677,30.0845481859775,42.4446872598564));
#39293=CARTESIAN_POINT('Ctrl Pts',(-29.5809835883393,32.2153468604003,42.5558170490762));
#39294=CARTESIAN_POINT('Ctrl Pts',(-30.8688288986318,34.1490612499125,42.6669468382959));
#39295=CARTESIAN_POINT('Ctrl Pts',(-33.1919092821327,34.1159786819058,42.7780766275156));
#39296=CARTESIAN_POINT('Ctrl Pts',(-34.4241674445136,32.1463750716222,42.8892064167354));
#39297=CARTESIAN_POINT('Ctrl Pts',(-33.4378537354262,30.0428107344064,43.0003362059551));
#39298=CARTESIAN_POINT('Ctrl Pts',(-31.1356319387654,29.7304447118329,43.1114659951747));
#39299=CARTESIAN_POINT('Ctrl Pts',(-29.6244703886607,31.4951511152756,43.2225957843946));
#39300=CARTESIAN_POINT('Ctrl Pts',(-30.2873677921603,33.7218897236688,43.3337255736142));
#39301=CARTESIAN_POINT('Ctrl Pts',(-32.5176476120498,34.372773539922,43.4448553628341));
#39302=CARTESIAN_POINT('Ctrl Pts',(-34.2741819548352,32.8521207391232,43.5559851520537));
#39303=CARTESIAN_POINT('Ctrl Pts',(-33.9494096331178,30.5516162812554,43.6671149412735));
#39304=CARTESIAN_POINT('Ctrl Pts',(-31.8405587566049,29.5766568944465,43.7782447304931));
#39305=CARTESIAN_POINT('Ctrl Pts',(-29.8776267764906,30.8195148384194,43.889374519713));
#39306=CARTESIAN_POINT('Ctrl Pts',(-29.8570677545995,33.1427400001187,44.0005043089325));
#39307=CARTESIAN_POINT('Ctrl Pts',(-31.7976970844419,34.4201419063721,44.1116340981524));
#39308=CARTESIAN_POINT('Ctrl Pts',(-33.9234718487822,33.4826561851773,44.2227638873721));
#39309=CARTESIAN_POINT('Ctrl Pts',(-34.2889060362689,31.1882596020868,44.3338936765918));
#39310=CARTESIAN_POINT('Ctrl Pts',(-32.5595582415307,29.6367590281872,44.4450234658115));
#39311=CARTESIAN_POINT('Ctrl Pts',(-30.3181088122919,30.2480709634203,44.5561532550313));
#39312=CARTESIAN_POINT('Ctrl Pts',(-29.6159079586973,32.4627293540464,44.6672830442509));
#39313=CARTESIAN_POINT('Ctrl Pts',(-31.0956022868993,34.2539028579429,44.7784128334708));
#39314=CARTESIAN_POINT('Ctrl Pts',(-33.4029915943473,33.9823289088073,44.8895426226903));
#39315=CARTESIAN_POINT('Ctrl Pts',(-34.4263782094584,31.8965490397939,45.0006724119102));
#39316=CARTESIAN_POINT('Ctrl Pts',(-33.2291698002495,29.9054463676817,45.1118022011298));
#39317=CARTESIAN_POINT('Ctrl Pts',(-30.9070385196435,29.8312564653792,45.2229319903496));
#39318=CARTESIAN_POINT('Ctrl Pts',(-29.5851737331861,31.7418771269173,45.3340617795693));
#39319=CARTESIAN_POINT('Ctrl Pts',(-30.4733317584164,33.8887290426746,45.4451915687891));
#39320=CARTESIAN_POINT('Ctrl Pts',(-32.7586800023163,34.3070366209898,45.5563213580088));
#39321=CARTESIAN_POINT('Ctrl Pts',(-34.3496925356383,32.6139693025454,45.6674511472286));
#39322=CARTESIAN_POINT('Ctrl Pts',(-33.7902919416986,30.3590039366313,45.7785809364482));
#39323=CARTESIAN_POINT('Ctrl Pts',(-31.592435577624,29.605860372051,45.889710725668));
#39324=CARTESIAN_POINT('Ctrl Pts',(-29.7675777530558,31.0438074316064,46.0008405148877));
#39325=CARTESIAN_POINT('Ctrl Pts',(-29.9858085592797,33.3568515602791,46.1119703041074));
#39326=CARTESIAN_POINT('Ctrl Pts',(-32.0474055290543,34.4281198554267,46.2231000933271));
#39327=CARTESIAN_POINT('Ctrl Pts',(-34.0656174727299,33.2771991907512,46.3342298825469));
#39328=CARTESIAN_POINT('Ctrl Pts',(-34.1933987060518,30.9573996773486,46.4453596717666));
#39329=CARTESIAN_POINT('Ctrl Pts',(-32.3138052300136,29.5917766727069,46.5564894609864));
#39330=CARTESIAN_POINT('Ctrl Pts',(-30.1470206105429,30.4301335411094,46.667619250206));
#39331=CARTESIAN_POINT('Ctrl Pts',(-29.6760626335787,32.7052151681957,46.7787490394258));
#39332=CARTESIAN_POINT('Ctrl Pts',(-31.3319469323119,34.3348915210894,46.8898788286455));
#39333=CARTESIAN_POINT('Ctrl Pts',(-33.5992261538594,33.8277004747262,47.0010086178653));
#39334=CARTESIAN_POINT('Ctrl Pts',(-34.4029109422803,31.64781777448,47.1121384070849));
#39335=CARTESIAN_POINT('Ctrl Pts',(-33.0074776948103,29.7902484277724,47.2232681963048));
#39336=CARTESIAN_POINT('Ctrl Pts',(-30.6900117866906,29.9550197562096,47.3343979855244));
#39337=CARTESIAN_POINT('Ctrl Pts',(-29.571432885161,31.9913348268765,47.4455277747442));
#39338=CARTESIAN_POINT('Ctrl Pts',(-30.6754522704185,34.0355801700161,47.5566575639638));
#39339=CARTESIAN_POINT('Ctrl Pts',(-32.9916833736669,34.2168846165047,47.6677873531836));
#39340=CARTESIAN_POINT('Ctrl Pts',(-34.4003366076938,32.3693203030807,47.7789171424033));
#39341=CARTESIAN_POINT('Ctrl Pts',(-33.6122278089259,30.1837580533892,47.890046931623));
#39342=CARTESIAN_POINT('Ctrl Pts',(-31.3486256033116,29.6604007369121,48.0011767208428));
#39343=CARTESIAN_POINT('Ctrl Pts',(-29.6811541816853,31.2782192941156,48.1123065100625));
#39344=CARTESIAN_POINT('Ctrl Pts',(-30.1358653061449,33.5566037259586,48.2234362992823));
#39345=CARTESIAN_POINT('Ctrl Pts',(-32.2966122867217,34.4104013084688,48.3345660885019));
#39346=CARTESIAN_POINT('Ctrl Pts',(-34.1859029191172,33.0582257531821,48.4456958777217));
#39347=CARTESIAN_POINT('Ctrl Pts',(-34.0746789050666,30.7375734645635,48.5568256669414));
#39348=CARTESIAN_POINT('Ctrl Pts',(-32.064731256055,29.5722802507307,48.6679554561612));
#39349=CARTESIAN_POINT('Ctrl Pts',(-29.995542263483,30.6288098239048,48.7790852453808));
#39350=CARTESIAN_POINT('Ctrl Pts',(-29.7608112539325,32.940237776303,48.8902150346006));
#39351=CARTESIAN_POINT('Ctrl Pts',(-31.5753615017921,34.3911703122827,49.0013448238203));
#39352=CARTESIAN_POINT('Ctrl Pts',(-33.7785362981989,33.6537297096236,49.1124746130401));
#39353=CARTESIAN_POINT('Ctrl Pts',(-34.354013961917,31.4028136106688,49.2236044022597));
#39354=CARTESIAN_POINT('Ctrl Pts',(-32.7751235759071,29.6984360190133,49.3347341914796));
#39355=CARTESIAN_POINT('Ctrl Pts',(-30.4868484990922,30.1004248233347,49.4458639806991));
#39356=CARTESIAN_POINT('Ctrl Pts',(-29.5833932664634,32.2408842293052,49.556993769919));
#39357=CARTESIAN_POINT('Ctrl Pts',(-30.8915903093585,34.1608890008963,49.6681235591386));
#39358=CARTESIAN_POINT('Ctrl Pts',(-33.2141918809262,34.1032715927325,49.7792533483584));
#39359=CARTESIAN_POINT('Ctrl Pts',(-34.4255782104328,32.1207628319306,49.8903831375781));
#39360=CARTESIAN_POINT('Ctrl Pts',(-33.4171016660518,30.0277332369641,50.0015129267978));
#39361=CARTESIAN_POINT('Ctrl Pts',(-31.1117090447276,29.7397007951857,50.1126427160176));
#39362=CARTESIAN_POINT('Ctrl Pts',(-29.6192706725547,31.5202696737293,50.2237725052373));
#39363=CARTESIAN_POINT('Ctrl Pts',(-30.3056499629249,33.7398825444167,50.334902294457));
#39364=CARTESIAN_POINT('Ctrl Pts',(-32.5426800327657,34.3671737786953,50.4460320836768));
#39365=CARTESIAN_POINT('Ctrl Pts',(-34.2830552217384,32.828053241641,50.5571618728965));
#39366=CARTESIAN_POINT('Ctrl Pts',(-33.9340030304806,30.5311073577035,50.6682916621162));
#39367=CARTESIAN_POINT('Ctrl Pts',(-31.8149722391133,29.5784760905123,50.779421451336));
#39368=CARTESIAN_POINT('Ctrl Pts',(-29.8652768479733,30.8419972449628,50.8905512405557));
#39369=CARTESIAN_POINT('Ctrl Pts',(-29.869256935447,33.1653099627831,51.0016810297754));
#39370=CARTESIAN_POINT('Ctrl Pts',(-31.8232699686781,34.4221436399707,51.1128108189951));
#39371=CARTESIAN_POINT('Ctrl Pts',(-33.9390244099684,33.4622577248198,51.2239406082149));
#39372=CARTESIAN_POINT('Ctrl Pts',(-34.2802047391973,31.1641293976194,51.3350703974346));
#39373=CARTESIAN_POINT('Ctrl Pts',(-32.5345664187102,29.6309807807203,51.4462001866543));
#39374=CARTESIAN_POINT('Ctrl Pts',(-30.2996987093337,30.2659328630714,51.557329975874));
#39375=CARTESIAN_POINT('Ctrl Pts',(-29.6209283014176,32.4878843825608,51.6684597650938));
#39376=CARTESIAN_POINT('Ctrl Pts',(-31.1194585135859,34.2633294087954,51.7795895543135));
#39377=CARTESIAN_POINT('Ctrl Pts',(-33.423850742076,33.9673998993839,51.8907193435332));
#39378=CARTESIAN_POINT('Ctrl Pts',(-34.4251502183154,31.8709273485123,52.001849132753));
#39379=CARTESIAN_POINT('Ctrl Pts',(-33.2069785027727,29.8925806669829,52.1129789219727));
#39380=CARTESIAN_POINT('Ctrl Pts',(-30.8841931736715,29.8429213477129,52.2241087111924));
#39381=CARTESIAN_POINT('Ctrl Pts',(-29.5825821059866,31.7673969339495,52.3352385004122));
#39382=CARTESIAN_POINT('Ctrl Pts',(-30.4933657694112,33.9047484910958,52.4463682896318));
#39383=CARTESIAN_POINT('Ctrl Pts',(-32.7830045631024,34.2988945540426,52.5574980788516));
#39384=CARTESIAN_POINT('Ctrl Pts',(-34.3560464259567,32.5891179074725,52.6686278680713));
#39385=CARTESIAN_POINT('Ctrl Pts',(-33.7728594492291,30.3401856422308,52.7797576572911));
#39386=CARTESIAN_POINT('Ctrl Pts',(-31.5671721178615,29.6103000479543,52.8908874465108));
#39387=CARTESIAN_POINT('Ctrl Pts',(-29.7576014236038,31.0674368452352,53.0020172357304));
#39388=CARTESIAN_POINT('Ctrl Pts',(-30.0002550266955,33.3780554042465,53.1131470249502));
#39389=CARTESIAN_POINT('Ctrl Pts',(-32.0730427769752,34.4274726540847,53.2242768141699));
#39390=CARTESIAN_POINT('Ctrl Pts',(-34.0790038841791,33.2553327473947,53.3354066033897));
#39391=CARTESIAN_POINT('Ctrl Pts',(-34.182240985042,30.9342477393896,53.4465363926094));
#39392=CARTESIAN_POINT('Ctrl Pts',(-32.288398343005,29.5886824305611,53.5576661818291));
#39393=CARTESIAN_POINT('Ctrl Pts',(-30.130451271847,30.4496223583594,53.6687959710488));
#39394=CARTESIAN_POINT('Ctrl Pts',(-29.6838223728037,32.7300579053691,53.7799257602686));
#39395=CARTESIAN_POINT('Ctrl Pts',(-31.3562857209018,34.3411497251595,53.8910555494883));
#39396=CARTESIAN_POINT('Ctrl Pts',(-33.6191545377039,33.8120432967827,54.002185338708));
#39397=CARTESIAN_POINT('Ctrl Pts',(-34.3976274079488,31.6196462144305,54.1133151279277));
#39398=CARTESIAN_POINT('Ctrl Pts',(-33.4572031808897,30.3983372977455,54.1874016540742));
#39399=CARTESIAN_POINT('Ctrl Pts',(-32.8326019491389,30.121497522815,54.2244449171475));
#39400=CARTESIAN_POINT('Ctrl Pts',(-31.5032651029123,30.1400211999972,40.9251850276175));
#39401=CARTESIAN_POINT('Ctrl Pts',(-30.8848229855226,30.3051853306507,40.9622282906908));
#39402=CARTESIAN_POINT('Ctrl Pts',(-29.8363898125428,31.2984354031054,41.0363148168372));
#39403=CARTESIAN_POINT('Ctrl Pts',(-30.2372658353235,33.4410397701959,41.147444606057));
#39404=CARTESIAN_POINT('Ctrl Pts',(-32.2544678878028,34.2606326162469,41.2585743952767));
#39405=CARTESIAN_POINT('Ctrl Pts',(-34.0372448734482,33.0133497544479,41.3697041844965));
#39406=CARTESIAN_POINT('Ctrl Pts',(-33.956332880986,30.8376416336016,41.4808339737161));
#39407=CARTESIAN_POINT('Ctrl Pts',(-32.0846147237652,29.7262251682171,41.5919637629359));
#39408=CARTESIAN_POINT('Ctrl Pts',(-30.1356558404978,30.6954832530194,41.7030935521556));
#39409=CARTESIAN_POINT('Ctrl Pts',(-29.8928246289527,32.8587519984865,41.8142233413753));
#39410=CARTESIAN_POINT('Ctrl Pts',(-31.5785079184226,34.2360340179664,41.9253531305951));
#39411=CARTESIAN_POINT('Ctrl Pts',(-33.6499107058901,33.5669553961153,42.0364829198148));
#39412=CARTESIAN_POINT('Ctrl Pts',(-34.2113459801549,31.4637992962278,42.1476127090345));
#39413=CARTESIAN_POINT('Ctrl Pts',(-32.7489748925163,29.8513767981043,42.2587424982542));
#39414=CARTESIAN_POINT('Ctrl Pts',(-30.6011533897186,30.205346643649,42.3698722874739));
#39415=CARTESIAN_POINT('Ctrl Pts',(-29.7335394759222,32.2017659556705,42.4810020766937));
#39416=CARTESIAN_POINT('Ctrl Pts',(-30.9401664929307,34.0135301535256,42.5921318659134));
#39417=CARTESIAN_POINT('Ctrl Pts',(-33.1167412189572,33.9825339461162,42.7032616551331));
#39418=CARTESIAN_POINT('Ctrl Pts',(-34.2712867057287,32.1371438903604,42.8143914443529));
#39419=CARTESIAN_POINT('Ctrl Pts',(-33.3471751225135,30.1662413751168,42.9255212335726));
#39420=CARTESIAN_POINT('Ctrl Pts',(-31.1901435312227,29.8735747955049,43.0366510227923));
#39421=CARTESIAN_POINT('Ctrl Pts',(-29.7742837700791,31.52698953908,43.1477808120121));
#39422=CARTESIAN_POINT('Ctrl Pts',(-30.3953753795874,33.6132983086424,43.2589106012317));
#39423=CARTESIAN_POINT('Ctrl Pts',(-32.485002033239,34.2231339708512,43.3700403904516));
#39424=CARTESIAN_POINT('Ctrl Pts',(-34.1307600892487,32.7983815271616,43.4811701796711));
#39425=CARTESIAN_POINT('Ctrl Pts',(-33.8264696169156,30.6429589702544,43.5922999688911));
#39426=CARTESIAN_POINT('Ctrl Pts',(-31.8506139593254,29.7294856460844,43.7034297581105));
#39427=CARTESIAN_POINT('Ctrl Pts',(-30.0114747856789,30.8939624365156,43.8145595473305));
#39428=CARTESIAN_POINT('Ctrl Pts',(-29.9922123237522,33.0706728102665,43.92568933655));
#39429=CARTESIAN_POINT('Ctrl Pts',(-31.8104553694601,34.2675150391779,44.0368191257699));
#39430=CARTESIAN_POINT('Ctrl Pts',(-33.8021676055711,33.3891520943329,44.1479489149895));
#39431=CARTESIAN_POINT('Ctrl Pts',(-34.1445555927276,31.2394522175207,44.2590787042094));
#39432=CARTESIAN_POINT('Ctrl Pts',(-32.5242695581717,29.7857974234166,44.370208493429));
#39433=CARTESIAN_POINT('Ctrl Pts',(-30.4241777094362,30.3585568153845,44.4813382826488));
#39434=CARTESIAN_POINT('Ctrl Pts',(-29.7662613319473,32.4335472091974,44.5924680718684));
#39435=CARTESIAN_POINT('Ctrl Pts',(-31.1526383595712,34.1117598987791,44.7035978610883));
#39436=CARTESIAN_POINT('Ctrl Pts',(-33.3145115712621,33.8573128300793,44.8147276503079));
#39437=CARTESIAN_POINT('Ctrl Pts',(-34.2733580482179,31.9030732010106,44.9258574395277));
#39438=CARTESIAN_POINT('Ctrl Pts',(-33.1516518929863,30.0375399272492,45.0369872287473));
#39439=CARTESIAN_POINT('Ctrl Pts',(-30.9759664144383,29.9680288300763,45.1481170179672));
#39440=CARTESIAN_POINT('Ctrl Pts',(-29.7374653682146,31.7581557118077,45.2592468071868));
#39441=CARTESIAN_POINT('Ctrl Pts',(-30.5696114808345,33.7696158634006,45.3703765964066));
#39442=CARTESIAN_POINT('Ctrl Pts',(-32.7108336542772,34.1615427674943,45.4815063856263));
#39443=CARTESIAN_POINT('Ctrl Pts',(-34.2015085759953,32.5752491717323,45.592636174846));
#39444=CARTESIAN_POINT('Ctrl Pts',(-33.677386723329,30.4624937723185,45.7037659640658));
#39445=CARTESIAN_POINT('Ctrl Pts',(-31.6181387319734,29.756847398918,45.8148957532855));
#39446=CARTESIAN_POINT('Ctrl Pts',(-29.9083660320029,31.1041099600508,45.9260255425052));
#39447=CARTESIAN_POINT('Ctrl Pts',(-30.1128340567174,33.2712813702222,46.0371553317249));
#39448=CARTESIAN_POINT('Ctrl Pts',(-32.0444158872617,34.2749898568386,46.1482851209447));
#39449=CARTESIAN_POINT('Ctrl Pts',(-33.9353487794544,33.196652297714,46.2594149101644));
#39450=CARTESIAN_POINT('Ctrl Pts',(-34.0550714566739,31.0231515328753,46.3705446993841));
#39451=CARTESIAN_POINT('Ctrl Pts',(-32.2940150230675,29.7436518916687,46.4816744886039));
#39452=CARTESIAN_POINT('Ctrl Pts',(-30.2638792288098,30.5291375701305,46.5928042778235));
#39453=CARTESIAN_POINT('Ctrl Pts',(-29.8226223368996,32.6607405935701,46.7039340670433));
#39454=CARTESIAN_POINT('Ctrl Pts',(-31.3740778695814,34.1876409912076,46.815063856263));
#39455=CARTESIAN_POINT('Ctrl Pts',(-33.4983705481795,33.7124360776707,46.9261936454827));
#39456=CARTESIAN_POINT('Ctrl Pts',(-34.2513707502356,31.6700282364455,47.0373234347025));
#39457=CARTESIAN_POINT('Ctrl Pts',(-32.9439408567753,29.9296069748306,47.1484532239222));
#39458=CARTESIAN_POINT('Ctrl Pts',(-30.7726265278065,30.0839869573734,47.2595830131419));
#39459=CARTESIAN_POINT('Ctrl Pts',(-29.7245910902782,31.9918812982318,47.3707128023617));
#39460=CARTESIAN_POINT('Ctrl Pts',(-30.7589852111452,33.9072057869049,47.4818425915814));
#39461=CARTESIAN_POINT('Ctrl Pts',(-32.9291426085271,34.0770762221881,47.5929723808011));
#39462=CARTESIAN_POINT('Ctrl Pts',(-34.248958766717,32.3460290238784,47.7041021700208));
#39463=CARTESIAN_POINT('Ctrl Pts',(-33.5105522505498,30.2982998154438,47.8152319592406));
#39464=CARTESIAN_POINT('Ctrl Pts',(-31.3897046959364,29.8079481617449,47.9263617484603));
#39465=CARTESIAN_POINT('Ctrl Pts',(-29.8273927852251,31.3237385786048,48.0374915376801));
#39466=CARTESIAN_POINT('Ctrl Pts',(-30.2534274365316,33.4584361145758,48.1486213268997));
#39467=CARTESIAN_POINT('Ctrl Pts',(-32.2779063571337,34.2583887345682,48.2597511161195));
#39468=CARTESIAN_POINT('Ctrl Pts',(-34.048048393456,32.9914884758897,48.3708809053392));
#39469=CARTESIAN_POINT('Ctrl Pts',(-33.9438387502473,30.8171887163217,48.4820106945589));
#39470=CARTESIAN_POINT('Ctrl Pts',(-32.0606489628658,29.7253850165219,48.5931404837786));
#39471=CARTESIAN_POINT('Ctrl Pts',(-30.1219539023801,30.7152842824289,48.7042702729984));
#39472=CARTESIAN_POINT('Ctrl Pts',(-29.9020262638743,32.8809414408952,48.8154000622181));
#39473=CARTESIAN_POINT('Ctrl Pts',(-31.602141437093,34.2403705460662,48.9265298514378));
#39474=CARTESIAN_POINT('Ctrl Pts',(-33.6663724524877,33.5494368232845,49.0376596406576));
#39475=CARTESIAN_POINT('Ctrl Pts',(-34.2055574704225,31.4404753227754,49.1487894298773));
#39476=CARTESIAN_POINT('Ctrl Pts',(-32.7262402097014,29.8435847390698,49.259919219097));
#39477=CARTESIAN_POINT('Ctrl Pts',(-30.5822757848087,30.2202220168179,49.3710490083167));
#39478=CARTESIAN_POINT('Ctrl Pts',(-29.7357971870802,32.2256928038857,49.4821787975365));
#39479=CARTESIAN_POINT('Ctrl Pts',(-30.9614924494789,34.0246119843739,49.5933085867562));
#39480=CARTESIAN_POINT('Ctrl Pts',(-33.1376185599691,33.9706282327658,49.7044383759759));
#39481=CARTESIAN_POINT('Ctrl Pts',(-34.2726085013351,32.1131468931038,49.8155681651957));
#39482=CARTESIAN_POINT('Ctrl Pts',(-33.3277317876923,30.1521147439001,49.9266979544153));
#39483=CARTESIAN_POINT('Ctrl Pts',(-31.167729340605,29.8822471415979,50.0378277436351));
#39484=CARTESIAN_POINT('Ctrl Pts',(-29.7694119753968,31.550523989232,50.1489575328548));
#39485=CARTESIAN_POINT('Ctrl Pts',(-30.4125045805853,33.6301564075563,50.2600873220745));
#39486=CARTESIAN_POINT('Ctrl Pts',(-32.5084557779517,34.2178873599959,50.3712171112943));
#39487=CARTESIAN_POINT('Ctrl Pts',(-34.1390737613091,32.7758318525526,50.482346900514));
#39488=CARTESIAN_POINT('Ctrl Pts',(-33.8120346356071,30.6237434472022,50.5934766897338));
#39489=CARTESIAN_POINT('Ctrl Pts',(-31.8266410620917,29.7311901140859,50.7046064789534));
#39490=CARTESIAN_POINT('Ctrl Pts',(-29.9999037085566,30.9150269843506,50.8157362681732));
#39491=CARTESIAN_POINT('Ctrl Pts',(-30.0036327907976,33.0918193924733,50.9268660573929));
#39492=CARTESIAN_POINT('Ctrl Pts',(-31.8344154932231,34.2693905329361,51.0379958466127));
#39493=CARTESIAN_POINT('Ctrl Pts',(-33.8167393405155,33.3700400680856,51.1491256358324));
#39494=CARTESIAN_POINT('Ctrl Pts',(-34.1364030451772,31.2168437905586,51.2602554250521));
#39495=CARTESIAN_POINT('Ctrl Pts',(-32.5008538510381,29.7803835826013,51.3713852142718));
#39496=CARTESIAN_POINT('Ctrl Pts',(-30.4069286443211,30.3752922497739,51.4825150034915));
#39497=CARTESIAN_POINT('Ctrl Pts',(-29.7709650654724,32.4571158294164,51.5936447927113));
#39498=CARTESIAN_POINT('Ctrl Pts',(-31.1749900872312,34.1205919617954,51.704774581931));
#39499=CARTESIAN_POINT('Ctrl Pts',(-33.334055231514,33.8433253224467,51.8159043711508));
#39500=CARTESIAN_POINT('Ctrl Pts',(-34.2722075006498,31.879067348231,51.9270341603704));
#39501=CARTESIAN_POINT('Ctrl Pts',(-33.1308600953504,30.0254856052496,52.0381639495902));
#39502=CARTESIAN_POINT('Ctrl Pts',(-30.9545618160425,29.9789580636276,52.1492937388099));
#39503=CARTESIAN_POINT('Ctrl Pts',(-29.735037182646,31.7820661056942,52.2604235280297));
#39504=CARTESIAN_POINT('Ctrl Pts',(-30.5883820418111,33.7846250412173,52.3715533172493));
#39505=CARTESIAN_POINT('Ctrl Pts',(-32.733624180427,34.1539141820779,52.4826831064691));
#39506=CARTESIAN_POINT('Ctrl Pts',(-34.2074617565987,32.5519650362343,52.5938128956888));
#39507=CARTESIAN_POINT('Ctrl Pts',(-33.6610536154475,30.4448622584587,52.7049426849085));
#39508=CARTESIAN_POINT('Ctrl Pts',(-31.5944685187508,29.761007085527,52.8160724741283));
#39509=CARTESIAN_POINT('Ctrl Pts',(-29.8990188623148,31.1262491786764,52.927202263348));
#39510=CARTESIAN_POINT('Ctrl Pts',(-30.1263694539774,33.2911479883563,53.0383320525678));
#39511=CARTESIAN_POINT('Ctrl Pts',(-32.0684363155972,34.2743834714144,53.1494618417874));
#39512=CARTESIAN_POINT('Ctrl Pts',(-33.9478909734479,33.1761648671903,53.2605916310072));
#39513=CARTESIAN_POINT('Ctrl Pts',(-34.0446174001881,31.0014596777944,53.3717214202269));
#39514=CARTESIAN_POINT('Ctrl Pts',(-32.2702104278746,29.7407527886938,53.4828512094466));
#39515=CARTESIAN_POINT('Ctrl Pts',(-30.2483548396889,30.5473973201451,53.5939809986664));
#39516=CARTESIAN_POINT('Ctrl Pts',(-29.8298927061893,32.6840166171813,53.705110787886));
#39517=CARTESIAN_POINT('Ctrl Pts',(-31.3968817262552,34.1935045200403,53.8162405771059));
#39518=CARTESIAN_POINT('Ctrl Pts',(-33.517042143409,33.6977663236515,53.9273703663255));
#39519=CARTESIAN_POINT('Ctrl Pts',(-34.2464204233457,31.6436333230227,54.0385001555453));
#39520=CARTESIAN_POINT('Ctrl Pts',(-33.3653042902589,30.4993465649721,54.1125866816917));
#39521=CARTESIAN_POINT('Ctrl Pts',(-32.7800936946509,30.2399657611256,54.149629944765));
#39522=CARTESIAN_POINT('Ctrl Pts',(-31.5367004230132,30.2652167256662,40.850370055235));
#39523=CARTESIAN_POINT('Ctrl Pts',(-30.9598857617979,30.4192636273712,40.8874133183083));
#39524=CARTESIAN_POINT('Ctrl Pts',(-29.9820228244681,31.3456578491348,40.9614998444547));
#39525=CARTESIAN_POINT('Ctrl Pts',(-30.3559158061516,33.3440431100515,41.0726296336745));
#39526=CARTESIAN_POINT('Ctrl Pts',(-32.2373396060292,34.108469006245,41.1837594228942));
#39527=CARTESIAN_POINT('Ctrl Pts',(-33.900117534767,32.945140990351,41.2948892121139));
#39528=CARTESIAN_POINT('Ctrl Pts',(-33.8246517438579,30.91588019562,41.4060190013336));
#39529=CARTESIAN_POINT('Ctrl Pts',(-32.0789192906661,29.8792733832384,41.5171487905534));
#39530=CARTESIAN_POINT('Ctrl Pts',(-30.2611451993424,30.7832905225872,41.6282785797731));
#39531=CARTESIAN_POINT('Ctrl Pts',(-30.0346590026857,32.8009492386541,41.7394083689928));
#39532=CARTESIAN_POINT('Ctrl Pts',(-31.6068786303459,34.0855261442786,41.8505381582125));
#39533=CARTESIAN_POINT('Ctrl Pts',(-33.5388549034635,33.4614833313175,41.9616679474323));
#39534=CARTESIAN_POINT('Ctrl Pts',(-34.0624998629728,31.4998910672591,42.072797736652));
#39535=CARTESIAN_POINT('Ctrl Pts',(-32.6985612504999,29.9960010331899,42.1839275258717));
#39536=CARTESIAN_POINT('Ctrl Pts',(-30.6953100202696,30.3261451013204,42.2950573150915));
#39537=CARTESIAN_POINT('Ctrl Pts',(-29.8860953635051,32.1881850509407,42.4061871043112));
#39538=CARTESIAN_POINT('Ctrl Pts',(-31.0115040872296,33.8779990571385,42.5173168935309));
#39539=CARTESIAN_POINT('Ctrl Pts',(-33.0415731557818,33.8490892103266,42.6284466827506));
#39540=CARTESIAN_POINT('Ctrl Pts',(-34.1184059669438,32.1279127090986,42.7395764719704));
#39541=CARTESIAN_POINT('Ctrl Pts',(-33.2564965096008,30.2896720158273,42.8507062611901));
#39542=CARTESIAN_POINT('Ctrl Pts',(-31.24465512368,30.0167048791768,42.9618360504098));
#39543=CARTESIAN_POINT('Ctrl Pts',(-29.9240971514974,31.5588279628845,43.0729658396296));
#39544=CARTESIAN_POINT('Ctrl Pts',(-30.5033829670146,33.5047068936161,43.1840956288493));
#39545=CARTESIAN_POINT('Ctrl Pts',(-32.4523564544282,34.0734944017804,43.295225418069));
#39546=CARTESIAN_POINT('Ctrl Pts',(-33.9873382236621,32.7446423152,43.4063552072887));
#39547=CARTESIAN_POINT('Ctrl Pts',(-33.7035296007133,30.7343016592533,43.5174849965085));
#39548=CARTESIAN_POINT('Ctrl Pts',(-31.8606691620459,29.8823143977223,43.6286147857282));
#39549=CARTESIAN_POINT('Ctrl Pts',(-30.1453227948673,30.9684100346118,43.739744574948));
#39550=CARTESIAN_POINT('Ctrl Pts',(-30.1273568929049,32.9986056204144,43.8508743641676));
#39551=CARTESIAN_POINT('Ctrl Pts',(-31.8232136544782,34.1148881719836,43.9620041533874));
#39552=CARTESIAN_POINT('Ctrl Pts',(-33.68086336236,33.2956480034885,44.073133942607));
#39553=CARTESIAN_POINT('Ctrl Pts',(-34.0002051491863,31.2906448329547,44.1842637318269));
#39554=CARTESIAN_POINT('Ctrl Pts',(-32.4889808748128,29.9348358186458,44.2953935210465));
#39555=CARTESIAN_POINT('Ctrl Pts',(-30.5302466065805,30.4690426673488,44.4065233102663));
#39556=CARTESIAN_POINT('Ctrl Pts',(-29.9166147051972,32.4043650643483,44.5176530994859));
#39557=CARTESIAN_POINT('Ctrl Pts',(-31.2096744322432,33.9696169396154,44.6287828887058));
#39558=CARTESIAN_POINT('Ctrl Pts',(-33.226031548177,33.7322967513513,44.7399126779253));
#39559=CARTESIAN_POINT('Ctrl Pts',(-34.1203378869774,31.9095973622274,44.8510424671453));
#39560=CARTESIAN_POINT('Ctrl Pts',(-33.0741339857231,30.1696334868166,44.9621722563649));
#39561=CARTESIAN_POINT('Ctrl Pts',(-31.0448943092331,30.1048011947734,45.0733020455846));
#39562=CARTESIAN_POINT('Ctrl Pts',(-29.889757003243,31.7744342966981,45.1844318348044));
#39563=CARTESIAN_POINT('Ctrl Pts',(-30.6658912032526,33.6505026841267,45.2955616240241));
#39564=CARTESIAN_POINT('Ctrl Pts',(-32.662987306238,34.0160489139987,45.4066914132438));
#39565=CARTESIAN_POINT('Ctrl Pts',(-34.0533246163523,32.5365290409192,45.5178212024636));
#39566=CARTESIAN_POINT('Ctrl Pts',(-33.5644815049592,30.5659836080057,45.6289509916833));
#39567=CARTESIAN_POINT('Ctrl Pts',(-31.643841886323,29.907834425785,45.740080780903));
#39568=CARTESIAN_POINT('Ctrl Pts',(-30.0491543109499,31.1644124884951,45.8512105701227));
#39569=CARTESIAN_POINT('Ctrl Pts',(-30.2398595541551,33.1857111801652,45.9623403593424));
#39570=CARTESIAN_POINT('Ctrl Pts',(-32.0414262454691,34.1218598582504,46.0734701485622));
#39571=CARTESIAN_POINT('Ctrl Pts',(-33.8050800861789,33.1161054046768,46.1845999377819));
#39572=CARTESIAN_POINT('Ctrl Pts',(-33.916744207296,31.0889033884021,46.2957297270016));
#39573=CARTESIAN_POINT('Ctrl Pts',(-32.2742248161213,29.8955271106305,46.4068595162214));
#39574=CARTESIAN_POINT('Ctrl Pts',(-30.3807378470766,30.6281415991517,46.5179893054411));
#39575=CARTESIAN_POINT('Ctrl Pts',(-29.9691820402206,32.6162660189444,46.6291190946608));
#39576=CARTESIAN_POINT('Ctrl Pts',(-31.416208806851,34.0403904613259,46.7402488838805));
#39577=CARTESIAN_POINT('Ctrl Pts',(-33.3975149424995,33.5971716806151,46.8513786731002));
#39578=CARTESIAN_POINT('Ctrl Pts',(-34.0998305581909,31.692238698411,46.96250846232));
#39579=CARTESIAN_POINT('Ctrl Pts',(-32.8804040187402,30.0689655218888,47.0736382515397));
#39580=CARTESIAN_POINT('Ctrl Pts',(-30.8552412689225,30.2129541585371,47.1847680407594));
#39581=CARTESIAN_POINT('Ctrl Pts',(-29.8777492953954,31.9924277695871,47.2958978299792));
#39582=CARTESIAN_POINT('Ctrl Pts',(-30.842518151872,33.7788314037936,47.4070276191988));
#39583=CARTESIAN_POINT('Ctrl Pts',(-32.8666018433873,33.9372678278714,47.5181574084187));
#39584=CARTESIAN_POINT('Ctrl Pts',(-34.0975809257403,32.3227377446762,47.6292871976383));
#39585=CARTESIAN_POINT('Ctrl Pts',(-33.4088766921736,30.4128415774984,47.7404169868581));
#39586=CARTESIAN_POINT('Ctrl Pts',(-31.4307837885612,29.9554955865777,47.8515467760778));
#39587=CARTESIAN_POINT('Ctrl Pts',(-29.9736313887648,31.369257863094,47.9626765652975));
#39588=CARTESIAN_POINT('Ctrl Pts',(-30.3709895669183,33.360268503193,48.0738063545173));
#39589=CARTESIAN_POINT('Ctrl Pts',(-32.2592004275456,34.1063761606675,48.1849361437369));
#39590=CARTESIAN_POINT('Ctrl Pts',(-33.9101938677949,32.9247511985973,48.2960659329567));
#39591=CARTESIAN_POINT('Ctrl Pts',(-33.8129985954281,30.89680396808,48.4071957221764));
#39592=CARTESIAN_POINT('Ctrl Pts',(-32.0565666696766,29.8784897823131,48.5183255113962));
#39593=CARTESIAN_POINT('Ctrl Pts',(-30.2483655412771,30.801758740953,48.6294553006159));
#39594=CARTESIAN_POINT('Ctrl Pts',(-30.0432412738161,32.8216451054873,48.7405850898357));
#39595=CARTESIAN_POINT('Ctrl Pts',(-31.6289213723938,34.0895707798498,48.8517148790553));
#39596=CARTESIAN_POINT('Ctrl Pts',(-33.5542086067766,33.4451439369453,48.9628446682751));
#39597=CARTESIAN_POINT('Ctrl Pts',(-34.0571009789279,31.4781370348818,49.0739744574948));
#39598=CARTESIAN_POINT('Ctrl Pts',(-32.6773568434957,29.9887334591264,49.1851042467145));
#39599=CARTESIAN_POINT('Ctrl Pts',(-30.6777030705251,30.340019210301,49.2962340359342));
#39600=CARTESIAN_POINT('Ctrl Pts',(-29.8882011076971,32.2105013784662,49.407363825154));
#39601=CARTESIAN_POINT('Ctrl Pts',(-31.0313945895992,33.8883349678514,49.5184936143736));
#39602=CARTESIAN_POINT('Ctrl Pts',(-33.0610452390119,33.8379848727991,49.6296234035935));
#39603=CARTESIAN_POINT('Ctrl Pts',(-34.1196387922374,32.105530954277,49.7407531928131));
#39604=CARTESIAN_POINT('Ctrl Pts',(-33.2383619093327,30.2764962508361,49.8518829820329));
#39605=CARTESIAN_POINT('Ctrl Pts',(-31.2237496364824,30.0247934880102,49.9630127712526));
#39606=CARTESIAN_POINT('Ctrl Pts',(-29.9195532782388,31.5807783047347,50.0741425604724));
#39607=CARTESIAN_POINT('Ctrl Pts',(-30.5193591982457,33.5204302706958,50.185272349692));
#39608=CARTESIAN_POINT('Ctrl Pts',(-32.4742315231376,34.0686009412964,50.2964021389119));
#39609=CARTESIAN_POINT('Ctrl Pts',(-33.9950923008799,32.7236104634643,50.4075319281315));
#39610=CARTESIAN_POINT('Ctrl Pts',(-33.6900662407335,30.716379536701,50.5186617173513));
#39611=CARTESIAN_POINT('Ctrl Pts',(-31.8383098850701,29.8839041376594,50.6297915065709));
#39612=CARTESIAN_POINT('Ctrl Pts',(-30.1345305691399,30.9880567237383,50.7409212957907));
#39613=CARTESIAN_POINT('Ctrl Pts',(-30.1380086461482,33.0183288221635,50.8520510850104));
#39614=CARTESIAN_POINT('Ctrl Pts',(-31.8455610177681,34.1166374259014,50.9631808742302));
#39615=CARTESIAN_POINT('Ctrl Pts',(-33.6944542710625,33.2778224113514,51.0743106634499));
#39616=CARTESIAN_POINT('Ctrl Pts',(-33.9926013511572,31.2695581834978,51.1854404526696));
#39617=CARTESIAN_POINT('Ctrl Pts',(-32.4671412833658,29.9297863844823,51.2965702418893));
#39618=CARTESIAN_POINT('Ctrl Pts',(-30.5141585793086,30.4846516364765,51.4077000311091));
#39619=CARTESIAN_POINT('Ctrl Pts',(-29.921001829527,32.426347276272,51.5188298203287));
#39620=CARTESIAN_POINT('Ctrl Pts',(-31.2305216608766,33.9778545147955,51.6299596095485));
#39621=CARTESIAN_POINT('Ctrl Pts',(-33.2442597209519,33.7192507455094,51.7410893987682));
#39622=CARTESIAN_POINT('Ctrl Pts',(-34.1192647829842,31.8872073479497,51.8522191879879));
#39623=CARTESIAN_POINT('Ctrl Pts',(-33.0547416879281,30.1583905435162,51.9633489772077));
#39624=CARTESIAN_POINT('Ctrl Pts',(-31.0249304584134,30.1149947795421,52.0744787664274));
#39625=CARTESIAN_POINT('Ctrl Pts',(-29.8874922593055,31.7967352774389,52.1856085556472));
#39626=CARTESIAN_POINT('Ctrl Pts',(-30.6833983142111,33.6645015913388,52.2967383448669));
#39627=CARTESIAN_POINT('Ctrl Pts',(-32.6842437977518,34.0089338101131,52.4078681340866));
#39628=CARTESIAN_POINT('Ctrl Pts',(-34.0588770872406,32.5148121649961,52.5189979233063));
#39629=CARTESIAN_POINT('Ctrl Pts',(-33.549247781666,30.5495388746866,52.6301277125261));
#39630=CARTESIAN_POINT('Ctrl Pts',(-31.62176491964,29.9117141230998,52.7412575017458));
#39631=CARTESIAN_POINT('Ctrl Pts',(-30.0404363010257,31.1850615121176,52.8523872909655));
#39632=CARTESIAN_POINT('Ctrl Pts',(-30.2524838812592,33.2042405724662,52.9635170801852));
#39633=CARTESIAN_POINT('Ctrl Pts',(-32.0638298542192,34.1212942887441,53.074646869405));
#39634=CARTESIAN_POINT('Ctrl Pts',(-33.8167780627168,33.0969969869859,53.1857766586247));
#39635=CARTESIAN_POINT('Ctrl Pts',(-33.9069938153344,31.0686716161993,53.2969064478444));
#39636=CARTESIAN_POINT('Ctrl Pts',(-32.252022512744,29.8928231468264,53.4080362370641));
#39637=CARTESIAN_POINT('Ctrl Pts',(-30.3662584075308,30.6451722819308,53.5191660262839));
#39638=CARTESIAN_POINT('Ctrl Pts',(-29.975963039575,32.6379753289934,53.6302958155036));
#39639=CARTESIAN_POINT('Ctrl Pts',(-31.4374777316085,34.0458593149211,53.7414256047233));
#39640=CARTESIAN_POINT('Ctrl Pts',(-33.4149297491141,33.5834893505202,53.8525553939431));
#39641=CARTESIAN_POINT('Ctrl Pts',(-34.0952134387425,31.6676204316151,53.9636851831627));
#39642=CARTESIAN_POINT('Ctrl Pts',(-33.2734053996281,30.6003558321987,54.0377717093093));
#39643=CARTESIAN_POINT('Ctrl Pts',(-32.7275854401629,30.3584339994361,54.0748149723825));
#39644=CARTESIAN_POINT('Ctrl Pts',(-31.5701357431141,30.3904122513352,40.7755550828525));
#39645=CARTESIAN_POINT('Ctrl Pts',(-31.0349485380732,30.5333419240918,40.8125983459258));
#39646=CARTESIAN_POINT('Ctrl Pts',(-30.1276558363932,31.3928802951642,40.8866848720723));
#39647=CARTESIAN_POINT('Ctrl Pts',(-30.4745657769798,33.2470464499072,40.997814661292));
#39648=CARTESIAN_POINT('Ctrl Pts',(-32.2202113242556,33.9563053962431,41.1089444505117));
#39649=CARTESIAN_POINT('Ctrl Pts',(-33.7629901960859,32.8769322262541,41.2200742397314));
#39650=CARTESIAN_POINT('Ctrl Pts',(-33.6929706067298,30.9941187576385,41.3312040289512));
#39651=CARTESIAN_POINT('Ctrl Pts',(-32.073223857567,30.0323215982597,41.4423338181709));
#39652=CARTESIAN_POINT('Ctrl Pts',(-30.3866345581869,30.871097792155,41.5534636073906));
#39653=CARTESIAN_POINT('Ctrl Pts',(-30.1764933764186,32.7431464788218,41.6645933966103));
#39654=CARTESIAN_POINT('Ctrl Pts',(-31.6352493422693,33.9350182705907,41.7757231858301));
#39655=CARTESIAN_POINT('Ctrl Pts',(-33.4277991010369,33.3560112665197,41.8868529750498));
#39656=CARTESIAN_POINT('Ctrl Pts',(-33.9136537457907,31.5359828382904,41.9979827642695));
#39657=CARTESIAN_POINT('Ctrl Pts',(-32.6481476084835,30.1406252682755,42.1091125534893));
#39658=CARTESIAN_POINT('Ctrl Pts',(-30.7894666508205,30.4469435589918,42.2202423427089));
#39659=CARTESIAN_POINT('Ctrl Pts',(-30.0386512510881,32.174604146211,42.3313721319287));
#39660=CARTESIAN_POINT('Ctrl Pts',(-31.0828416815284,33.7424679607515,42.4425019211484));
#39661=CARTESIAN_POINT('Ctrl Pts',(-32.9664050926064,33.7156444745371,42.5536317103681));
#39662=CARTESIAN_POINT('Ctrl Pts',(-33.965525228159,32.1186815278368,42.6647614995879));
#39663=CARTESIAN_POINT('Ctrl Pts',(-33.1658178966882,30.4131026565378,42.7758912888076));
#39664=CARTESIAN_POINT('Ctrl Pts',(-31.2991667161373,30.1598349628488,42.8870210780273));
#39665=CARTESIAN_POINT('Ctrl Pts',(-30.0739105329158,31.590666386689,42.9981508672471));
#39666=CARTESIAN_POINT('Ctrl Pts',(-30.6113905544417,33.3961154785897,43.1092806564667));
#39667=CARTESIAN_POINT('Ctrl Pts',(-32.4197108756174,33.9238548327095,43.2204104456866));
#39668=CARTESIAN_POINT('Ctrl Pts',(-33.8439163580755,32.6909031032385,43.3315402349062));
#39669=CARTESIAN_POINT('Ctrl Pts',(-33.5805895845112,30.8256443482523,43.442670024126));
#39670=CARTESIAN_POINT('Ctrl Pts',(-31.8707243647664,30.0351431493602,43.5537998133457));
#39671=CARTESIAN_POINT('Ctrl Pts',(-30.2791708040556,31.042857632708,43.6649296025655));
#39672=CARTESIAN_POINT('Ctrl Pts',(-30.2625014620576,32.9265384305622,43.7760593917851));
#39673=CARTESIAN_POINT('Ctrl Pts',(-31.8359719394964,33.9622613047893,43.8871891810049));
#39674=CARTESIAN_POINT('Ctrl Pts',(-33.5595591191489,33.2021439126441,43.9983189702245));
#39675=CARTESIAN_POINT('Ctrl Pts',(-33.855854705645,31.3418374483886,44.1094487594444));
#39676=CARTESIAN_POINT('Ctrl Pts',(-32.453692191454,30.0838742138751,44.220578548664));
#39677=CARTESIAN_POINT('Ctrl Pts',(-30.6363155037247,30.5795285193129,44.3317083378839));
#39678=CARTESIAN_POINT('Ctrl Pts',(-30.0669680784473,32.3751829194994,44.4428381271034));
#39679=CARTESIAN_POINT('Ctrl Pts',(-31.266710504915,33.8274739804516,44.5539679163233));
#39680=CARTESIAN_POINT('Ctrl Pts',(-33.1375515250919,33.6072806726234,44.6650977055429));
#39681=CARTESIAN_POINT('Ctrl Pts',(-33.9673177257368,31.916121523444,44.7762274947628));
#39682=CARTESIAN_POINT('Ctrl Pts',(-32.99661607846,30.3017270463841,44.8873572839823));
#39683=CARTESIAN_POINT('Ctrl Pts',(-31.1138222040278,30.2415735594704,44.9984870732022));
#39684=CARTESIAN_POINT('Ctrl Pts',(-30.0420486382714,31.7907128815886,45.1096168624219));
#39685=CARTESIAN_POINT('Ctrl Pts',(-30.7621709256707,33.5313895048526,45.2207466516415));
#39686=CARTESIAN_POINT('Ctrl Pts',(-32.6151409581988,33.8705550605032,45.3318764408614));
#39687=CARTESIAN_POINT('Ctrl Pts',(-33.9051406567093,32.4978089101062,45.443006230081));
#39688=CARTESIAN_POINT('Ctrl Pts',(-33.4515762865896,30.6694734436928,45.5541360193008));
#39689=CARTESIAN_POINT('Ctrl Pts',(-31.6695450406724,30.0588214526521,45.6652658085205));
#39690=CARTESIAN_POINT('Ctrl Pts',(-30.189942589897,31.2247150169395,45.7763955977402));
#39691=CARTESIAN_POINT('Ctrl Pts',(-30.3668850515927,33.1001409901083,45.88752538696));
#39692=CARTESIAN_POINT('Ctrl Pts',(-32.0384366036765,33.9687298596622,45.9986551761797));
#39693=CARTESIAN_POINT('Ctrl Pts',(-33.6748113929033,33.0355585116396,46.1097849653994));
#39694=CARTESIAN_POINT('Ctrl Pts',(-33.7784169579181,31.1546552439288,46.2209147546192));
#39695=CARTESIAN_POINT('Ctrl Pts',(-32.2544346091752,30.0474023295923,46.3320445438389));
#39696=CARTESIAN_POINT('Ctrl Pts',(-30.4975964653435,30.7271456281728,46.4431743330586));
#39697=CARTESIAN_POINT('Ctrl Pts',(-30.1157417435415,32.5717914443188,46.5543041222783));
#39698=CARTESIAN_POINT('Ctrl Pts',(-31.4583397441205,33.8931399314442,46.665433911498));
#39699=CARTESIAN_POINT('Ctrl Pts',(-33.2966593368194,33.4819072835595,46.7765637007178));
#39700=CARTESIAN_POINT('Ctrl Pts',(-33.9482903661463,31.7144491603765,46.8876934899375));
#39701=CARTESIAN_POINT('Ctrl Pts',(-32.8168671807052,30.208324068947,46.9988232791572));
#39702=CARTESIAN_POINT('Ctrl Pts',(-30.9378560100384,30.3419213597008,47.109953068377));
#39703=CARTESIAN_POINT('Ctrl Pts',(-30.0309075005126,31.9929742409423,47.2210828575967));
#39704=CARTESIAN_POINT('Ctrl Pts',(-30.9260510925986,33.6504570206823,47.3322126468164));
#39705=CARTESIAN_POINT('Ctrl Pts',(-32.8040610782476,33.7974594335549,47.4433424360362));
#39706=CARTESIAN_POINT('Ctrl Pts',(-33.9462030847635,32.2994464654739,47.5544722252558));
#39707=CARTESIAN_POINT('Ctrl Pts',(-33.3072011337976,30.5273833395529,47.6656020144756));
#39708=CARTESIAN_POINT('Ctrl Pts',(-31.471862881186,30.1030430114104,47.7767318036953));
#39709=CARTESIAN_POINT('Ctrl Pts',(-30.1198699923045,31.4147771475832,47.887861592915));
#39710=CARTESIAN_POINT('Ctrl Pts',(-30.488551697305,33.2621008918102,47.9989913821348));
#39711=CARTESIAN_POINT('Ctrl Pts',(-32.2404944979576,33.9543635867668,48.1101211713545));
#39712=CARTESIAN_POINT('Ctrl Pts',(-33.7723393421336,32.8580139213049,48.2212509605742));
#39713=CARTESIAN_POINT('Ctrl Pts',(-33.6821584406089,30.9764192198383,48.332380749794));
#39714=CARTESIAN_POINT('Ctrl Pts',(-32.0524843764874,30.0315945481044,48.4435105390137));
#39715=CARTESIAN_POINT('Ctrl Pts',(-30.3747771801741,30.888233199477,48.5546403282334));
#39716=CARTESIAN_POINT('Ctrl Pts',(-30.1844562837579,32.7623487700795,48.6657701174531));
#39717=CARTESIAN_POINT('Ctrl Pts',(-31.6557013076947,33.9387710136333,48.7768999066728));
#39718=CARTESIAN_POINT('Ctrl Pts',(-33.4420447610655,33.3408510506062,48.8880296958927));
#39719=CARTESIAN_POINT('Ctrl Pts',(-33.9086444874334,31.5157987469883,48.9991594851123));
#39720=CARTESIAN_POINT('Ctrl Pts',(-32.6284734772899,30.1338821791829,49.110289274332));
#39721=CARTESIAN_POINT('Ctrl Pts',(-30.7731303562417,30.4598164037842,49.2214190635518));
#39722=CARTESIAN_POINT('Ctrl Pts',(-30.0406050283139,32.1953099530466,49.3325488527715));
#39723=CARTESIAN_POINT('Ctrl Pts',(-31.1012967297195,33.752057951329,49.4436786419912));
#39724=CARTESIAN_POINT('Ctrl Pts',(-32.9844719180548,33.7053415128324,49.5548084312109));
#39725=CARTESIAN_POINT('Ctrl Pts',(-33.9666690831396,32.0979150154502,49.6659382204306));
#39726=CARTESIAN_POINT('Ctrl Pts',(-33.1489920309732,30.4008777577721,49.7770680096504));
#39727=CARTESIAN_POINT('Ctrl Pts',(-31.2797699323598,30.1673398344224,49.8881977988701));
#39728=CARTESIAN_POINT('Ctrl Pts',(-30.0696945810809,31.6110326202375,49.9993275880899));
#39729=CARTESIAN_POINT('Ctrl Pts',(-30.6262138159061,33.4107041338354,50.1104573773096));
#39730=CARTESIAN_POINT('Ctrl Pts',(-32.4400072683235,33.9193145225971,50.2215871665293));
#39731=CARTESIAN_POINT('Ctrl Pts',(-33.8511108404508,32.6713890743759,50.332716955749));
#39732=CARTESIAN_POINT('Ctrl Pts',(-33.5680978458599,30.8090156261998,50.4438467449687));
#39733=CARTESIAN_POINT('Ctrl Pts',(-31.8499787080486,30.036618161233,50.5549765341885));
#39734=CARTESIAN_POINT('Ctrl Pts',(-30.2691574297231,31.061086463126,50.6661063234082));
#39735=CARTESIAN_POINT('Ctrl Pts',(-30.2723845014988,32.9448382518538,50.777236112628));
#39736=CARTESIAN_POINT('Ctrl Pts',(-31.8567065423131,33.9638843188666,50.8883659018476));
#39737=CARTESIAN_POINT('Ctrl Pts',(-33.5721692016096,33.1856047546172,50.9994956910675));
#39738=CARTESIAN_POINT('Ctrl Pts',(-33.8487996571372,31.322272576437,51.110625480287));
#39739=CARTESIAN_POINT('Ctrl Pts',(-32.4334287156935,30.0791891863634,51.2217552695069));
#39740=CARTESIAN_POINT('Ctrl Pts',(-30.6213885142961,30.594011023179,51.3328850587265));
#39741=CARTESIAN_POINT('Ctrl Pts',(-30.0710385935816,32.3955787231275,51.4440148479463));
#39742=CARTESIAN_POINT('Ctrl Pts',(-31.286053234522,33.8351170677957,51.555144637166));
#39743=CARTESIAN_POINT('Ctrl Pts',(-33.1544642103899,33.5951761685721,51.6662744263858));
#39744=CARTESIAN_POINT('Ctrl Pts',(-33.9663220653187,31.8953473476683,51.7774042156054));
#39745=CARTESIAN_POINT('Ctrl Pts',(-32.9786232805058,30.291295481783,51.8885340048253));
#39746=CARTESIAN_POINT('Ctrl Pts',(-31.0952991007844,30.2510314954568,51.9996637940449));
#39747=CARTESIAN_POINT('Ctrl Pts',(-30.0399473359648,31.8114044491835,52.1107935832646));
#39748=CARTESIAN_POINT('Ctrl Pts',(-30.778414586611,33.5443781414603,52.2219233724844));
#39749=CARTESIAN_POINT('Ctrl Pts',(-32.6348634150766,33.8639534381483,52.3330531617041));
#39750=CARTESIAN_POINT('Ctrl Pts',(-33.9102924178824,32.4776592937579,52.4441829509238));
#39751=CARTESIAN_POINT('Ctrl Pts',(-33.4374419478845,30.6542154909145,52.5553127401436));
#39752=CARTESIAN_POINT('Ctrl Pts',(-31.6490613205292,30.0624211606725,52.6664425293633));
#39753=CARTESIAN_POINT('Ctrl Pts',(-30.1818537397367,31.2438738455587,52.777572318583));
#39754=CARTESIAN_POINT('Ctrl Pts',(-30.378598308541,33.1173331565761,52.8887021078027));
#39755=CARTESIAN_POINT('Ctrl Pts',(-32.0592233928413,33.9682051060738,52.9998318970225));
#39756=CARTESIAN_POINT('Ctrl Pts',(-33.6856651519856,33.0178291067816,53.1109616862421));
#39757=CARTESIAN_POINT('Ctrl Pts',(-33.7693702304806,31.1358835546042,53.222091475462));
#39758=CARTESIAN_POINT('Ctrl Pts',(-32.2338345976135,30.0448935049591,53.3332212646815));
#39759=CARTESIAN_POINT('Ctrl Pts',(-30.4841619753727,30.7429472437166,53.4443510539014));
#39760=CARTESIAN_POINT('Ctrl Pts',(-30.1220333729607,32.5919340408055,53.555480843121));
#39761=CARTESIAN_POINT('Ctrl Pts',(-31.4780737369618,33.898214109802,53.6666106323408));
#39762=CARTESIAN_POINT('Ctrl Pts',(-33.3128173548192,33.469212377389,53.7777404215606));
#39763=CARTESIAN_POINT('Ctrl Pts',(-33.9440064541393,31.6916075402074,53.8888702107803));
#39764=CARTESIAN_POINT('Ctrl Pts',(-33.1815065089974,30.7013650994253,53.9629567369268));
#39765=CARTESIAN_POINT('Ctrl Pts',(-32.6750771856749,30.4769022377466,54.));
#39766=CARTESIAN_POINT('Ctrl Pts',(-30.3361589164137,32.0009454232939,41.6214803633902));
#39767=CARTESIAN_POINT('Ctrl Pts',(-30.3350387322945,32.2165036755626,41.6358513744636));
#39768=CARTESIAN_POINT('Ctrl Pts',(-30.3739091166134,32.4316746076715,41.6502223855369));
#39769=CARTESIAN_POINT('Ctrl Pts',(-30.4546429010218,32.6297836630055,41.6645933966103));
#39770=CARTESIAN_POINT('Ctrl Pts',(-30.6627453650355,33.1404370760781,41.7016366596836));
#39771=CARTESIAN_POINT('Ctrl Pts',(-31.1489973536524,33.5377276733344,41.7386799227568));
#39772=CARTESIAN_POINT('Ctrl Pts',(-31.6908816410888,33.6398718046173,41.7757231858301));
#39773=CARTESIAN_POINT('Ctrl Pts',(-32.2327659285252,33.7420159359003,41.8127664489033));
#39774=CARTESIAN_POINT('Ctrl Pts',(-32.830282514781,33.54901360121,41.8498097119766));
#39775=CARTESIAN_POINT('Ctrl Pts',(-33.2100165820346,33.1491743624933,41.8868529750498));
#39776=CARTESIAN_POINT('Ctrl Pts',(-33.5897506492881,32.7493351237766,41.9238962381231));
#39777=CARTESIAN_POINT('Ctrl Pts',(-33.7517021975394,32.1426589810335,41.9609395011963));
#39778=CARTESIAN_POINT('Ctrl Pts',(-33.6217602821139,31.6067613146595,41.9979827642695));
#39779=CARTESIAN_POINT('Ctrl Pts',(-33.4918183666883,31.0708636482855,42.0350260273428));
#39780=CARTESIAN_POINT('Ctrl Pts',(-33.0699829875859,30.6057444582805,42.072069290416));
#39781=CARTESIAN_POINT('Ctrl Pts',(-32.5492851384242,30.4242379117307,42.1091125534893));
#39782=CARTESIAN_POINT('Ctrl Pts',(-32.0285872892625,30.242731365181,42.1461558165625));
#39783=CARTESIAN_POINT('Ctrl Pts',(-31.4090269700415,30.3448374620864,42.1831990796357));
#39784=CARTESIAN_POINT('Ctrl Pts',(-30.9741109104756,30.6838339417423,42.220242342709));
#39785=CARTESIAN_POINT('Ctrl Pts',(-30.5779071442121,30.9926560213956,42.2539883496027));
#39786=CARTESIAN_POINT('Ctrl Pts',(-30.3349398414768,31.4980736765861,42.2877343564965));
#39787=CARTESIAN_POINT('Ctrl Pts',(-30.3317921991812,32.000855278924,42.3214803633902));
#39788=CARTESIAN_POINT('Ctrl Pts',(-31.4698297828114,30.0148256743283,41.));
#39789=CARTESIAN_POINT('Ctrl Pts',(-31.4011629084353,30.0402504721211,41.));
#39790=CARTESIAN_POINT('Ctrl Pts',(-31.3341993832291,30.0695646102219,41.));
#39791=CARTESIAN_POINT('Ctrl Pts',(-31.2691281870165,30.1024741661484,41.));
#39792=CARTESIAN_POINT('Ctrl Pts',(-31.2022478796466,30.136298674439,41.));
#39793=CARTESIAN_POINT('Ctrl Pts',(-31.1373658136216,30.1739219879674,41.));
#39794=CARTESIAN_POINT('Ctrl Pts',(-31.0747183883007,30.2150696221828,41.));
#39795=CARTESIAN_POINT('Ctrl Pts',(-31.0217877302761,30.2498351587395,41.));
#39796=CARTESIAN_POINT('Ctrl Pts',(-30.9704526091484,30.2871175891263,41.));
#39797=CARTESIAN_POINT('Ctrl Pts',(-30.9208783414071,30.3267693724872,41.));
#39798=CARTESIAN_POINT('Ctrl Pts',(-30.8988476211705,30.3443905575476,41.));
#39799=CARTESIAN_POINT('Ctrl Pts',(-30.877164954821,30.3624798447009,41.));
#39800=CARTESIAN_POINT('Ctrl Pts',(-30.8558464048857,30.3810250092555,41.));
#39801=CARTESIAN_POINT('Ctrl Pts',(-30.8441323268764,30.3912151725146,41.));
#39802=CARTESIAN_POINT('Ctrl Pts',(-30.8325282028598,30.4015429837462,41.));
#39803=CARTESIAN_POINT('Ctrl Pts',(-30.8210368319428,30.4120064565416,41.));
#39804=CARTESIAN_POINT('Ctrl Pts',(-30.8104448512627,30.421650989165,41.));
#39805=CARTESIAN_POINT('Ctrl Pts',(-30.799947233707,30.4314122915714,41.));
#39806=CARTESIAN_POINT('Ctrl Pts',(-30.7895620525903,30.4412733595479,41.));
#39807=CARTESIAN_POINT('Ctrl Pts',(-30.7364770065195,30.4916793411058,41.));
#39808=CARTESIAN_POINT('Ctrl Pts',(-30.6862319428219,30.5447736155129,41.));
#39809=CARTESIAN_POINT('Ctrl Pts',(-30.6390455537104,30.6002968491221,41.));
#39810=CARTESIAN_POINT('Ctrl Pts',(-30.5922257365251,30.6553887452401,41.));
#39811=CARTESIAN_POINT('Ctrl Pts',(-30.5484167469741,30.7128728910456,41.));
#39812=CARTESIAN_POINT('Ctrl Pts',(-30.5078770105767,30.7725201905801,41.));
#39813=CARTESIAN_POINT('Ctrl Pts',(-30.4741908999485,30.8220835501218,41.));
#39814=CARTESIAN_POINT('Ctrl Pts',(-30.4427627290454,30.8731411370933,41.));
#39815=CARTESIAN_POINT('Ctrl Pts',(-30.4137683610081,30.9255679879711,41.));
#39816=CARTESIAN_POINT('Ctrl Pts',(-30.4016604837945,30.9474611319191,41.));
#39817=CARTESIAN_POINT('Ctrl Pts',(-30.3899773466439,30.9695930938703,41.));
#39818=CARTESIAN_POINT('Ctrl Pts',(-30.3787331983111,30.9919548569239,41.));
#39819=CARTESIAN_POINT('Ctrl Pts',(-30.3735336034124,31.0022955341953,41.));
#39820=CARTESIAN_POINT('Ctrl Pts',(-30.3684278936195,31.0126853517444,41.));
#39821=CARTESIAN_POINT('Ctrl Pts',(-30.363417543091,31.0231234159713,41.));
#39822=CARTESIAN_POINT('Ctrl Pts',(-30.3581837446205,31.0340269893391,41.));
#39823=CARTESIAN_POINT('Ctrl Pts',(-30.3530576063202,31.0449757645301,41.));
#39824=CARTESIAN_POINT('Ctrl Pts',(-30.348042198309,31.0559644120955,41.));
#39825=CARTESIAN_POINT('Ctrl Pts',(-30.3195018402902,31.1184957026626,41.));
#39826=CARTESIAN_POINT('Ctrl Pts',(-30.2945224741136,31.182360381032,41.));
#39827=CARTESIAN_POINT('Ctrl Pts',(-30.2733275766249,31.2473541148403,41.));
#39828=CARTESIAN_POINT('Ctrl Pts',(-30.2541304118743,31.3062218407325,41.));
#39829=CARTESIAN_POINT('Ctrl Pts',(-30.2380382479865,31.3660164111607,41.));
#39830=CARTESIAN_POINT('Ctrl Pts',(-30.2252538021287,31.4265908222046,41.));
#39831=CARTESIAN_POINT('Ctrl Pts',(-30.2101196168207,31.4982986124253,41.));
#39832=CARTESIAN_POINT('Ctrl Pts',(-30.1996201783637,31.5711007701871,41.));
#39833=CARTESIAN_POINT('Ctrl Pts',(-30.1936803374547,31.644574102922,41.));
#39834=CARTESIAN_POINT('Ctrl Pts',(-30.192373397395,31.6607404015391,41.));
#39835=CARTESIAN_POINT('Ctrl Pts',(-30.1912874246838,31.6769391120234,41.));
#39836=CARTESIAN_POINT('Ctrl Pts',(-30.1904219877599,31.6931655622086,41.));
#39837=CARTESIAN_POINT('Ctrl Pts',(-30.1895243490928,31.7099957767667,41.));
#39838=CARTESIAN_POINT('Ctrl Pts',(-30.1888639529652,31.72686206175,41.));
#39839=CARTESIAN_POINT('Ctrl Pts',(-30.1884408807954,31.7437248028176,41.));
#39840=CARTESIAN_POINT('Ctrl Pts',(-30.1867207010254,31.8122874455965,41.));
#39841=CARTESIAN_POINT('Ctrl Pts',(-30.1889121483104,31.8808779859611,41.));
#39842=CARTESIAN_POINT('Ctrl Pts',(-30.1948946421042,31.9491579840471,41.));
#39843=CARTESIAN_POINT('Ctrl Pts',(-30.2008758629234,32.0174234532929,41.));
#39844=CARTESIAN_POINT('Ctrl Pts',(-30.2106469707899,32.0853795842456,41.));
#39845=CARTESIAN_POINT('Ctrl Pts',(-30.2241370660968,32.1526731205519,41.));
#39846=CARTESIAN_POINT('Ctrl Pts',(-30.2338950540172,32.2013495382838,41.));
#39847=CARTESIAN_POINT('Ctrl Pts',(-30.2455999681403,32.2496790024792,41.));
#39848=CARTESIAN_POINT('Ctrl Pts',(-30.2592391639345,32.2975181738642,41.));
#39849=CARTESIAN_POINT('Ctrl Pts',(-30.269473786622,32.333415881925,41.));
#39850=CARTESIAN_POINT('Ctrl Pts',(-30.2807978036095,32.3690373637504,41.));
#39851=CARTESIAN_POINT('Ctrl Pts',(-30.293209784769,32.404317881334,41.));
#39852=CARTESIAN_POINT('Ctrl Pts',(-30.2973424899566,32.4160649164095,41.));
#39853=CARTESIAN_POINT('Ctrl Pts',(-30.3015926249635,32.4277649816303,41.));
#39854=CARTESIAN_POINT('Ctrl Pts',(-30.3059595224773,32.4394154501761,41.));
#39855=CARTESIAN_POINT('Ctrl Pts',(-30.3290832908114,32.501107471751,41.));
#39856=CARTESIAN_POINT('Ctrl Pts',(-30.355479582176,32.5614159713376,41.));
#39857=CARTESIAN_POINT('Ctrl Pts',(-30.3850984013863,32.6200067698823,41.));
#39858=CARTESIAN_POINT('Ctrl Pts',(-30.4059238288755,32.6612028222288,41.));
#39859=CARTESIAN_POINT('Ctrl Pts',(-30.4283432331492,32.7015491648088,41.));
#39860=CARTESIAN_POINT('Ctrl Pts',(-30.4523496254102,32.7409183022664,41.));
#39861=CARTESIAN_POINT('Ctrl Pts',(-30.4600634641435,32.7535685653344,41.));
#39862=CARTESIAN_POINT('Ctrl Pts',(-30.4679423056765,32.7661195241672,41.));
#39863=CARTESIAN_POINT('Ctrl Pts',(-30.4759826277317,32.7785613658112,41.));
#39864=CARTESIAN_POINT('Ctrl Pts',(-30.5102255857725,32.8315499722927,41.));
#39865=CARTESIAN_POINT('Ctrl Pts',(-30.5473242553461,32.8824546989078,41.));
#39866=CARTESIAN_POINT('Ctrl Pts',(-30.5872443914682,32.9309602517629,41.));
#39867=CARTESIAN_POINT('Ctrl Pts',(-30.6240203591527,32.9756454361735,41.));
#39868=CARTESIAN_POINT('Ctrl Pts',(-30.6631914372638,33.0182945811671,41.));
#39869=CARTESIAN_POINT('Ctrl Pts',(-30.7047522727162,33.0586283114149,41.));
#39870=CARTESIAN_POINT('Ctrl Pts',(-30.7125941112345,33.0662386155871,41.));
#39871=CARTESIAN_POINT('Ctrl Pts',(-30.720521081831,33.073766383874,41.));
#39872=CARTESIAN_POINT('Ctrl Pts',(-30.728531577822,33.081210944453,41.));
#39873=CARTESIAN_POINT('Origin',(-32.,32.,48.));
#39874=CARTESIAN_POINT('Origin',(32.,32.,54.));
#39875=CARTESIAN_POINT('Ctrl Pts',(31.3249228143251,30.4769022377466,54.));
#39876=CARTESIAN_POINT('Ctrl Pts',(31.2652392925755,30.4954885225906,54.));
#39877=CARTESIAN_POINT('Ctrl Pts',(31.2068683211469,30.5176493909919,54.));
#39878=CARTESIAN_POINT('Ctrl Pts',(31.1499664526549,30.5430859698249,54.));
#39879=CARTESIAN_POINT('Ctrl Pts',(31.1138836855836,30.5592158821362,54.));
#39880=CARTESIAN_POINT('Ctrl Pts',(31.0783916111174,30.5766640975224,54.));
#39881=CARTESIAN_POINT('Ctrl Pts',(31.0435310469341,30.5953648451471,54.));
#39882=CARTESIAN_POINT('Ctrl Pts',(31.0197684746904,30.6081121393132,54.));
#39883=CARTESIAN_POINT('Ctrl Pts',(30.996299346444,30.6214415774298,54.));
#39884=CARTESIAN_POINT('Ctrl Pts',(30.9731370541742,30.6353342860965,54.));
#39885=CARTESIAN_POINT('Ctrl Pts',(30.9607881815602,30.6427411216371,54.));
#39886=CARTESIAN_POINT('Ctrl Pts',(30.9485266882192,30.6503081374092,54.));
#39887=CARTESIAN_POINT('Ctrl Pts',(30.9363666889478,30.6580245755571,54.));
#39888=CARTESIAN_POINT('Ctrl Pts',(30.8806648540549,30.6933715977137,54.));
#39889=CARTESIAN_POINT('Ctrl Pts',(30.8270267921164,30.7318880347813,54.));
#39890=CARTESIAN_POINT('Ctrl Pts',(30.7756343274519,30.773271408358,54.));
#39891=CARTESIAN_POINT('Ctrl Pts',(30.7385655425372,30.8031207526961,54.));
#39892=CARTESIAN_POINT('Ctrl Pts',(30.7026651301385,30.8344628590285,54.));
#39893=CARTESIAN_POINT('Ctrl Pts',(30.6680066073461,30.8672000886409,54.));
#39894=CARTESIAN_POINT('Ctrl Pts',(30.6585374859811,30.876144289818,54.));
#39895=CARTESIAN_POINT('Ctrl Pts',(30.6491610994594,30.8851926993893,54.));
#39896=CARTESIAN_POINT('Ctrl Pts',(30.639879031127,30.8943434783427,54.));
#39897=CARTESIAN_POINT('Ctrl Pts',(30.6303154851562,30.9037717535995,54.));
#39898=CARTESIAN_POINT('Ctrl Pts',(30.6208577720802,30.9133031307529,54.));
#39899=CARTESIAN_POINT('Ctrl Pts',(30.6115111155573,30.922931187383,54.));
#39900=CARTESIAN_POINT('Ctrl Pts',(30.5642487582623,30.9716164740835,54.));
#39901=CARTESIAN_POINT('Ctrl Pts',(30.5197932859356,31.0228006877741,54.));
#39902=CARTESIAN_POINT('Ctrl Pts',(30.4783284042593,31.0761767372777,54.));
#39903=CARTESIAN_POINT('Ctrl Pts',(30.436264293657,31.1303241497162,54.));
#39904=CARTESIAN_POINT('Ctrl Pts',(30.3972769445889,31.1867277877173,54.));
#39905=CARTESIAN_POINT('Ctrl Pts',(30.3615825003683,31.2451139635999,54.));
#39906=CARTESIAN_POINT('Ctrl Pts',(30.3394718058714,31.2812809057101,54.));
#39907=CARTESIAN_POINT('Ctrl Pts',(30.3186251627735,31.3182094602772,54.));
#39908=CARTESIAN_POINT('Ctrl Pts',(30.2991008591822,31.3558418492927,54.));
#39909=CARTESIAN_POINT('Ctrl Pts',(30.2831165799908,31.3866509693133,54.));
#39910=CARTESIAN_POINT('Ctrl Pts',(30.2680186762366,31.417931948164,54.));
#39911=CARTESIAN_POINT('Ctrl Pts',(30.2538424561611,31.4496552941849,54.));
#39912=CARTESIAN_POINT('Ctrl Pts',(30.2480304578859,31.4626613022304,54.));
#39913=CARTESIAN_POINT('Ctrl Pts',(30.2423725282932,31.4757441614276,54.));
#39914=CARTESIAN_POINT('Ctrl Pts',(30.2368802697065,31.4888793524524,54.));
#39915=CARTESIAN_POINT('Ctrl Pts',(30.209689682674,31.5539078920073,54.));
#39916=CARTESIAN_POINT('Ctrl Pts',(30.1865048065016,31.6203282670227,54.));
#39917=CARTESIAN_POINT('Ctrl Pts',(30.1675372143216,31.6878453452323,54.));
#39918=CARTESIAN_POINT('Ctrl Pts',(30.165437190741,31.695320593276,54.));
#39919=CARTESIAN_POINT('Ctrl Pts',(30.1633888988524,31.7028093234633,54.));
#39920=CARTESIAN_POINT('Ctrl Pts',(30.1613926538322,31.7103111628798,54.));
#39921=CARTESIAN_POINT('Ctrl Pts',(30.1440545227347,31.7754674307538,54.));
#39922=CARTESIAN_POINT('Ctrl Pts',(30.1306386910357,31.8416105480239,54.));
#39923=CARTESIAN_POINT('Ctrl Pts',(30.1209911133228,31.9084360573021,54.));
#39924=CARTESIAN_POINT('Ctrl Pts',(30.1106126487227,31.9803241729591,54.));
#39925=CARTESIAN_POINT('Ctrl Pts',(30.1045944012331,32.0530027832628,54.));
#39926=CARTESIAN_POINT('Ctrl Pts',(30.1028047404686,32.1261154066584,54.));
#39927=CARTESIAN_POINT('Ctrl Pts',(30.1024846698419,32.139191182611,54.));
#39928=CARTESIAN_POINT('Ctrl Pts',(30.1023000105237,32.1522808750456,54.));
#39929=CARTESIAN_POINT('Ctrl Pts',(30.1022502162009,32.1653824793981,54.));
#39930=CARTESIAN_POINT('Ctrl Pts',(30.1022052492636,32.1772139290201,54.));
#39931=CARTESIAN_POINT('Ctrl Pts',(30.1022703199631,32.1890464872063,54.));
#39932=CARTESIAN_POINT('Ctrl Pts',(30.1024444765937,32.2008751816772,54.));
#39933=CARTESIAN_POINT('Ctrl Pts',(30.1034907073006,32.2719350278467,54.));
#39934=CARTESIAN_POINT('Ctrl Pts',(30.1084695156064,32.3428927641364,54.));
#39935=CARTESIAN_POINT('Ctrl Pts',(30.1172007707484,32.413412787761,54.));
#39936=CARTESIAN_POINT('Ctrl Pts',(30.1261162611738,32.4854208307286,54.));
#39937=CARTESIAN_POINT('Ctrl Pts',(30.1389441735648,32.5569734294332,54.));
#39938=CARTESIAN_POINT('Ctrl Pts',(30.1555454304087,32.6277294754119,54.));
#39939=CARTESIAN_POINT('Ctrl Pts',(30.1722476063644,32.6989156476985,54.));
#39940=CARTESIAN_POINT('Ctrl Pts',(30.1927692213023,32.7692966238086,54.));
#39941=CARTESIAN_POINT('Ctrl Pts',(30.2170210478913,32.8385259647519,54.));
#39942=CARTESIAN_POINT('Ctrl Pts',(30.2230020581078,32.8555993754471,54.));
#39943=CARTESIAN_POINT('Ctrl Pts',(30.2292101918566,32.8726027019187,54.));
#39944=CARTESIAN_POINT('Ctrl Pts',(30.2356445879338,32.8895306376608,54.));
#39945=CARTESIAN_POINT('Ctrl Pts',(30.2407135830383,32.9028664072306,54.));
#39946=CARTESIAN_POINT('Ctrl Pts',(30.2459237771072,32.9161569899756,54.));
#39947=CARTESIAN_POINT('Ctrl Pts',(30.2512663088271,32.9293795887561,54.));
#39948=CARTESIAN_POINT('Ctrl Pts',(30.2794914917943,32.9992360331264,54.));
#39949=CARTESIAN_POINT('Ctrl Pts',(30.3114529069637,33.0673215315237,54.));
#39950=CARTESIAN_POINT('Ctrl Pts',(30.3469924470567,33.1332787426213,54.));
#39951=CARTESIAN_POINT('Ctrl Pts',(30.3825709958759,33.1993083493318,54.));
#39952=CARTESIAN_POINT('Ctrl Pts',(30.4217357000898,33.2632061094673,54.));
#39953=CARTESIAN_POINT('Ctrl Pts',(30.4643796980224,33.3246090804382,54.));
#39954=CARTESIAN_POINT('Ctrl Pts',(30.5060535747287,33.3846151766228,54.));
#39955=CARTESIAN_POINT('Ctrl Pts',(30.5510505813055,33.4422396847995,54.));
#39956=CARTESIAN_POINT('Ctrl Pts',(30.5993163191418,33.4971242544356,54.));
#39957=CARTESIAN_POINT('Ctrl Pts',(30.6096515303738,33.5088767655541,54.));
#39958=CARTESIAN_POINT('Ctrl Pts',(30.6201367787392,33.5205035406757,54.));
#39959=CARTESIAN_POINT('Ctrl Pts',(30.6307717865001,33.5320008742866,54.));
#39960=CARTESIAN_POINT('Ctrl Pts',(30.6398828337217,33.5418506789889,54.));
#39961=CARTESIAN_POINT('Ctrl Pts',(30.6491037972993,33.5516054798596,54.));
#39962=CARTESIAN_POINT('Ctrl Pts',(30.6584328166059,33.5612648614874,54.));
#39963=CARTESIAN_POINT('Ctrl Pts',(31.6163320011532,34.0186125009919,54.));
#39964=CARTESIAN_POINT('Ctrl Pts',(31.6906496900554,34.0256330925326,54.));
#39965=CARTESIAN_POINT('Ctrl Pts',(31.7652154809392,34.0282517372431,54.));
#39966=CARTESIAN_POINT('Ctrl Pts',(31.8397072565627,34.0266320313122,54.));
#39967=CARTESIAN_POINT('Ctrl Pts',(31.9122409523519,34.0250549007326,54.));
#39968=CARTESIAN_POINT('Ctrl Pts',(31.9847052554167,34.0194586585716,54.));
#39969=CARTESIAN_POINT('Ctrl Pts',(32.0567895869437,34.009950480074,54.));
#39970=CARTESIAN_POINT('Ctrl Pts',(32.0728797642137,34.0078281287349,54.));
#39971=CARTESIAN_POINT('Ctrl Pts',(32.0889530628615,34.0055103754858,54.));
#39972=CARTESIAN_POINT('Ctrl Pts',(32.1049990603174,34.0029992289119,54.));
#39973=CARTESIAN_POINT('Ctrl Pts',(32.1786326365799,33.9914758129782,54.));
#39974=CARTESIAN_POINT('Ctrl Pts',(32.2515465637322,33.9759078826664,54.));
#39975=CARTESIAN_POINT('Ctrl Pts',(32.3234089085464,33.9564349301845,54.));
#39976=CARTESIAN_POINT('Ctrl Pts',(32.3738561644734,33.9427649473854,54.));
#39977=CARTESIAN_POINT('Ctrl Pts',(32.4237849247872,33.9271694712033,54.));
#39978=CARTESIAN_POINT('Ctrl Pts',(32.4730724197954,33.9096836167836,54.));
#39979=CARTESIAN_POINT('Ctrl Pts',(32.4917998071078,33.9030396522617,54.));
#39980=CARTESIAN_POINT('Ctrl Pts',(32.5104345309238,33.896122668595,54.));
#39981=CARTESIAN_POINT('Ctrl Pts',(32.5289695229777,33.8889342296203,54.));
#39982=CARTESIAN_POINT('Ctrl Pts',(32.5466571100482,33.8820744403149,54.));
#39983=CARTESIAN_POINT('Ctrl Pts',(32.5642593377296,33.874964996238,54.));
#39984=CARTESIAN_POINT('Ctrl Pts',(32.5817391496632,33.8676204838936,54.));
#39985=CARTESIAN_POINT('Ctrl Pts',(32.6486663172982,33.8394996201947,54.));
#39986=CARTESIAN_POINT('Ctrl Pts',(32.7138733597198,33.8079107127814,54.));
#39987=CARTESIAN_POINT('Ctrl Pts',(32.7770520704153,33.7729809129467,54.));
#39988=CARTESIAN_POINT('Ctrl Pts',(32.8388737816019,33.7388013614265,54.));
#39989=CARTESIAN_POINT('Ctrl Pts',(32.8987540539514,33.7014222659878,54.));
#39990=CARTESIAN_POINT('Ctrl Pts',(32.9563717527268,33.6609259427107,54.));
#39991=CARTESIAN_POINT('Ctrl Pts',(33.0127259983595,33.6213176314161,54.));
#39992=CARTESIAN_POINT('Ctrl Pts',(33.0669163726691,33.5787267777315,54.));
#39993=CARTESIAN_POINT('Ctrl Pts',(33.1186019715482,33.5332031777472,54.));
#39994=CARTESIAN_POINT('Ctrl Pts',(33.1354287832063,33.5183824721823,54.));
#39995=CARTESIAN_POINT('Ctrl Pts',(33.1519897538664,33.5032507388309,54.));
#39996=CARTESIAN_POINT('Ctrl Pts',(33.1682720164058,33.4878091927252,54.));
#39997=CARTESIAN_POINT('Ctrl Pts',(33.1774026318648,33.4791500263936,54.));
#39998=CARTESIAN_POINT('Ctrl Pts',(33.1864464242868,33.4703924724357,54.));
#39999=CARTESIAN_POINT('Ctrl Pts',(33.1953886696531,33.4615493621301,54.));
#40000=CARTESIAN_POINT('Ctrl Pts',(33.2439541235006,33.4135223121193,54.));
#40001=CARTESIAN_POINT('Ctrl Pts',(33.2896152685707,33.3628927157441,54.));
#40002=CARTESIAN_POINT('Ctrl Pts',(33.332079740635,33.3097415636927,54.));
#40003=CARTESIAN_POINT('Ctrl Pts',(33.3381856709119,33.3020990048009,54.));
#40004=CARTESIAN_POINT('Ctrl Pts',(33.3442254363888,33.2944042619705,54.));
#40005=CARTESIAN_POINT('Ctrl Pts',(33.3501980920418,33.2866575274568,54.));
#40006=CARTESIAN_POINT('Ctrl Pts',(33.3925565636038,33.2317171704926,54.));
#40007=CARTESIAN_POINT('Ctrl Pts',(33.4315436482843,33.1741631439773,54.));
#40008=CARTESIAN_POINT('Ctrl Pts',(33.4670921079473,33.1143576586055,54.));
#40009=CARTESIAN_POINT('Ctrl Pts',(33.5002539400628,33.058567351957,54.));
#40010=CARTESIAN_POINT('Ctrl Pts',(33.5304229661912,33.0008167747747,54.));
#40011=CARTESIAN_POINT('Ctrl Pts',(33.557504889555,32.9413945291346,54.));
#40012=CARTESIAN_POINT('Ctrl Pts',(33.563398708835,32.9284625090446,54.));
#40013=CARTESIAN_POINT('Ctrl Pts',(33.5691461688042,32.9154513223191,54.));
#40014=CARTESIAN_POINT('Ctrl Pts',(33.5747460519361,32.9023639711173,54.));
#40015=CARTESIAN_POINT('Ctrl Pts',(33.5792733485958,32.8917833357747,54.));
#40016=CARTESIAN_POINT('Ctrl Pts',(33.5837039631642,32.8811532170269,54.));
#40017=CARTESIAN_POINT('Ctrl Pts',(33.588032228022,32.870488236425,54.));
#40018=CARTESIAN_POINT('Ctrl Pts',(33.6137449952032,32.8071311702053,54.));
#40019=CARTESIAN_POINT('Ctrl Pts',(33.6359004658581,32.7424283875045,54.));
#40020=CARTESIAN_POINT('Ctrl Pts',(33.6544523724797,32.6767299554583,54.));
#40021=CARTESIAN_POINT('Ctrl Pts',(33.6729186410861,32.6113347959239,54.));
#40022=CARTESIAN_POINT('Ctrl Pts',(33.6878145454425,32.5449520220622,54.));
#40023=CARTESIAN_POINT('Ctrl Pts',(33.6990433939503,32.4779242445738,54.));
#40024=CARTESIAN_POINT('Ctrl Pts',(33.7100316622983,32.4123325496376,54.));
#40025=CARTESIAN_POINT('Ctrl Pts',(33.7175081962818,32.3461222296304,54.));
#40026=CARTESIAN_POINT('Ctrl Pts',(33.7213344983069,32.2796272244155,54.));
#40027=CARTESIAN_POINT('Ctrl Pts',(33.7224477961555,32.2602798896349,54.));
#40028=CARTESIAN_POINT('Ctrl Pts',(33.7232517671042,32.2409085892293,54.));
#40029=CARTESIAN_POINT('Ctrl Pts',(33.7237422384393,32.2215219353351,54.));
#40030=CARTESIAN_POINT('Ctrl Pts',(33.72401437674,32.2107652393375,54.));
#40031=CARTESIAN_POINT('Ctrl Pts',(33.7241897483875,32.2000135675735,54.));
#40032=CARTESIAN_POINT('Ctrl Pts',(33.7242681224748,32.1892683767583,54.));
#40033=CARTESIAN_POINT('Ctrl Pts',(33.7247442520814,32.1239903792229,54.));
#40034=CARTESIAN_POINT('Ctrl Pts',(33.7216445871738,32.0589495683597,54.));
#40035=CARTESIAN_POINT('Ctrl Pts',(33.7148888928212,31.9944557738682,54.));
#40036=CARTESIAN_POINT('Ctrl Pts',(33.7079758523754,31.9284598618934,54.));
#40037=CARTESIAN_POINT('Ctrl Pts',(33.6972346951092,31.8630356000403,54.));
#40038=CARTESIAN_POINT('Ctrl Pts',(33.6825255118463,31.798535704284,54.));
#40039=CARTESIAN_POINT('Ctrl Pts',(33.668893202805,31.7387579112976,54.));
#40040=CARTESIAN_POINT('Ctrl Pts',(33.6518520502579,31.6797736424106,54.));
#40041=CARTESIAN_POINT('Ctrl Pts',(33.6312489013858,31.6218918727598,54.));
#40042=CARTESIAN_POINT('Ctrl Pts',(33.6296213708013,31.6173195449581,54.));
#40043=CARTESIAN_POINT('Ctrl Pts',(33.6279715922876,31.6127541143676,54.));
#40044=CARTESIAN_POINT('Ctrl Pts',(33.6262994796833,31.6081957426667,54.));
#40045=CARTESIAN_POINT('Ctrl Pts',(33.6225368250294,31.5979383123658,54.));
#40046=CARTESIAN_POINT('Ctrl Pts',(33.6186610809759,31.587716623037,54.));
#40047=CARTESIAN_POINT('Ctrl Pts',(33.614673303851,31.5775320375437,54.));
#40048=CARTESIAN_POINT('Origin',(32.,32.,39.4540747194623));
#40049=CARTESIAN_POINT('Ctrl Pts',(34.0565678449602,32.0014926321758,41.2040747194623));
#40050=CARTESIAN_POINT('Ctrl Pts',(34.0573842294279,32.0995827500376,41.2094078928854));
#40051=CARTESIAN_POINT('Ctrl Pts',(34.0064118509519,32.8781629596678,41.2517843293816));
#40052=CARTESIAN_POINT('Ctrl Pts',(33.0117215203461,34.2080087873732,41.3312040289512));
#40053=CARTESIAN_POINT('Ctrl Pts',(30.693930615665,34.0473906585599,41.4423338181709));
#40054=CARTESIAN_POINT('Ctrl Pts',(29.5714562640958,32.0133707418711,41.5534636073906));
#40055=CARTESIAN_POINT('Ctrl Pts',(30.6715507113449,29.9669383183226,41.6645933966104));
#40056=CARTESIAN_POINT('Ctrl Pts',(32.9874316286532,29.7812306730564,41.7757231858301));
#40057=CARTESIAN_POINT('Ctrl Pts',(34.0018420245732,31.1064228934244,41.8555502934474));
#40058=CARTESIAN_POINT('Ctrl Pts',(34.0572700743595,31.8927563372387,41.8983341379915));
#40059=CARTESIAN_POINT('Ctrl Pts',(34.0563620767522,31.9983919833491,41.9040747194623));
#40060=CARTESIAN_POINT('Ctrl Pts',(34.052676219088,31.9976391197375,41.1459252805377));
#40061=CARTESIAN_POINT('Ctrl Pts',(34.0491258389796,32.4677617736048,41.1713700465049));
#40062=CARTESIAN_POINT('Ctrl Pts',(33.6566798069838,33.6293344104736,41.2338580755454));
#40063=CARTESIAN_POINT('Ctrl Pts',(31.7284038427318,34.4127959913661,41.3333893676592));
#40064=CARTESIAN_POINT('Ctrl Pts',(29.8256278405404,33.0815586024407,41.4445191568789));
#40065=CARTESIAN_POINT('Ctrl Pts',(29.9119860164316,30.7594030366271,41.5556489460986));
#40066=CARTESIAN_POINT('Ctrl Pts',(31.9096898523802,29.5731770382926,41.6667787353184));
#40067=CARTESIAN_POINT('Ctrl Pts',(33.7208347882445,30.4738973185028,41.7635375134647));
#40068=CARTESIAN_POINT('Ctrl Pts',(34.0499076510441,31.5817394238508,41.8232530285378));
#40069=CARTESIAN_POINT('Ctrl Pts',(34.0520872716434,32.0011660295939,41.8459252805377));
#40070=CARTESIAN_POINT('Ctrl Pts',(30.7309291201476,33.0793586530485,41.));
#40071=CARTESIAN_POINT('Ctrl Pts',(30.3720428517593,32.6573931542737,41.0370432630732));
#40072=CARTESIAN_POINT('Ctrl Pts',(30.114703984369,31.4343794756361,41.1111297892197));
#40073=CARTESIAN_POINT('Ctrl Pts',(31.4546599251405,30.1066751817884,41.2222595784394));
#40074=CARTESIAN_POINT('Ctrl Pts',(33.2938434714149,30.5162236027394,41.3333893676592));
#40075=CARTESIAN_POINT('Ctrl Pts',(33.9488200232574,32.2815049853891,41.4445191568789));
#40076=CARTESIAN_POINT('Ctrl Pts',(32.8203080924183,33.7902628737138,41.5556489460987));
#40077=CARTESIAN_POINT('Ctrl Pts',(30.9410334131636,33.6600330148003,41.6667787353184));
#40078=CARTESIAN_POINT('Ctrl Pts',(30.0309264562519,32.010841054122,41.7779085245381));
#40079=CARTESIAN_POINT('Ctrl Pts',(30.9228876919823,30.3515849803264,41.8890383137579));
#40080=CARTESIAN_POINT('Ctrl Pts',(32.8006137453881,30.2010124352413,42.0001681029775));
#40081=CARTESIAN_POINT('Ctrl Pts',(33.9456251072274,31.6968174418197,42.1112978921973));
#40082=CARTESIAN_POINT('Ctrl Pts',(33.3100223159796,33.4701102033079,42.222427681417));
#40083=CARTESIAN_POINT('Ctrl Pts',(31.4755008806028,33.897964772512,42.3335574706367));
#40084=CARTESIAN_POINT('Ctrl Pts',(30.1209955671039,32.5888272504792,42.4446872598565));
#40085=CARTESIAN_POINT('Ctrl Pts',(30.4861346246503,30.740799047359,42.5558170490762));
#40086=CARTESIAN_POINT('Ctrl Pts',(32.2367469115823,30.0451790962689,42.6669468382959));
#40087=CARTESIAN_POINT('Ctrl Pts',(33.7706909646394,31.1385894331762,42.7780766275156));
#40088=CARTESIAN_POINT('Ctrl Pts',(33.6841178632491,33.0203536843011,42.8892064167355));
#40089=CARTESIAN_POINT('Ctrl Pts',(32.0562583498155,33.9683011547304,43.000336205955));
#40090=CARTESIAN_POINT('Ctrl Pts',(30.3769118083114,33.1148808315266,43.1114659951749));
#40091=CARTESIAN_POINT('Ctrl Pts',(30.1829979763716,31.2411336223703,43.2225957843945));
#40092=CARTESIAN_POINT('Ctrl Pts',(31.6519846928047,30.0618927123183,43.3337255736143));
#40093=CARTESIAN_POINT('Ctrl Pts',(33.4394712438521,30.6563865640221,43.444855362834));
#40094=CARTESIAN_POINT('Ctrl Pts',(33.909569323175,32.4805408665194,43.5559851520537));
#40095=CARTESIAN_POINT('Ctrl Pts',(32.6320502662273,33.8649093766671,43.6671149412734));
#40096=CARTESIAN_POINT('Ctrl Pts',(30.7760856599876,33.5425330506821,43.7782447304932));
#40097=CARTESIAN_POINT('Ctrl Pts',(30.0402341848989,31.8084472041341,43.8893745197128));
#40098=CARTESIAN_POINT('Ctrl Pts',(31.0979391310306,30.2496683993889,44.0005043089327));
#40099=CARTESIAN_POINT('Ctrl Pts',(32.9812004019927,30.2927740938005,44.1116340981523));
#40100=CARTESIAN_POINT('Ctrl Pts',(33.9664777057302,31.8983144235561,44.2227638873721));
#40101=CARTESIAN_POINT('Ctrl Pts',(33.1520559387442,33.5969162900964,44.3338936765918));
#40102=CARTESIAN_POINT('Ctrl Pts',(31.2832850701469,33.8340376857981,44.4450234658115));
#40103=CARTESIAN_POINT('Ctrl Pts',(30.0704439329009,32.3926676807569,44.5561532550313));
#40104=CARTESIAN_POINT('Ctrl Pts',(30.6235115831001,30.5919324725962,44.667283044251));
#40105=CARTESIAN_POINT('Ctrl Pts',(32.4363265050506,30.0798453956562,44.7784128334707));
#40106=CARTESIAN_POINT('Ctrl Pts',(33.8498201413429,31.3250629894034,44.8895426226904));
#40107=CARTESIAN_POINT('Ctrl Pts',(33.5703784447421,33.1879756158609,45.0006724119101));
#40108=CARTESIAN_POINT('Ctrl Pts',(31.8537434255585,33.9636658417418,45.1118022011299));
#40109=CARTESIAN_POINT('Ctrl Pts',(30.2709608372172,32.9422303843299,45.2229319903496));
#40110=CARTESIAN_POINT('Ctrl Pts',(30.2705761400058,31.0584758972423,45.3340617795693));
#40111=CARTESIAN_POINT('Ctrl Pts',(31.8529414046403,30.0363940585948,45.4451915687891));
#40112=CARTESIAN_POINT('Ctrl Pts',(33.5698931009639,30.8113830831017,45.5563213580088));
#40113=CARTESIAN_POINT('Ctrl Pts',(33.8500956560671,32.6741814199402,45.6674511472285));
#40114=CARTESIAN_POINT('Ctrl Pts',(32.4371107301896,33.9199762324424,45.7785809364483));
#40115=CARTESIAN_POINT('Ctrl Pts',(30.6240868043111,33.4086296182887,45.8897107256679));
#40116=CARTESIAN_POINT('Ctrl Pts',(30.0702837139698,31.6081204534292,46.0008405148878));
#40117=CARTESIAN_POINT('Ctrl Pts',(31.2825360417016,30.1662551998346,46.1119703041074));
#40118=CARTESIAN_POINT('Ctrl Pts',(33.1514036034955,30.4026133012171,46.2231000933272));
#40119=CARTESIAN_POINT('Ctrl Pts',(33.9665190738225,32.1008823863883,46.3342298825469));
#40120=CARTESIAN_POINT('Ctrl Pts',(32.9818976137984,33.7068250055609,46.4453596717666));
#40121=CARTESIAN_POINT('Ctrl Pts',(31.0986541058623,33.7506998893905,46.5564894609863));
#40122=CARTESIAN_POINT('Ctrl Pts',(30.0403125855518,32.1923532199997,46.6676192502061));
#40123=CARTESIAN_POINT('Ctrl Pts',(30.7754557350193,30.457966969649,46.7787490394258));
#40124=CARTESIAN_POINT('Ctrl Pts',(32.6312885161675,30.1348326260236,46.8898788286455));
#40125=CARTESIAN_POINT('Ctrl Pts',(33.9093728933581,31.5186792361636,47.0010086178653));
#40126=CARTESIAN_POINT('Ctrl Pts',(33.4400199048342,33.3430253896603,47.112138407085));
#40127=CARTESIAN_POINT('Ctrl Pts',(31.6527763157716,33.9382492710438,47.2232681963047));
#40128=CARTESIAN_POINT('Ctrl Pts',(30.1833080770308,32.7596084390061,47.3343979855245));
#40129=CARTESIAN_POINT('Ctrl Pts',(30.3764565849878,30.8857822012005,47.4455277747441));
#40130=CARTESIAN_POINT('Ctrl Pts',(32.0554544197689,30.0316760096674,47.5566575639639));
#40131=CARTESIAN_POINT('Ctrl Pts',(33.6837009709555,30.9789585885018,47.6677873531836));
#40132=CARTESIAN_POINT('Ctrl Pts',(33.7710426525005,32.8606871944064,47.7789171424033));
#40133=CARTESIAN_POINT('Ctrl Pts',(32.2375453046347,33.9547242137542,47.890046931623));
#40134=CARTESIAN_POINT('Ctrl Pts',(30.4866490700389,33.2598188307756,48.0011767208428));
#40135=CARTESIAN_POINT('Ctrl Pts',(30.120755194936,31.4119409160375,48.1123065100625));
#40136=CARTESIAN_POINT('Ctrl Pts',(31.4747257858664,30.1022482977067,48.2234362992822));
#40137=CARTESIAN_POINT('Ctrl Pts',(33.3094216412102,30.5293574570545,48.334566088502));
#40138=CARTESIAN_POINT('Ctrl Pts',(33.9457490106048,32.3023827232517,48.4456958777217));
#40139=CARTESIAN_POINT('Ctrl Pts',(32.8013479862633,33.7986706003332,48.5568256669415));
#40140=CARTESIAN_POINT('Ctrl Pts',(30.9235619751506,33.64883464976,48.6679554561611));
#40141=CARTESIAN_POINT('Ctrl Pts',(30.0309203708958,31.9900031085938,48.7790852453808));
#40142=CARTESIAN_POINT('Ctrl Pts',(30.9403590894178,30.3403206140307,48.8902150346006));
#40143=CARTESIAN_POINT('Ctrl Pts',(32.8195696779774,30.2095586950333,49.0013448238203));
#40144=CARTESIAN_POINT('Ctrl Pts',(33.9487189851152,31.717389241814,49.1124746130401));
#40145=CARTESIAN_POINT('Ctrl Pts',(33.2944218100529,33.4838620897005,49.2236044022597));
#40146=CARTESIAN_POINT('Ctrl Pts',(31.4554838318502,33.8923204449074,49.3347341914795));
#40147=CARTESIAN_POINT('Ctrl Pts',(30.1148811457062,32.5689476502957,49.4458639806992));
#40148=CARTESIAN_POINT('Ctrl Pts',(30.4995187917492,30.7248801361138,49.5569937699189));
#40149=CARTESIAN_POINT('Ctrl Pts',(32.2573805675422,30.0477884932614,49.6681235591387));
#40150=CARTESIAN_POINT('Ctrl Pts',(33.7796904390966,31.1573396505239,49.7792533483584));
#40151=CARTESIAN_POINT('Ctrl Pts',(33.673246920729,33.038084421356,49.8903831375781));
#40152=CARTESIAN_POINT('Ctrl Pts',(32.0354659661174,33.9687855873198,50.0015129267978));
#40153=CARTESIAN_POINT('Ctrl Pts',(30.3652269439276,33.0976755343592,50.1126427160176));
#40154=CARTESIAN_POINT('Ctrl Pts',(30.1911144942798,31.2219847361484,50.2237725052373));
#40155=CARTESIAN_POINT('Ctrl Pts',(31.6724744429204,30.0583250701906,50.334902294457));
#40156=CARTESIAN_POINT('Ctrl Pts',(33.4535822295341,30.6716652434062,50.4460320836768));
#40157=CARTESIAN_POINT('Ctrl Pts',(33.9043873231198,32.5006829806665,50.5571618728964));
#40158=CARTESIAN_POINT('Ctrl Pts',(32.6123177908093,33.8714810837004,50.6682916621163));
#40159=CARTESIAN_POINT('Ctrl Pts',(30.7598616566552,33.5295199943014,50.7794214513359));
#40160=CARTESIAN_POINT('Ctrl Pts',(30.0423666855995,31.7877587930665,50.8905512405557));
#40161=CARTESIAN_POINT('Ctrl Pts',(31.1164764942148,30.2402384427668,51.0016810297754));
#40162=CARTESIAN_POINT('Ctrl Pts',(32.9991774339491,30.3032327858082,51.1128108189951));
#40163=CARTESIAN_POINT('Ctrl Pts',(33.9674420216862,31.9190900826419,51.2239406082149));
#40164=CARTESIAN_POINT('Ctrl Pts',(33.135125007345,33.6089952583346,51.3350703974345));
#40165=CARTESIAN_POINT('Ctrl Pts',(31.2639538959055,33.8263654225762,51.4462001866543));
#40166=CARTESIAN_POINT('Ctrl Pts',(30.0664041974282,32.3722657578878,51.557329975874));
#40167=CARTESIAN_POINT('Ctrl Pts',(30.638460407338,30.5774725092217,51.6684597650938));
#40168=CARTESIAN_POINT('Ctrl Pts',(32.4565828894534,30.0845609922851,51.7795895543135));
#40169=CARTESIAN_POINT('Ctrl Pts',(33.8568456580557,31.3446384854398,51.8907193435332));
#40170=CARTESIAN_POINT('Ctrl Pts',(33.5577434260076,33.2044957250635,52.0018491327529));
#40171=CARTESIAN_POINT('Ctrl Pts',(31.833011285784,33.9620115483424,52.1129789219727));
#40172=CARTESIAN_POINT('Ctrl Pts',(30.2611054409688,32.9239156618485,52.2241087111923));
#40173=CARTESIAN_POINT('Ctrl Pts',(30.2806169696143,31.0402622164347,52.3352385004122));
#40174=CARTESIAN_POINT('Ctrl Pts',(31.873689339204,30.034950312623,52.4463682896318));
#40175=CARTESIAN_POINT('Ctrl Pts',(33.5823595836263,30.8280307111899,52.5574980788517));
#40176=CARTESIAN_POINT('Ctrl Pts',(33.842872035858,32.6936844190747,52.6686278680713));
#40177=CARTESIAN_POINT('Ctrl Pts',(32.4168069193824,33.9244862123967,52.7797576572911));
#40178=CARTESIAN_POINT('Ctrl Pts',(30.6092867419366,33.3940180191776,52.8908874465107));
#40179=CARTESIAN_POINT('Ctrl Pts',(30.0745280763313,31.5877617807645,53.0020172357305));
#40180=CARTESIAN_POINT('Ctrl Pts',(31.3019487101277,30.1587772763281,53.1131470249502));
#40181=CARTESIAN_POINT('Ctrl Pts',(33.1682019308355,30.4148681833194,53.2242768141699));
#40182=CARTESIAN_POINT('Ctrl Pts',(33.9653618476556,32.1216380242729,53.3354066033897));
#40183=CARTESIAN_POINT('Ctrl Pts',(32.9637797039416,33.7171187586807,53.4465363926094));
#40184=CARTESIAN_POINT('Ctrl Pts',(31.0802839463425,33.7410463011958,53.5576661818291));
#40185=CARTESIAN_POINT('Ctrl Pts',(30.038250683241,32.1717152925075,53.6687959710489));
#40186=CARTESIAN_POINT('Ctrl Pts',(30.7920873980091,30.4449785577687,53.7799257602685));
#40187=CARTESIAN_POINT('Ctrl Pts',(32.6504055030379,30.1418837476604,53.8910555494883));
#40188=CARTESIAN_POINT('Ctrl Pts',(33.9154419463401,31.538310911213,54.002185338708));
#40189=CARTESIAN_POINT('Ctrl Pts',(33.4235043307428,33.3593759834911,54.1133151279278));
#40190=CARTESIAN_POINT('Ctrl Pts',(32.2331222331376,33.7401334029927,54.1874016540742));
#40191=CARTESIAN_POINT('Ctrl Pts',(31.6889203620495,33.6366995627948,54.2244449171475));
#40192=CARTESIAN_POINT('Ctrl Pts',(30.6322193753411,33.1633123698097,40.9251850276175));
#40193=CARTESIAN_POINT('Ctrl Pts',(30.2454185337564,32.7085259251269,40.9622282906908));
#40194=CARTESIAN_POINT('Ctrl Pts',(29.9680635629852,31.3903848820294,41.0363148168373));
#40195=CARTESIAN_POINT('Ctrl Pts',(31.412242767457,29.9594102712082,41.1474446060569));
#40196=CARTESIAN_POINT('Ctrl Pts',(33.3944800559513,30.4008138239409,41.2585743952767));
#40197=CARTESIAN_POINT('Ctrl Pts',(34.1004014126213,32.3034007563114,41.3697041844964));
#40198=CARTESIAN_POINT('Ctrl Pts',(32.8841125683943,33.9295115116003,41.4808339737162));
#40199=CARTESIAN_POINT('Ctrl Pts',(30.8586658139974,33.7891522293869,41.5919637629359));
#40200=CARTESIAN_POINT('Ctrl Pts',(29.8777697255332,32.0116842833717,41.7030935521556));
#40201=CARTESIAN_POINT('Ctrl Pts',(30.8391086984365,30.2233694263251,41.8142233413754));
#40202=CARTESIAN_POINT('Ctrl Pts',(32.8628863731431,30.0610851811797,41.925353130595));
#40203=CARTESIAN_POINT('Ctrl Pts',(34.0969579924684,31.6732355651705,42.0364829198148));
#40204=CARTESIAN_POINT('Ctrl Pts',(33.4119173090442,33.5844570103379,42.1476127090345));
#40205=CARTESIAN_POINT('Ctrl Pts',(31.4347047556197,34.0455905838994,42.2587424982542));
#40206=CARTESIAN_POINT('Ctrl Pts',(29.9748445120241,32.6346268890594,42.369872287474));
#40207=CARTESIAN_POINT('Ctrl Pts',(30.3683844916637,30.6428569964709,42.4810020766937));
#40208=CARTESIAN_POINT('Ctrl Pts',(32.2551613497331,29.893130951746,42.5921318659135));
#40209=CARTESIAN_POINT('Ctrl Pts',(33.9084172776653,31.0715879610168,42.7032616551331));
#40210=CARTESIAN_POINT('Ctrl Pts',(33.815110424141,33.0997179289533,42.8143914443529));
#40211=CARTESIAN_POINT('Ctrl Pts',(32.0606341868485,34.1213978081722,42.9255212335726));
#40212=CARTESIAN_POINT('Ctrl Pts',(30.2506662031655,33.2015975028463,43.0366510227923));
#40213=CARTESIAN_POINT('Ctrl Pts',(30.0416695376591,31.1821081513212,43.147780812012));
#40214=CARTESIAN_POINT('Ctrl Pts',(31.6249156750632,29.9111445714447,43.2589106012318));
#40215=CARTESIAN_POINT('Ctrl Pts',(33.5514349185315,30.5518788162757,43.3700403904515));
#40216=CARTESIAN_POINT('Ctrl Pts',(34.0580977494224,32.5179178696926,43.4811701796712));
#40217=CARTESIAN_POINT('Ctrl Pts',(32.6812118390555,34.0099641025933,43.592299968891));
#40218=CARTESIAN_POINT('Ctrl Pts',(30.680888241084,33.6625129873473,43.7034297581107));
#40219=CARTESIAN_POINT('Ctrl Pts',(29.8878014196687,31.7935480145797,43.8145595473304));
#40220=CARTESIAN_POINT('Ctrl Pts',(31.0277758331491,30.1135256603458,43.9256893365501));
#40221=CARTESIAN_POINT('Ctrl Pts',(33.0575192607911,30.1599841636214,44.0368191257698));
#40222=CARTESIAN_POINT('Ctrl Pts',(34.1194325292802,31.8904052063007,44.1479489149897));
#40223=CARTESIAN_POINT('Ctrl Pts',(33.2416641312585,33.7211262156216,44.2590787042093));
#40224=CARTESIAN_POINT('Ctrl Pts',(31.227538185597,33.9766911772654,44.3702084934291));
#40225=CARTESIAN_POINT('Ctrl Pts',(29.920360915477,32.4232098097874,44.4813382826487));
#40226=CARTESIAN_POINT('Ctrl Pts',(30.516446782766,30.4824114139171,44.5924680718685));
#40227=CARTESIAN_POINT('Ctrl Pts',(32.4702644660027,29.930493634464,44.7035978610882));
#40228=CARTESIAN_POINT('Ctrl Pts',(33.9937012097596,31.2725656378889,44.814727650308));
#40229=CARTESIAN_POINT('Ctrl Pts',(33.6925242271338,33.28037768082,44.9258574395276));
#40230=CARTESIAN_POINT('Ctrl Pts',(31.8423674264961,34.1164019553827,45.0369872287474));
#40231=CARTESIAN_POINT('Ctrl Pts',(30.1364742476751,33.0155181118025,45.1481170179671));
#40232=CARTESIAN_POINT('Ctrl Pts',(30.1360596282866,30.985243105136,45.2592468071869));
#40233=CARTESIAN_POINT('Ctrl Pts',(31.8415030234986,29.8836626040688,45.3703765964065));
#40234=CARTESIAN_POINT('Ctrl Pts',(33.6920011327766,30.7189311370344,45.4815063856263));
#40235=CARTESIAN_POINT('Ctrl Pts',(33.9939981543256,32.7266200007729,45.592636174846));
#40236=CARTESIAN_POINT('Ctrl Pts',(32.4711096890454,34.0693141196697,45.7037659640657));
#40237=CARTESIAN_POINT('Ctrl Pts',(30.5170667453227,33.5181943970221,45.8148957532855));
#40238=CARTESIAN_POINT('Ctrl Pts',(29.9201882345391,31.5776396263525,45.9260255425052));
#40239=CARTESIAN_POINT('Ctrl Pts',(31.226730896886,30.0236244893375,46.0371553317249));
#40240=CARTESIAN_POINT('Ctrl Pts',(33.2409610566485,30.278366786781,46.1482851209446));
#40241=CARTESIAN_POINT('Ctrl Pts',(34.1194771150287,32.1087291306277,46.2594149101644));
#40242=CARTESIAN_POINT('Ctrl Pts',(33.0582707025067,33.8395837532423,46.3705446993841));
#40243=CARTESIAN_POINT('Ctrl Pts',(31.0285464195185,33.8868712743446,46.4816744886038));
#40244=CARTESIAN_POINT('Ctrl Pts',(29.8878859184116,32.2073146674336,46.5928042778236));
#40245=CARTESIAN_POINT('Ctrl Pts',(30.6802093198509,30.3380259251214,46.7039340670433));
#40246=CARTESIAN_POINT('Ctrl Pts',(32.6803908392287,29.9897578327796,46.815063856263));
#40247=CARTESIAN_POINT('Ctrl Pts',(34.0578860410758,31.4812415717095,46.9261936454828));
#40248=CARTESIAN_POINT('Ctrl Pts',(33.5520262549751,33.4474873985099,47.0373234347025));
#40249=CARTESIAN_POINT('Ctrl Pts',(31.6257688713451,34.0890084555412,47.1484532239222));
#40250=CARTESIAN_POINT('Ctrl Pts',(30.0420037582924,32.8186916284146,47.2595830131419));
#40251=CARTESIAN_POINT('Ctrl Pts',(30.2501755720655,30.7991171013039,47.3707128023616));
#40252=CARTESIAN_POINT('Ctrl Pts',(32.0597677262285,29.8785775800472,47.4818425915814));
#40253=CARTESIAN_POINT('Ctrl Pts',(33.8146611055012,30.8995408516631,47.5929723808011));
#40254=CARTESIAN_POINT('Ctrl Pts',(33.9087963201994,32.9276324018544,47.7041021700208));
#40255=CARTESIAN_POINT('Ctrl Pts',(32.2560218426853,34.1067648376231,47.8152319592405));
#40256=CARTESIAN_POINT('Ctrl Pts',(30.3689389511868,33.3578089409124,47.9263617484603));
#40257=CARTESIAN_POINT('Ctrl Pts',(29.9745854434417,31.3662010263035,48.03749153768));
#40258=CARTESIAN_POINT('Ctrl Pts',(31.4338693731524,29.9546390591579,48.1486213268997));
#40259=CARTESIAN_POINT('Ctrl Pts',(33.4112699131231,30.4149692440553,48.2597511161195));
#40260=CARTESIAN_POINT('Ctrl Pts',(34.0970915331884,32.3259023878504,48.3708809053391));
#40261=CARTESIAN_POINT('Ctrl Pts',(32.8636777240904,33.9385732005491,48.482010694559));
#40262=CARTESIAN_POINT('Ctrl Pts',(30.8398354280997,33.7770828430561,48.5931404837786));
#40263=CARTESIAN_POINT('Ctrl Pts',(29.8777631668513,31.9892255392592,48.7042702729984));
#40264=CARTESIAN_POINT('Ctrl Pts',(30.8579390406005,30.211228905088,48.815400062218));
#40265=CARTESIAN_POINT('Ctrl Pts',(32.8833167192567,30.0702961785655,48.9265298514379));
#40266=CARTESIAN_POINT('Ctrl Pts',(34.1002925156201,31.6954074626534,49.0376596406576));
#40267=CARTESIAN_POINT('Ctrl Pts',(33.3951033784119,33.5992785337523,49.1487894298773));
#40268=CARTESIAN_POINT('Ctrl Pts',(31.4131307585472,34.0395072342147,49.259919219097));
#40269=CARTESIAN_POINT('Ctrl Pts',(29.9682545041283,32.6132010314587,49.3710490083168));
#40270=CARTESIAN_POINT('Ctrl Pts',(30.3828096941687,30.6256998946,49.4821787975364));
#40271=CARTESIAN_POINT('Ctrl Pts',(32.2773999144073,29.8959433105394,49.5933085867562));
#40272=CARTESIAN_POINT('Ctrl Pts',(33.9181167412572,31.0917965911284,49.7044383759758));
#40273=CARTESIAN_POINT('Ctrl Pts',(33.8033939276184,33.1188277824609,49.8155681651957));
#40274=CARTESIAN_POINT('Ctrl Pts',(32.0382245484159,34.1219199204672,49.9266979544153));
#40275=CARTESIAN_POINT('Ctrl Pts',(30.2380724770312,33.1830539585253,50.0378277436352));
#40276=CARTESIAN_POINT('Ctrl Pts',(30.0504173673593,31.1614698434269,50.1489575328547));
#40277=CARTESIAN_POINT('Ctrl Pts',(31.6469991407365,29.9072994341435,50.2600873220747));
#40278=CARTESIAN_POINT('Ctrl Pts',(33.5666434723775,30.568345888339,50.3712171112942));
#40279=CARTESIAN_POINT('Ctrl Pts',(34.0525126876382,32.539626659885,50.4823469005141));
#40280=CARTESIAN_POINT('Ctrl Pts',(32.6599445497484,34.0170469643103,50.5934766897337));
#40281=CARTESIAN_POINT('Ctrl Pts',(30.6634023167241,33.648487760965,50.7046064789535));
#40282=CARTESIAN_POINT('Ctrl Pts',(29.8900997886462,31.7712504358846,50.8157362681732));
#40283=CARTESIAN_POINT('Ctrl Pts',(31.0477550530635,30.1033622312073,50.926866057393));
#40284=CARTESIAN_POINT('Ctrl Pts',(33.0768945662916,30.1712563443283,51.0379958466126));
#40285=CARTESIAN_POINT('Ctrl Pts',(34.120471850804,31.912796819262,51.1491256358324));
#40286=CARTESIAN_POINT('Ctrl Pts',(33.2234162931804,33.7341446994465,51.260255425052));
#40287=CARTESIAN_POINT('Ctrl Pts',(31.2067034111182,33.9684221568752,51.3713852142719));
#40288=CARTESIAN_POINT('Ctrl Pts',(29.9160069648852,32.4012210026614,51.4825150034915));
#40289=CARTESIAN_POINT('Ctrl Pts',(30.5325583431829,30.4668267385054,51.5936447927113));
#40290=CARTESIAN_POINT('Ctrl Pts',(32.4920964145184,29.9355760154445,51.7047745819309));
#40291=CARTESIAN_POINT('Ctrl Pts',(34.001273178978,31.2936637377837,51.8159043711508));
#40292=CARTESIAN_POINT('Ctrl Pts',(33.6789064425863,33.2981827424942,51.9270341603704));
#40293=CARTESIAN_POINT('Ctrl Pts',(31.8200227178265,34.1146189892024,52.0381639495902));
#40294=CARTESIAN_POINT('Ctrl Pts',(30.1258522877428,32.9957788498324,52.1492937388099));
#40295=CARTESIAN_POINT('Ctrl Pts',(30.1468814447919,30.9656127439735,52.2604235280297));
#40296=CARTESIAN_POINT('Ctrl Pts',(31.8638647554936,29.8821065619291,52.3715533172493));
#40297=CARTESIAN_POINT('Ctrl Pts',(33.7054372723287,30.7368736361549,52.4826831064692));
#40298=CARTESIAN_POINT('Ctrl Pts',(33.9862126729008,32.7476399648761,52.5938128956888));
#40299=CARTESIAN_POINT('Ctrl Pts',(32.4492266252468,34.074174890882,52.7049426849086));
#40300=CARTESIAN_POINT('Ctrl Pts',(30.5011155176325,33.5024462914775,52.8160724741282));
#40301=CARTESIAN_POINT('Ctrl Pts',(29.9247627281268,31.5556974334801,52.927202263348));
#40302=CARTESIAN_POINT('Ctrl Pts',(31.2476535042578,30.0155649246219,53.0383320525677));
#40303=CARTESIAN_POINT('Ctrl Pts',(33.2590659765762,30.291574867246,53.1494618417874));
#40304=CARTESIAN_POINT('Ctrl Pts',(34.1182298785232,32.1310991651164,53.2605916310072));
#40305=CARTESIAN_POINT('Ctrl Pts',(33.0387435614661,33.850678165931,53.3717214202268));
#40306=CARTESIAN_POINT('Ctrl Pts',(31.0087474085555,33.876466819321,53.4828512094467));
#40307=CARTESIAN_POINT('Ctrl Pts',(29.8856636390453,32.1850714989825,53.5939809986663));
#40308=CARTESIAN_POINT('Ctrl Pts',(30.6981346120899,30.3240272601162,53.7051107878861));
#40309=CARTESIAN_POINT('Ctrl Pts',(32.7009947666045,29.9973573985013,53.8162405771057));
#40310=CARTESIAN_POINT('Ctrl Pts',(34.0644271517501,31.5024002202835,53.9273703663256));
#40311=CARTESIAN_POINT('Ctrl Pts',(33.5342260811582,33.465109759718,54.0385001555452));
#40312=CARTESIAN_POINT('Ctrl Pts',(32.2512547397667,33.8754829148801,54.1125866816917));
#40313=CARTESIAN_POINT('Ctrl Pts',(31.6647242417507,33.7640038755272,54.149629944765));
#40314=CARTESIAN_POINT('Ctrl Pts',(30.5335096305347,33.2472660865709,40.850370055235));
#40315=CARTESIAN_POINT('Ctrl Pts',(30.1187942157535,32.75965869598,40.8874133183083));
#40316=CARTESIAN_POINT('Ctrl Pts',(29.8214231416013,31.3463902884227,40.9614998444548));
#40317=CARTESIAN_POINT('Ctrl Pts',(31.3698256097737,29.812145360628,41.0726296336744));
#40318=CARTESIAN_POINT('Ctrl Pts',(33.4951166404876,30.2854040451424,41.1837594228943));
#40319=CARTESIAN_POINT('Ctrl Pts',(34.2519828019854,32.3252965272338,41.2948892121139));
#40320=CARTESIAN_POINT('Ctrl Pts',(32.9479170443701,34.0687601494867,41.4060190013337));
#40321=CARTESIAN_POINT('Ctrl Pts',(30.7762982148312,33.9182714439734,41.5171487905533));
#40322=CARTESIAN_POINT('Ctrl Pts',(29.7246129948145,32.0125275126214,41.6282785797731));
#40323=CARTESIAN_POINT('Ctrl Pts',(30.7553297048906,30.0951538723239,41.7394083689928));
#40324=CARTESIAN_POINT('Ctrl Pts',(32.9251590008982,29.9211579271181,41.8505381582126));
#40325=CARTESIAN_POINT('Ctrl Pts',(34.2482908777094,31.6496536885213,41.9616679474323));
#40326=CARTESIAN_POINT('Ctrl Pts',(33.5138123021089,33.698803817368,42.072797736652));
#40327=CARTESIAN_POINT('Ctrl Pts',(31.3939086306365,34.1932163952868,42.1839275258717));
#40328=CARTESIAN_POINT('Ctrl Pts',(29.8286934569445,32.6804265276396,42.2950573150915));
#40329=CARTESIAN_POINT('Ctrl Pts',(30.250634358677,30.5449149455827,42.4061871043112));
#40330=CARTESIAN_POINT('Ctrl Pts',(32.2735757878839,29.7410828072231,42.5173168935309));
#40331=CARTESIAN_POINT('Ctrl Pts',(34.0461435906913,31.0045864888574,42.6284466827506));
#40332=CARTESIAN_POINT('Ctrl Pts',(33.946102985033,33.1790821736056,42.7395764719704));
#40333=CARTESIAN_POINT('Ctrl Pts',(32.0650100238815,34.2744944616138,42.8507062611901));
#40334=CARTESIAN_POINT('Ctrl Pts',(30.1244205980196,33.288314174166,42.9618360504099));
#40335=CARTESIAN_POINT('Ctrl Pts',(29.9003410989465,31.1230826802721,43.0729658396295));
#40336=CARTESIAN_POINT('Ctrl Pts',(31.5978466573217,29.7603964305711,43.1840956288493));
#40337=CARTESIAN_POINT('Ctrl Pts',(33.6633985932109,30.4473710685293,43.295225418069));
#40338=CARTESIAN_POINT('Ctrl Pts',(34.2066261756697,32.5552948728657,43.4063552072888));
#40339=CARTESIAN_POINT('Ctrl Pts',(32.7303734118838,34.1550188285196,43.5174849965084));
#40340=CARTESIAN_POINT('Ctrl Pts',(30.5856908221805,33.7824929240125,43.6286147857282));
#40341=CARTESIAN_POINT('Ctrl Pts',(29.7353686544384,31.7786488250253,43.7397445749479));
#40342=CARTESIAN_POINT('Ctrl Pts',(30.9576125352676,29.9773829213026,43.8508743641677));
#40343=CARTESIAN_POINT('Ctrl Pts',(33.1338381195896,30.0271942334423,43.9620041533873));
#40344=CARTESIAN_POINT('Ctrl Pts',(34.2723873528301,31.8824959890453,44.0731339426071));
#40345=CARTESIAN_POINT('Ctrl Pts',(33.3312723237729,33.8453361411468,44.1842637318268));
#40346=CARTESIAN_POINT('Ctrl Pts',(31.1717913010471,34.1193446687329,44.2953935210466));
#40347=CARTESIAN_POINT('Ctrl Pts',(29.770277898053,32.4537519388178,44.4065233102662));
#40348=CARTESIAN_POINT('Ctrl Pts',(30.4093819824319,30.372890355238,44.5176530994861));
#40349=CARTESIAN_POINT('Ctrl Pts',(32.5042024269548,29.7811418732718,44.6287828887057));
#40350=CARTESIAN_POINT('Ctrl Pts',(34.1375822781764,31.2200682863745,44.7399126779255));
#40351=CARTESIAN_POINT('Ctrl Pts',(33.8146700095254,33.3727797457791,44.8510424671451));
#40352=CARTESIAN_POINT('Ctrl Pts',(31.8309914274337,34.2691380690237,44.9621722563649));
#40353=CARTESIAN_POINT('Ctrl Pts',(30.0019876581329,33.0888058392751,45.0733020455846));
#40354=CARTESIAN_POINT('Ctrl Pts',(30.0015431165673,30.9120103130298,45.1844318348044));
#40355=CARTESIAN_POINT('Ctrl Pts',(31.8300646423569,29.7309311495427,45.2955616240241));
#40356=CARTESIAN_POINT('Ctrl Pts',(33.8141091645892,30.6264791909671,45.4066914132438));
#40357=CARTESIAN_POINT('Ctrl Pts',(34.1379006525841,32.7790585816055,45.5178212024635));
#40358=CARTESIAN_POINT('Ctrl Pts',(32.5051086479012,34.2186520068971,45.6289509916833));
#40359=CARTESIAN_POINT('Ctrl Pts',(30.4100466863343,33.6277591757555,45.740080780903));
#40360=CARTESIAN_POINT('Ctrl Pts',(29.7700927551085,31.5471587992758,45.8512105701227));
#40361=CARTESIAN_POINT('Ctrl Pts',(31.1709257520704,29.8809937788405,45.9623403593425));
#40362=CARTESIAN_POINT('Ctrl Pts',(33.3305185098015,30.1541202723448,46.0734701485622));
#40363=CARTESIAN_POINT('Ctrl Pts',(34.2724351562348,32.1165758748671,46.1845999377819));
#40364=CARTESIAN_POINT('Ctrl Pts',(33.134643791215,33.9723425009238,46.2957297270016));
#40365=CARTESIAN_POINT('Ctrl Pts',(30.9584387331748,34.0230426592987,46.4068595162213));
#40366=CARTESIAN_POINT('Ctrl Pts',(29.7354592512714,32.2222761148676,46.5179893054411));
#40367=CARTESIAN_POINT('Ctrl Pts',(30.5849629046826,30.2180848805937,46.6291190946608));
#40368=CARTESIAN_POINT('Ctrl Pts',(32.72949316229,29.8446830395357,46.7402488838805));
#40369=CARTESIAN_POINT('Ctrl Pts',(34.2063991887935,31.4438039072554,46.8513786731003));
#40370=CARTESIAN_POINT('Ctrl Pts',(33.6640326051161,33.5519494073595,46.96250846232));
#40371=CARTESIAN_POINT('Ctrl Pts',(31.5987614269185,34.2397676400387,47.0736382515397));
#40372=CARTESIAN_POINT('Ctrl Pts',(29.9006994395541,32.8777748178231,47.1847680407595));
#40373=CARTESIAN_POINT('Ctrl Pts',(30.1238945591431,30.7124520014073,47.2958978299791));
#40374=CARTESIAN_POINT('Ctrl Pts',(32.0640810326881,29.725479150427,47.4070276191989));
#40375=CARTESIAN_POINT('Ctrl Pts',(33.9456212400468,30.8201231148243,47.5181574084186));
#40376=CARTESIAN_POINT('Ctrl Pts',(34.0465499878984,32.9945776093026,47.6292871976383));
#40377=CARTESIAN_POINT('Ctrl Pts',(32.2744983807359,34.258805461492,47.7404169868581));
#40378=CARTESIAN_POINT('Ctrl Pts',(30.2512288323348,33.4557990510493,47.8515467760777));
#40379=CARTESIAN_POINT('Ctrl Pts',(29.8284156919473,31.3204611365695,47.9626765652976));
#40380=CARTESIAN_POINT('Ctrl Pts',(31.3930129604384,29.8070298206093,48.0738063545172));
#40381=CARTESIAN_POINT('Ctrl Pts',(33.513118185036,30.300581031056,48.184936143737));
#40382=CARTESIAN_POINT('Ctrl Pts',(34.2484340557719,32.3494220524491,48.2960659329567));
#40383=CARTESIAN_POINT('Ctrl Pts',(32.9260074619175,34.0784758007651,48.4071957221765));
#40384=CARTESIAN_POINT('Ctrl Pts',(30.7561088810489,33.9053310363523,48.5183255113961));
#40385=CARTESIAN_POINT('Ctrl Pts',(29.7246059628069,31.9884479699246,48.6294553006159));
#40386=CARTESIAN_POINT('Ctrl Pts',(30.7755189917832,30.0821371961453,48.7405850898356));
#40387=CARTESIAN_POINT('Ctrl Pts',(32.9470637605359,29.9310336620978,48.8517148790554));
#40388=CARTESIAN_POINT('Ctrl Pts',(34.251866046125,31.6734256834927,48.962844668275));
#40389=CARTESIAN_POINT('Ctrl Pts',(33.4957849467709,33.7146949778041,49.0739744574948));
#40390=CARTESIAN_POINT('Ctrl Pts',(31.3707776852443,34.1866940235219,49.1851042467145));
#40391=CARTESIAN_POINT('Ctrl Pts',(29.8216278625503,32.6574544126216,49.2962340359343));
#40392=CARTESIAN_POINT('Ctrl Pts',(30.2661005965881,30.5265196530863,49.4073638251539));
#40393=CARTESIAN_POINT('Ctrl Pts',(32.2974192612725,29.7440981278174,49.5184936143737));
#40394=CARTESIAN_POINT('Ctrl Pts',(34.0565430434178,31.0262535317329,49.6296234035934));
#40395=CARTESIAN_POINT('Ctrl Pts',(33.9335409345078,33.1995711435658,49.7407531928132));
#40396=CARTESIAN_POINT('Ctrl Pts',(32.0409831307145,34.2750542536145,49.8518829820329));
#40397=CARTESIAN_POINT('Ctrl Pts',(30.1109180101348,33.2684323826914,49.9630127712527));
#40398=CARTESIAN_POINT('Ctrl Pts',(29.9097202404387,31.1009549507053,50.0741425604723));
#40399=CARTESIAN_POINT('Ctrl Pts',(31.6215238385528,29.7562737980964,50.1852723496921));
#40400=CARTESIAN_POINT('Ctrl Pts',(33.6797047152209,30.4650265332718,50.2964021389118));
#40401=CARTESIAN_POINT('Ctrl Pts',(34.2006380521566,32.5785703391035,50.4075319281315));
#40402=CARTESIAN_POINT('Ctrl Pts',(32.7075713086873,34.1626128449203,50.5186617173513));
#40403=CARTESIAN_POINT('Ctrl Pts',(30.5669429767931,33.7674555276286,50.6297915065709));
#40404=CARTESIAN_POINT('Ctrl Pts',(29.7378328916927,31.7547420787026,50.7409212957907));
#40405=CARTESIAN_POINT('Ctrl Pts',(30.9790336119123,29.9664860196478,50.8520510850104));
#40406=CARTESIAN_POINT('Ctrl Pts',(33.1546116986341,30.0392799028483,50.9631808742301));
#40407=CARTESIAN_POINT('Ctrl Pts',(34.2735016799217,31.906503555882,51.0743106634499));
#40408=CARTESIAN_POINT('Ctrl Pts',(33.3117075790158,33.8592941405585,51.1854404526696));
#40409=CARTESIAN_POINT('Ctrl Pts',(31.1494529263309,34.1104788911743,51.2965702418893));
#40410=CARTESIAN_POINT('Ctrl Pts',(29.7656097323423,32.4301762474351,51.4077000311091));
#40411=CARTESIAN_POINT('Ctrl Pts',(30.4266562790277,30.3561809677892,51.5188298203287));
#40412=CARTESIAN_POINT('Ctrl Pts',(32.5276099395835,29.7865910386039,51.6299596095486));
#40413=CARTESIAN_POINT('Ctrl Pts',(34.1457006999001,31.2426889901276,51.7410893987682));
#40414=CARTESIAN_POINT('Ctrl Pts',(33.8000694591651,33.3918697599249,51.852219187988));
#40415=CARTESIAN_POINT('Ctrl Pts',(31.807034149869,34.2672264300624,51.9633489772076));
#40416=CARTESIAN_POINT('Ctrl Pts',(29.9905991345169,33.0676420378163,52.0744787664275));
#40417=CARTESIAN_POINT('Ctrl Pts',(30.0131459199694,30.8909632715124,52.1856085556471));
#40418=CARTESIAN_POINT('Ctrl Pts',(31.8540401717833,29.7292628112352,52.2967383448669));
#40419=CARTESIAN_POINT('Ctrl Pts',(33.8285149610311,30.6457165611199,52.4078681340866));
#40420=CARTESIAN_POINT('Ctrl Pts',(34.1295533099436,32.8015955106775,52.5189979233063));
#40421=CARTESIAN_POINT('Ctrl Pts',(32.4816463311111,34.2238635693672,52.630127712526));
#40422=CARTESIAN_POINT('Ctrl Pts',(30.3929442933283,33.6108745637776,52.7412575017457));
#40423=CARTESIAN_POINT('Ctrl Pts',(29.7749973799223,31.5236330861956,52.8523872909655));
#40424=CARTESIAN_POINT('Ctrl Pts',(31.1933582983878,29.8723525729158,52.9635170801853));
#40425=CARTESIAN_POINT('Ctrl Pts',(33.349930022317,30.1682815511726,53.0746468694049));
#40426=CARTESIAN_POINT('Ctrl Pts',(34.2710979093908,32.14056030596,53.1857766586248));
#40427=CARTESIAN_POINT('Ctrl Pts',(33.1137074189905,33.9842375731813,53.2969064478443));
#40428=CARTESIAN_POINT('Ctrl Pts',(30.9372108707685,34.0118873374463,53.4080362370642));
#40429=CARTESIAN_POINT('Ctrl Pts',(29.7330765948496,32.1984277054576,53.5191660262838));
#40430=CARTESIAN_POINT('Ctrl Pts',(30.6041818261707,30.2030759624636,53.6302958155036));
#40431=CARTESIAN_POINT('Ctrl Pts',(32.7515840301711,29.8528310493422,53.7414256047234));
#40432=CARTESIAN_POINT('Ctrl Pts',(34.2134123571603,31.4664895293539,53.852555393943));
#40433=CARTESIAN_POINT('Ctrl Pts',(33.6449478315736,33.5708435359449,53.9636851831628));
#40434=CARTESIAN_POINT('Ctrl Pts',(32.2693872463958,34.0108324267675,54.0377717093093));
#40435=CARTESIAN_POINT('Ctrl Pts',(31.640528121452,33.8913081882596,54.0748149723825));
#40436=CARTESIAN_POINT('Ctrl Pts',(30.4347998857282,33.3312198033321,40.7755550828525));
#40437=CARTESIAN_POINT('Ctrl Pts',(29.9921698977506,32.8107914668331,40.8125983459258));
#40438=CARTESIAN_POINT('Ctrl Pts',(29.6747827202174,31.3023956948159,40.8866848720723));
#40439=CARTESIAN_POINT('Ctrl Pts',(31.3274084520903,29.6648804500478,40.9978146612919));
#40440=CARTESIAN_POINT('Ctrl Pts',(33.595753225024,30.1699942663438,41.1089444505117));
#40441=CARTESIAN_POINT('Ctrl Pts',(34.4035641913493,32.3471922981561,41.2200742397314));
#40442=CARTESIAN_POINT('Ctrl Pts',(33.0117215203461,34.2080087873732,41.3312040289512));
#40443=CARTESIAN_POINT('Ctrl Pts',(30.693930615665,34.0473906585599,41.4423338181709));
#40444=CARTESIAN_POINT('Ctrl Pts',(29.5714562640958,32.0133707418711,41.5534636073906));
#40445=CARTESIAN_POINT('Ctrl Pts',(30.6715507113449,29.9669383183226,41.6645933966104));
#40446=CARTESIAN_POINT('Ctrl Pts',(32.9874316286532,29.7812306730564,41.7757231858301));
#40447=CARTESIAN_POINT('Ctrl Pts',(34.3996237629505,31.6260718118722,41.8868529750498));
#40448=CARTESIAN_POINT('Ctrl Pts',(33.6157072951735,33.8131506243979,41.9979827642696));
#40449=CARTESIAN_POINT('Ctrl Pts',(31.3531125056534,34.3408422066741,42.1091125534892));
#40450=CARTESIAN_POINT('Ctrl Pts',(29.6825424018648,32.7262261662198,42.220242342709));
#40451=CARTESIAN_POINT('Ctrl Pts',(30.1328842256904,30.4469728946945,42.3313721319287));
#40452=CARTESIAN_POINT('Ctrl Pts',(32.2919902260347,29.5890346627002,42.4425019211484));
#40453=CARTESIAN_POINT('Ctrl Pts',(34.1838699037172,30.9375850166979,42.5536317103681));
#40454=CARTESIAN_POINT('Ctrl Pts',(34.0770955459249,33.2584464182579,42.6647614995879));
#40455=CARTESIAN_POINT('Ctrl Pts',(32.0693858609145,34.4275911150555,42.7758912888076));
#40456=CARTESIAN_POINT('Ctrl Pts',(29.9981749928738,33.3750308454857,42.8870210780274));
#40457=CARTESIAN_POINT('Ctrl Pts',(29.7590126602339,31.0640572092229,42.9981508672471));
#40458=CARTESIAN_POINT('Ctrl Pts',(31.5707776395802,29.6096482896975,43.1092806564668));
#40459=CARTESIAN_POINT('Ctrl Pts',(33.7753622678902,30.3428633207829,43.2204104456866));
#40460=CARTESIAN_POINT('Ctrl Pts',(34.3551546019171,32.5926718760388,43.3315402349062));
#40461=CARTESIAN_POINT('Ctrl Pts',(32.7795349847121,34.3000735544458,43.442670024126));
#40462=CARTESIAN_POINT('Ctrl Pts',(30.490493403277,33.9024728606777,43.5537998133457));
#40463=CARTESIAN_POINT('Ctrl Pts',(29.5829358892083,31.763749635471,43.6649296025654));
#40464=CARTESIAN_POINT('Ctrl Pts',(30.887449237386,29.8412401822595,43.7760593917852));
#40465=CARTESIAN_POINT('Ctrl Pts',(33.2101569783881,29.8944043032633,43.8871891810048));
#40466=CARTESIAN_POINT('Ctrl Pts',(34.42534217638,31.8745867717898,43.9983189702247));
#40467=CARTESIAN_POINT('Ctrl Pts',(33.4208805162873,33.9695460666721,44.1094487594443));
#40468=CARTESIAN_POINT('Ctrl Pts',(31.1160444164971,34.2619981602002,44.2205785486641));
#40469=CARTESIAN_POINT('Ctrl Pts',(29.6201948806291,32.4842940678484,44.3317083378838));
#40470=CARTESIAN_POINT('Ctrl Pts',(30.3023171820977,30.2633692965589,44.4428381271035));
#40471=CARTESIAN_POINT('Ctrl Pts',(32.5381403879069,29.6317901120796,44.5539679163233));
#40472=CARTESIAN_POINT('Ctrl Pts',(34.2814633465932,31.16757093486,44.6650977055429));
#40473=CARTESIAN_POINT('Ctrl Pts',(33.9368157919171,33.4651818107383,44.7762274947627));
#40474=CARTESIAN_POINT('Ctrl Pts',(31.8196154283712,34.4218741826645,44.8873572839824));
#40475=CARTESIAN_POINT('Ctrl Pts',(29.8675010685907,33.1620935667478,44.9984870732022));
#40476=CARTESIAN_POINT('Ctrl Pts',(29.8670266048481,30.8387775209235,45.1096168624218));
#40477=CARTESIAN_POINT('Ctrl Pts',(31.8186262612152,29.5781996950166,45.2207466516417));
#40478=CARTESIAN_POINT('Ctrl Pts',(33.9362171964019,30.5340272448998,45.3318764408613));
#40479=CARTESIAN_POINT('Ctrl Pts',(34.2818031508426,32.8314971624382,45.4430062300811));
#40480=CARTESIAN_POINT('Ctrl Pts',(32.539107606757,34.3679898941243,45.5541360193008));
#40481=CARTESIAN_POINT('Ctrl Pts',(30.3030266273459,33.737323954489,45.6652658085205));
#40482=CARTESIAN_POINT('Ctrl Pts',(29.6199972756779,31.516677972199,45.7763955977403));
#40483=CARTESIAN_POINT('Ctrl Pts',(31.1151206072547,29.7383630683434,45.88752538696));
#40484=CARTESIAN_POINT('Ctrl Pts',(33.4200759629546,30.0298737579086,45.9986551761796));
#40485=CARTESIAN_POINT('Ctrl Pts',(34.425393197441,32.1244226191065,46.1097849653995));
#40486=CARTESIAN_POINT('Ctrl Pts',(33.2110168799234,34.1051012486052,46.2209147546191));
#40487=CARTESIAN_POINT('Ctrl Pts',(30.8883310468311,34.1592140442528,46.3320445438389));
#40488=CARTESIAN_POINT('Ctrl Pts',(29.5830325841312,32.2372375623016,46.4431743330585));
#40489=CARTESIAN_POINT('Ctrl Pts',(30.4897164895143,30.0981438360661,46.5543041222784));
#40490=CARTESIAN_POINT('Ctrl Pts',(32.7785954853513,29.6996082462917,46.665433911498));
#40491=CARTESIAN_POINT('Ctrl Pts',(34.3549123365112,31.4063662428014,46.7765637007178));
#40492=CARTESIAN_POINT('Ctrl Pts',(33.776038955257,33.6564114162091,46.8876934899375));
#40493=CARTESIAN_POINT('Ctrl Pts',(31.571753982492,34.3905268245362,46.9988232791573));
#40494=CARTESIAN_POINT('Ctrl Pts',(29.7593951208157,32.9368580072316,47.1099530683769));
#40495=CARTESIAN_POINT('Ctrl Pts',(29.9976135462207,30.6257869015107,47.2210828575967));
#40496=CARTESIAN_POINT('Ctrl Pts',(32.0683943391477,29.5723807208067,47.3322126468164));
#40497=CARTESIAN_POINT('Ctrl Pts',(34.0765813745924,30.7407053779857,47.4433424360362));
#40498=CARTESIAN_POINT('Ctrl Pts',(34.1843036555974,33.0615228167506,47.5544722252558));
#40499=CARTESIAN_POINT('Ctrl Pts',(32.2929749187864,34.410846085361,47.6656020144756));
#40500=CARTESIAN_POINT('Ctrl Pts',(30.1335187134828,33.5537891611861,47.7767318036953));
#40501=CARTESIAN_POINT('Ctrl Pts',(29.682245940453,31.2747212468355,47.8878615929151));
#40502=CARTESIAN_POINT('Ctrl Pts',(31.3521565477245,29.6594205820605,47.9989913821348));
#40503=CARTESIAN_POINT('Ctrl Pts',(33.6149664569488,30.1861928180569,48.1101211713545));
#40504=CARTESIAN_POINT('Ctrl Pts',(34.3997765783555,32.3729417170477,48.2212509605742));
#40505=CARTESIAN_POINT('Ctrl Pts',(32.9883371997446,34.2183784009811,48.3323807497939));
#40506=CARTESIAN_POINT('Ctrl Pts',(30.672382333998,34.0335792296485,48.4435105390137));
#40507=CARTESIAN_POINT('Ctrl Pts',(29.5714487587624,31.98767040059,48.5546403282333));
#40508=CARTESIAN_POINT('Ctrl Pts',(30.6930989429659,29.9530454872026,48.6657701174531));
#40509=CARTESIAN_POINT('Ctrl Pts',(33.0108108018152,29.7917711456301,48.7768999066728));
#40510=CARTESIAN_POINT('Ctrl Pts',(34.40343957663,31.6514439043321,48.8880296958926));
#40511=CARTESIAN_POINT('Ctrl Pts',(33.5964665151298,33.830111421856,48.9991594851123));
#40512=CARTESIAN_POINT('Ctrl Pts',(31.3284246119414,34.3338808128292,49.1102892743321));
#40513=CARTESIAN_POINT('Ctrl Pts',(29.6750012209723,32.7017077937846,49.2214190635517));
#40514=CARTESIAN_POINT('Ctrl Pts',(30.1493914990076,30.4273394115725,49.3325488527715));
#40515=CARTESIAN_POINT('Ctrl Pts',(32.3174386081376,29.5922529450954,49.4436786419912));
#40516=CARTESIAN_POINT('Ctrl Pts',(34.1949693455785,30.9607104723374,49.554808431211));
#40517=CARTESIAN_POINT('Ctrl Pts',(34.0636879413972,33.2803145046706,49.6659382204306));
#40518=CARTESIAN_POINT('Ctrl Pts',(32.0437417130131,34.4281885867619,49.7770680096504));
#40519=CARTESIAN_POINT('Ctrl Pts',(29.9837635432384,33.3538108068575,49.8881977988701));
#40520=CARTESIAN_POINT('Ctrl Pts',(29.7690231135183,31.0404400579838,49.9993275880899));
#40521=CARTESIAN_POINT('Ctrl Pts',(31.5960485363689,29.6052481620493,50.1104573773095));
#40522=CARTESIAN_POINT('Ctrl Pts',(33.7927659580644,30.3617071782046,50.2215871665294));
#40523=CARTESIAN_POINT('Ctrl Pts',(34.348763416675,32.617514018322,50.3327169557489));
#40524=CARTESIAN_POINT('Ctrl Pts',(32.7551980676263,34.3081787255302,50.4438467449689));
#40525=CARTESIAN_POINT('Ctrl Pts',(30.4704836368621,33.8864232942922,50.5549765341884));
#40526=CARTESIAN_POINT('Ctrl Pts',(29.5855659947393,31.7382337215207,50.6661063234083));
#40527=CARTESIAN_POINT('Ctrl Pts',(30.910312170761,29.8296098080883,50.7772361126278));
#40528=CARTESIAN_POINT('Ctrl Pts',(33.2323288309766,29.9073034613682,50.8883659018477));
#40529=CARTESIAN_POINT('Ctrl Pts',(34.4265315090395,31.9002102925021,50.9994956910673));
#40530=CARTESIAN_POINT('Ctrl Pts',(33.3999988648512,33.9844435816704,51.1106254802872));
#40531=CARTESIAN_POINT('Ctrl Pts',(31.0922024415436,34.2525356254733,51.2217552695068));
#40532=CARTESIAN_POINT('Ctrl Pts',(29.6152124997993,32.4591314922087,51.3328850587266));
#40533=CARTESIAN_POINT('Ctrl Pts',(30.3207542148726,30.2455351970729,51.4440148479463));
#40534=CARTESIAN_POINT('Ctrl Pts',(32.5631234646485,29.6376060617633,51.5551446371661));
#40535=CARTESIAN_POINT('Ctrl Pts',(34.2901282208224,31.1917142424714,51.6662744263857));
#40536=CARTESIAN_POINT('Ctrl Pts',(33.9212324757437,33.4855567773556,51.7774042156055));
#40537=CARTESIAN_POINT('Ctrl Pts',(31.7940455819115,34.4198338709223,51.8885340048252));
#40538=CARTESIAN_POINT('Ctrl Pts',(29.8553459812909,33.1395052258002,51.9996637940449));
#40539=CARTESIAN_POINT('Ctrl Pts',(29.879410395147,30.8163137990511,52.1107935832647));
#40540=CARTESIAN_POINT('Ctrl Pts',(31.8442155880729,29.5764190605415,52.2219233724844));
#40541=CARTESIAN_POINT('Ctrl Pts',(33.9515926497335,30.5545594860849,52.3330531617041));
#40542=CARTESIAN_POINT('Ctrl Pts',(34.2728939469864,32.8555510564788,52.4441829509239));
#40543=CARTESIAN_POINT('Ctrl Pts',(32.5140660369754,34.3735522478524,52.5553127401435));
#40544=CARTESIAN_POINT('Ctrl Pts',(30.2847730690242,33.7193028360775,52.6664425293633));
#40545=CARTESIAN_POINT('Ctrl Pts',(29.6252320317178,31.4915687389112,52.7775723185829));
#40546=CARTESIAN_POINT('Ctrl Pts',(31.1390630925179,29.7291402212096,52.8887021078028));
#40547=CARTESIAN_POINT('Ctrl Pts',(33.4407940680577,30.0449882350993,52.9998318970224));
#40548=CARTESIAN_POINT('Ctrl Pts',(34.4239659402583,32.1500214468035,53.1109616862423));
#40549=CARTESIAN_POINT('Ctrl Pts',(33.188671276515,34.1177969804317,53.2220914754619));
#40550=CARTESIAN_POINT('Ctrl Pts',(30.8656743329815,34.1473078555715,53.3332212646817));
#40551=CARTESIAN_POINT('Ctrl Pts',(29.5804895506539,32.2117839119326,53.4443510539014));
#40552=CARTESIAN_POINT('Ctrl Pts',(30.5102290402516,30.0821246648111,53.5554808431211));
#40553=CARTESIAN_POINT('Ctrl Pts',(32.8021732937378,29.7083047001831,53.6666106323408));
#40554=CARTESIAN_POINT('Ctrl Pts',(34.3623975625704,31.4305788384244,53.7777404215606));
#40555=CARTESIAN_POINT('Ctrl Pts',(33.755669581989,33.6765773121718,53.8888702107803));
#40556=CARTESIAN_POINT('Ctrl Pts',(32.2875197530249,34.146181938655,53.9629567369268));
#40557=CARTESIAN_POINT('Ctrl Pts',(31.6163320011532,34.0186125009919,54.));
#40558=CARTESIAN_POINT('Ctrl Pts',(30.7309291201476,33.0793586530485,41.));
#40559=CARTESIAN_POINT('Ctrl Pts',(30.6855978938826,33.0370694300904,41.));
#40560=CARTESIAN_POINT('Ctrl Pts',(30.6429965450219,32.9922112417457,41.));
#40561=CARTESIAN_POINT('Ctrl Pts',(30.6031236806187,32.9451290731506,41.));
#40562=CARTESIAN_POINT('Ctrl Pts',(30.5606226882341,32.8949435919002,41.));
#40563=CARTESIAN_POINT('Ctrl Pts',(30.5212209933767,32.8422310572396,41.));
#40564=CARTESIAN_POINT('Ctrl Pts',(30.4849457305127,32.787354565294,41.));
#40565=CARTESIAN_POINT('Ctrl Pts',(30.4532048755067,32.7393376348417,41.));
#40566=CARTESIAN_POINT('Ctrl Pts',(30.4238579381761,32.6896626994178,41.));
#40567=CARTESIAN_POINT('Ctrl Pts',(30.3969459826243,32.6385454586234,41.));
#40568=CARTESIAN_POINT('Ctrl Pts',(30.3834464248084,32.6129040612093,41.));
#40569=CARTESIAN_POINT('Ctrl Pts',(30.3705599224503,32.5868993924579,41.));
#40570=CARTESIAN_POINT('Ctrl Pts',(30.3582939988302,32.560556837428,41.));
#40571=CARTESIAN_POINT('Ctrl Pts',(30.3526828221897,32.5485061566953,41.));
#40572=CARTESIAN_POINT('Ctrl Pts',(30.3472009327832,32.5363830748729,41.));
#40573=CARTESIAN_POINT('Ctrl Pts',(30.3418575717771,32.5242099978175,41.));
#40574=CARTESIAN_POINT('Ctrl Pts',(30.314936000612,32.4628781207701,41.));
#40575=CARTESIAN_POINT('Ctrl Pts',(30.2914757060973,32.4001707948082,41.));
#40576=CARTESIAN_POINT('Ctrl Pts',(30.2715002890511,32.3364457257782,41.));
#40577=CARTESIAN_POINT('Ctrl Pts',(30.2511708530155,32.2715912743439,41.));
#40578=CARTESIAN_POINT('Ctrl Pts',(30.2344503545547,32.2056818443951,41.));
#40579=CARTESIAN_POINT('Ctrl Pts',(30.2214029865264,32.139057988802,41.));
#40580=CARTESIAN_POINT('Ctrl Pts',(30.2104913962594,32.0833400683238,41.));
#40581=CARTESIAN_POINT('Ctrl Pts',(30.2021493761013,32.0271215322105,41.));
#40582=CARTESIAN_POINT('Ctrl Pts',(30.1964392904162,31.9705892943722,41.));
#40583=CARTESIAN_POINT('Ctrl Pts',(30.1938095119973,31.9445533875158,41.));
#40584=CARTESIAN_POINT('Ctrl Pts',(30.1917383177404,31.918450829594,41.));
#40585=CARTESIAN_POINT('Ctrl Pts',(30.1902336001224,31.8922994784363,41.));
#40586=CARTESIAN_POINT('Ctrl Pts',(30.1895755650056,31.8808631084452,41.));
#40587=CARTESIAN_POINT('Ctrl Pts',(30.1890259817236,31.8694175972641,41.));
#40588=CARTESIAN_POINT('Ctrl Pts',(30.1885858466957,31.8579786000936,41.));
#40589=CARTESIAN_POINT('Ctrl Pts',(30.1858876893862,31.7878541794764,41.));
#40590=CARTESIAN_POINT('Ctrl Pts',(30.1872904995807,31.7178431873908,41.));
#40591=CARTESIAN_POINT('Ctrl Pts',(30.1928490020739,31.6483063267634,41.));
#40592=CARTESIAN_POINT('Ctrl Pts',(30.1978163879672,31.5861643342093,41.));
#40593=CARTESIAN_POINT('Ctrl Pts',(30.206102944145,31.5244000293923,41.));
#40594=CARTESIAN_POINT('Ctrl Pts',(30.2177808112143,31.4632587210937,41.));
#40595=CARTESIAN_POINT('Ctrl Pts',(30.2305088547194,31.3966190490231,41.));
#40596=CARTESIAN_POINT('Ctrl Pts',(30.2472644984874,31.3307186298758,41.));
#40597=CARTESIAN_POINT('Ctrl Pts',(30.2678024552877,31.2657711075514,41.));
#40598=CARTESIAN_POINT('Ctrl Pts',(30.2757346768809,31.2406869112988,41.));
#40599=CARTESIAN_POINT('Ctrl Pts',(30.2842316526018,31.2157449037212,41.));
#40600=CARTESIAN_POINT('Ctrl Pts',(30.2932812639676,31.1909577139282,41.));
#40601=CARTESIAN_POINT('Ctrl Pts',(30.2972497295957,31.180087953147,41.));
#40602=CARTESIAN_POINT('Ctrl Pts',(30.3013243722381,31.1692485178295,41.));
#40603=CARTESIAN_POINT('Ctrl Pts',(30.3054990763298,31.158453031983,41.));
#40604=CARTESIAN_POINT('Ctrl Pts',(30.3307217120053,31.0932291022217,41.));
#40605=CARTESIAN_POINT('Ctrl Pts',(30.3596352637442,31.0294901920278,41.));
#40606=CARTESIAN_POINT('Ctrl Pts',(30.3919270267659,30.9674551823789,41.));
#40607=CARTESIAN_POINT('Ctrl Pts',(30.4249671644409,30.9039824863203,41.));
#40608=CARTESIAN_POINT('Ctrl Pts',(30.4615442128327,30.8422927637179,41.));
#40609=CARTESIAN_POINT('Ctrl Pts',(30.5013793582913,30.7826241753209,41.));
#40610=CARTESIAN_POINT('Ctrl Pts',(30.5318853054709,30.7369296815525,41.));
#40611=CARTESIAN_POINT('Ctrl Pts',(30.5643032022178,30.6924204631662,41.));
#40612=CARTESIAN_POINT('Ctrl Pts',(30.5985274068616,30.6492095916093,41.));
#40613=CARTESIAN_POINT('Ctrl Pts',(30.6198360174704,30.62230571917,41.));
#40614=CARTESIAN_POINT('Ctrl Pts',(30.6418451736476,30.5959052782455,41.));
#40615=CARTESIAN_POINT('Ctrl Pts',(30.6645322910513,30.5700372527086,41.));
#40616=CARTESIAN_POINT('Ctrl Pts',(30.6771876348299,30.555607532519,41.));
#40617=CARTESIAN_POINT('Ctrl Pts',(30.6900583764597,30.5413389753362,41.));
#40618=CARTESIAN_POINT('Ctrl Pts',(30.7031169971451,30.5272619247055,41.));
#40619=CARTESIAN_POINT('Ctrl Pts',(30.7539897854241,30.4724216139574,41.));
#40620=CARTESIAN_POINT('Ctrl Pts',(30.8077591398318,30.4204262274082,41.));
#40621=CARTESIAN_POINT('Ctrl Pts',(30.8641400445596,30.3715397784649,41.));
#40622=CARTESIAN_POINT('Ctrl Pts',(30.9062939887424,30.3349891652741,41.));
#40623=CARTESIAN_POINT('Ctrl Pts',(30.9499089479774,30.3001766489696,41.));
#40624=CARTESIAN_POINT('Ctrl Pts',(30.9948821813454,30.2672223105979,41.));
#40625=CARTESIAN_POINT('Ctrl Pts',(31.0089663888168,30.2569020444318,41.));
#40626=CARTESIAN_POINT('Ctrl Pts',(31.0231839012869,30.2467640954187,41.));
#40627=CARTESIAN_POINT('Ctrl Pts',(31.0375318056939,30.2368123795939,41.));
#40628=CARTESIAN_POINT('Ctrl Pts',(31.0513138251944,30.2272531619083,41.));
#40629=CARTESIAN_POINT('Ctrl Pts',(31.0652090979386,30.2178707336406,41.));
#40630=CARTESIAN_POINT('Ctrl Pts',(31.0792097070466,30.208671281042,41.));
#40631=CARTESIAN_POINT('Ctrl Pts',(31.1421653556993,30.167304687551,41.));
#40632=CARTESIAN_POINT('Ctrl Pts',(31.2072783160395,30.1296140175869,41.));
#40633=CARTESIAN_POINT('Ctrl Pts',(31.2742872364057,30.0958785366594,41.));
#40634=CARTESIAN_POINT('Ctrl Pts',(31.3254776883888,30.0701068258617,41.));
#40635=CARTESIAN_POINT('Ctrl Pts',(31.3777755899145,30.0466437584942,41.));
#40636=CARTESIAN_POINT('Ctrl Pts',(31.4310782545421,30.0256290548068,41.));
#40637=CARTESIAN_POINT('Ctrl Pts',(31.4435633682323,30.0207067687159,41.));
#40638=CARTESIAN_POINT('Ctrl Pts',(31.4561036516355,30.0159188770397,41.));
#40639=CARTESIAN_POINT('Ctrl Pts',(31.4686971487471,30.0112647854283,41.));
#40640=CARTESIAN_POINT('Ctrl Pts',(33.6673070786563,31.998696213291,42.1285196366098));
#40641=CARTESIAN_POINT('Ctrl Pts',(33.6680432869609,31.9130463841536,42.1227790551389));
#40642=CARTESIAN_POINT('Ctrl Pts',(33.6620132262641,31.8275005565021,42.1170384736681));
#40643=CARTESIAN_POINT('Ctrl Pts',(33.6488560817129,31.7430654009713,42.1112978921973));
#40644=CARTESIAN_POINT('Ctrl Pts',(33.563954653281,31.1982157729602,42.074254629124));
#40645=CARTESIAN_POINT('Ctrl Pts',(33.1822841993345,30.6996141041007,42.0372113660508));
#40646=CARTESIAN_POINT('Ctrl Pts',(32.678494630127,30.4754086938519,42.0001681029775));
#40647=CARTESIAN_POINT('Ctrl Pts',(32.1747050609195,30.251203283603,41.9631248399043));
#40648=CARTESIAN_POINT('Ctrl Pts',(31.5487963764509,30.3013941319647,41.9260815768311));
#40649=CARTESIAN_POINT('Ctrl Pts',(31.0871818282615,30.6030322351115,41.8890383137578));
#40650=CARTESIAN_POINT('Ctrl Pts',(30.6255672800722,30.9046703382582,41.8519950506846));
#40651=CARTESIAN_POINT('Ctrl Pts',(30.328246868162,31.4577556961901,41.8149517876113));
#40652=CARTESIAN_POINT('Ctrl Pts',(30.3312711550256,32.0091637019358,41.7779085245381));
#40653=CARTESIAN_POINT('Ctrl Pts',(30.3342954418892,32.5605717076814,41.7408652614648));
#40654=CARTESIAN_POINT('Ctrl Pts',(30.6376644275264,33.1103023612409,41.7038219983916));
#40655=CARTESIAN_POINT('Ctrl Pts',(31.1025613668874,33.4068726645062,41.6667787353184));
#40656=CARTESIAN_POINT('Ctrl Pts',(31.5674583062485,33.7034429677715,41.6297354722451));
#40657=CARTESIAN_POINT('Ctrl Pts',(32.1938831993334,33.7468529207427,41.5926922091719));
#40658=CARTESIAN_POINT('Ctrl Pts',(32.6951809676823,33.5170982491741,41.5556489460986));
#40659=CARTESIAN_POINT('Ctrl Pts',(33.1964787360313,33.2873435776056,41.5186056830254));
#40660=CARTESIAN_POINT('Ctrl Pts',(33.5726493796443,32.7844242814973,41.4815624199522));
#40661=CARTESIAN_POINT('Ctrl Pts',(33.6515719428105,32.2387510696683,41.4445191568789));
#40662=CARTESIAN_POINT('Ctrl Pts',(33.6629345410655,32.1601896895534,41.4391859834559));
#40663=CARTESIAN_POINT('Ctrl Pts',(33.6681358443738,32.080742115373,41.4338528100328));
#40664=CARTESIAN_POINT('Ctrl Pts',(33.6674739163907,32.0012102324881,41.4285196366098));
#40665=CARTESIAN_POINT('Ctrl Pts',(32.5301702171886,30.0148256743283,41.));
#40666=CARTESIAN_POINT('Ctrl Pts',(33.1902397907527,30.1911070339301,41.0370432630732));
#40667=CARTESIAN_POINT('Ctrl Pts',(34.3092433024178,31.2512123085144,41.1111297892197));
#40668=CARTESIAN_POINT('Ctrl Pts',(33.8813840453791,33.5380367222224,41.2222595784394));
#40669=CARTESIAN_POINT('Ctrl Pts',(31.7284038427318,34.4127959913661,41.3333893676592));
#40670=CARTESIAN_POINT('Ctrl Pts',(29.8256278405404,33.0815586024407,41.4445191568789));
#40671=CARTESIAN_POINT('Ctrl Pts',(29.9119860164316,30.7594030366271,41.5556489460986));
#40672=CARTESIAN_POINT('Ctrl Pts',(31.9096898523802,29.5731770382926,41.6667787353184));
#40673=CARTESIAN_POINT('Ctrl Pts',(33.9898334716449,30.6076759933568,41.7779085245381));
#40674=CARTESIAN_POINT('Ctrl Pts',(34.2490097010621,32.9165547497841,41.8890383137578));
#40675=CARTESIAN_POINT('Ctrl Pts',(32.4498627820811,34.3865418359406,42.0001681029776));
#40676=CARTESIAN_POINT('Ctrl Pts',(30.2390335296879,33.6724274291408,42.1112978921972));
#40677=CARTESIAN_POINT('Ctrl Pts',(29.6398079512964,31.4277075354308,42.222427681417));
#40678=CARTESIAN_POINT('Ctrl Pts',(31.2006114825729,29.706752611882,42.3335574706367));
#40679=CARTESIAN_POINT('Ctrl Pts',(33.4930032094031,30.0845482255105,42.4446872598564));
#40680=CARTESIAN_POINT('Ctrl Pts',(34.4190163612264,32.2153468561681,42.5558170490762));
#40681=CARTESIAN_POINT('Ctrl Pts',(33.1311710776567,34.1490612048519,42.6669468382959));
#40682=CARTESIAN_POINT('Ctrl Pts',(30.8080907428172,34.1159786377566,42.7780766275156));
#40683=CARTESIAN_POINT('Ctrl Pts',(29.5758326061327,32.1463750685223,42.8892064167354));
#40684=CARTESIAN_POINT('Ctrl Pts',(30.5621462946373,30.0428107753347,43.0003362059551));
#40685=CARTESIAN_POINT('Ctrl Pts',(32.8643680431626,29.7304447592571,43.1114659951748));
#40686=CARTESIAN_POINT('Ctrl Pts',(34.3755295616921,31.4951511258333,43.2225957843945));
#40687=CARTESIAN_POINT('Ctrl Pts',(33.7126321720426,33.7218896876768,43.3337255736143));
#40688=CARTESIAN_POINT('Ctrl Pts',(31.4823523987704,34.3727734903307,43.444855362834));
#40689=CARTESIAN_POINT('Ctrl Pts',(29.7258180926964,32.8521207213123,43.5559851520537));
#40690=CARTESIAN_POINT('Ctrl Pts',(30.0505904076267,30.5516163115282,43.6671149412734));
#40691=CARTESIAN_POINT('Ctrl Pts',(32.1594412400625,29.576656945096,43.7782447304932));
#40692=CARTESIAN_POINT('Ctrl Pts',(34.1223731791502,30.8195148630926,43.8893745197129));
#40693=CARTESIAN_POINT('Ctrl Pts',(34.1429322006114,33.1427399762344,44.0005043089326));
#40694=CARTESIAN_POINT('Ctrl Pts',(32.2023029113298,34.4201418557892,44.1116340981523));
#40695=CARTESIAN_POINT('Ctrl Pts',(30.0765281914199,33.4826561541886,44.2227638873721));
#40696=CARTESIAN_POINT('Ctrl Pts',(29.7110940115711,31.1882596190528,44.3338936765918));
#40697=CARTESIAN_POINT('Ctrl Pts',(31.4404417701646,29.6367590775809,44.4450234658115));
#40698=CARTESIAN_POINT('Ctrl Pts',(33.6818911525552,30.2480710000371,44.5561532550313));
#40699=CARTESIAN_POINT('Ctrl Pts',(34.3840919914733,32.462729344375,44.667283044251));
#40700=CARTESIAN_POINT('Ctrl Pts',(32.9043976941981,34.2539028108345,44.7784128334707));
#40701=CARTESIAN_POINT('Ctrl Pts',(30.5970084349764,33.9823288673751,44.8895426226904));
#40702=CARTESIAN_POINT('Ctrl Pts',(29.5736218412549,31.8965490419561,45.0006724119102));
#40703=CARTESIAN_POINT('Ctrl Pts',(30.7708302254411,29.9054464114596,45.1118022011299));
#40704=CARTESIAN_POINT('Ctrl Pts',(33.0929614575128,29.8312565107077,45.2229319903496));
#40705=CARTESIAN_POINT('Ctrl Pts',(34.414826216342,31.7418771323123,45.3340617795693));
#40706=CARTESIAN_POINT('Ctrl Pts',(33.526668209675,33.8887290031987,45.4451915687891));
#40707=CARTESIAN_POINT('Ctrl Pts',(31.2413200135407,34.3070365727709,45.5563213580088));
#40708=CARTESIAN_POINT('Ctrl Pts',(29.6503075134721,32.6139692897129,45.6674511472286));
#40709=CARTESIAN_POINT('Ctrl Pts',(30.2097080957199,30.3590039709295,45.7785809364483));
#40710=CARTESIAN_POINT('Ctrl Pts',(32.4075644138576,29.6058604220904,45.889710725668));
#40711=CARTESIAN_POINT('Ctrl Pts',(34.2324222002848,31.0438074515917,46.0008405148877));
#40712=CARTESIAN_POINT('Ctrl Pts',(34.014191398622,33.3568515319198,46.1119703041075));
#40713=CARTESIAN_POINT('Ctrl Pts',(31.9525944719365,34.4281198046771,46.2231000933271));
#40714=CARTESIAN_POINT('Ctrl Pts',(29.9343825704431,33.2771991640567,46.3342298825469));
#40715=CARTESIAN_POINT('Ctrl Pts',(29.806601339792,30.9573996991398,46.4453596717666));
#40716=CARTESIAN_POINT('Ctrl Pts',(31.6861947765452,29.5917767230407,46.5564894609864));
#40717=CARTESIAN_POINT('Ctrl Pts',(33.8529793507283,30.4301335739208,46.6676192502061));
#40718=CARTESIAN_POINT('Ctrl Pts',(34.3239373178492,32.7052151534561,46.7787490394258));
#40719=CARTESIAN_POINT('Ctrl Pts',(32.6680530537252,34.3348914722883,46.8898788286455));
#40720=CARTESIAN_POINT('Ctrl Pts',(30.4007738795658,33.8277004365258,47.0010086178653));
#40721=CARTESIAN_POINT('Ctrl Pts',(29.5970891079424,31.6478177818408,47.112138407085));
#40722=CARTESIAN_POINT('Ctrl Pts',(30.9925223262469,29.790248473958,47.2232681963047));
#40723=CARTESIAN_POINT('Ctrl Pts',(33.3099881859296,29.9550197989514,47.3343979855245));
#40724=CARTESIAN_POINT('Ctrl Pts',(34.42856706408,31.9913348270576,47.4455277747441));
#40725=CARTESIAN_POINT('Ctrl Pts',(33.3245477018974,34.0355801274709,47.556657563964));
#40726=CARTESIAN_POINT('Ctrl Pts',(31.0083166470601,34.21688457017,47.6677873531835));
#40727=CARTESIAN_POINT('Ctrl Pts',(29.5996634424752,32.3693202953617,47.7789171424034));
#40728=CARTESIAN_POINT('Ctrl Pts',(30.387772224771,30.1837580913501,47.890046931623));
#40729=CARTESIAN_POINT('Ctrl Pts',(32.6513743830742,29.6604007858116,48.0011767208428));
#40730=CARTESIAN_POINT('Ctrl Pts',(34.318845769849,31.2782193092014,48.1123065100625));
#40731=CARTESIAN_POINT('Ctrl Pts',(33.8641346548932,33.5566036934244,48.2234362992823));
#40732=CARTESIAN_POINT('Ctrl Pts',(31.7033877194777,34.4104012580895,48.3345660885019));
#40733=CARTESIAN_POINT('Ctrl Pts',(29.81409712657,33.0582257310643,48.4456958777218));
#40734=CARTESIAN_POINT('Ctrl Pts',(29.9253211382958,30.7375734909492,48.5568256669414));
#40735=CARTESIAN_POINT('Ctrl Pts',(31.935268745298,29.572280301472,48.6679554561612));
#40736=CARTESIAN_POINT('Ctrl Pts',(34.0044576946222,30.6288098525638,48.7790852453808));
#40737=CARTESIAN_POINT('Ctrl Pts',(34.2391886992667,32.9402377566512,48.8902150346007));
#40738=CARTESIAN_POINT('Ctrl Pts',(32.4246384893326,34.3911702623054,49.0013448238203));
#40739=CARTESIAN_POINT('Ctrl Pts',(30.221463738974,33.6537296750593,49.1124746130401));
#40740=CARTESIAN_POINT('Ctrl Pts',(29.6459860872837,31.4028136231505,49.2236044022597));
#40741=CARTESIAN_POINT('Ctrl Pts',(31.2248764402936,29.6984360671178,49.3347341914796));
#40742=CARTESIAN_POINT('Ctrl Pts',(33.5131514692818,30.1004248630373,49.4458639806992));
#40743=CARTESIAN_POINT('Ctrl Pts',(34.4166066830276,32.2408842242706,49.556993769919));
#40744=CARTESIAN_POINT('Ctrl Pts',(33.1084096674749,34.160888955732,49.6681235591387));
#40745=CARTESIAN_POINT('Ctrl Pts',(30.7858081444514,34.1032715487725,49.7792533483584));
#40746=CARTESIAN_POINT('Ctrl Pts',(29.5744218402637,32.1207628294065,49.8903831375782));
#40747=CARTESIAN_POINT('Ctrl Pts',(30.5828983635668,30.0277332781861,50.0015129267979));
#40748=CARTESIAN_POINT('Ctrl Pts',(32.8882909367063,29.7397008424277,50.1126427160176));
#40749=CARTESIAN_POINT('Ctrl Pts',(34.3807292776862,31.520269683756,50.2237725052373));
#40750=CARTESIAN_POINT('Ctrl Pts',(33.6943500016618,33.7398825080518,50.3349022944571));
#40751=CARTESIAN_POINT('Ctrl Pts',(31.4573199785767,34.3671737292195,50.4460320836768));
#40752=CARTESIAN_POINT('Ctrl Pts',(29.7169448259793,32.828053224334,50.5571618728965));
#40753=CARTESIAN_POINT('Ctrl Pts',(30.0659970099416,30.5311073884045,50.6682916621163));
#40754=CARTESIAN_POINT('Ctrl Pts',(32.1850277570195,29.5784761411241,50.7794214513359));
#40755=CARTESIAN_POINT('Ctrl Pts',(34.1347231074093,30.8419972691661,50.8905512405558));
#40756=CARTESIAN_POINT('Ctrl Pts',(34.1307430200187,33.1653099384271,51.0016810297753));
#40757=CARTESIAN_POINT('Ctrl Pts',(32.1767300276281,34.4221435893461,51.1128108189952));
#40758=CARTESIAN_POINT('Ctrl Pts',(30.0609756305588,33.4622576942574,51.2239406082148));
#40759=CARTESIAN_POINT('Ctrl Pts',(29.7197953084608,31.1641294150899,51.3350703974346));
#40760=CARTESIAN_POINT('Ctrl Pts',(31.4654335924627,29.6309808302345,51.4462001866543));
#40761=CARTESIAN_POINT('Ctrl Pts',(33.7003012551285,30.2659328993153,51.557329975874));
#40762=CARTESIAN_POINT('Ctrl Pts',(34.3790716488582,32.4878843723627,51.6684597650938));
#40763=CARTESIAN_POINT('Ctrl Pts',(32.8805414680095,34.2633293614917,51.7795895543134));
#40764=CARTESIAN_POINT('Ctrl Pts',(30.5761492876849,33.9673998582603,51.8907193435333));
#40765=CARTESIAN_POINT('Ctrl Pts',(29.5748498323699,31.8709273512164,52.0018491327529));
#40766=CARTESIAN_POINT('Ctrl Pts',(30.7930215224583,29.8925807110175,52.1129789219727));
#40767=CARTESIAN_POINT('Ctrl Pts',(33.1158068029996,29.8429213928206,52.2241087111924));
#40768=CARTESIAN_POINT('Ctrl Pts',(34.4174178435015,31.7673969387678,52.3352385004122));
#40769=CARTESIAN_POINT('Ctrl Pts',(33.5066341990735,33.9047484513664,52.4463682896318));
#40770=CARTESIAN_POINT('Ctrl Pts',(31.216995453309,34.2988945058415,52.5574980788517));
#40771=CARTESIAN_POINT('Ctrl Pts',(29.6439536232049,32.5891178954443,52.6686278680713));
#40772=CARTESIAN_POINT('Ctrl Pts',(30.2271405879685,30.340185676392,52.7797576572911));
#40773=CARTESIAN_POINT('Ctrl Pts',(32.4328278728442,29.6103000988841,52.8908874465108));
#40774=CARTESIAN_POINT('Ctrl Pts',(34.2423985299477,31.0674368629122,53.0020172357305));
#40775=CARTESIAN_POINT('Ctrl Pts',(33.9997449308191,33.3780553787745,53.1131470249502));
#40776=CARTESIAN_POINT('Ctrl Pts',(31.9269572256365,34.4274725972727,53.2242768141699));
#40777=CARTESIAN_POINT('Ctrl Pts',(29.9209961576786,33.2553327321614,53.3354066033897));
#40778=CARTESIAN_POINT('Ctrl Pts',(29.8177590626321,30.9342477419074,53.4465363926093));
#40779=CARTESIAN_POINT('Ctrl Pts',(31.7116016611041,29.5886825160599,53.5576661818292));
#40780=CARTESIAN_POINT('Ctrl Pts',(33.869548688589,30.4496223292041,53.6687959710489));
#40781=CARTESIAN_POINT('Ctrl Pts',(34.3161775882222,32.7300579964386,53.7799257602685));
#40782=CARTESIAN_POINT('Ctrl Pts',(32.6437142303927,34.3411494950526,53.8910555494883));
#40783=CARTESIAN_POINT('Ctrl Pts',(30.3808455967403,33.8120435710866,54.002185338708));
#40784=CARTESIAN_POINT('Ctrl Pts',(29.6023723893559,31.6196455898001,54.1133151279278));
#40785=CARTESIAN_POINT('Ctrl Pts',(30.5427968191103,30.3983372977455,54.1874016540742));
#40786=CARTESIAN_POINT('Ctrl Pts',(31.1673980508611,30.121497522815,54.2244449171475));
#40787=CARTESIAN_POINT('Ctrl Pts',(32.4967348970877,30.1400211999972,40.9251850276175));
#40788=CARTESIAN_POINT('Ctrl Pts',(33.1151770144774,30.3051853306507,40.9622282906908));
#40789=CARTESIAN_POINT('Ctrl Pts',(34.1636102839946,31.2984347954455,41.0363148168372));
#40790=CARTESIAN_POINT('Ctrl Pts',(33.7627340802347,33.4410400436705,41.147444606057));
#40791=CARTESIAN_POINT('Ctrl Pts',(31.7455321237292,34.2606323961771,41.2585743952767));
#40792=CARTESIAN_POINT('Ctrl Pts',(29.9627551758999,33.013349833053,41.3697041844964));
#40793=CARTESIAN_POINT('Ctrl Pts',(30.043667151381,30.8376416008499,41.4808339737161));
#40794=CARTESIAN_POINT('Ctrl Pts',(31.9153852848962,29.7262252479473,41.5919637629359));
#40795=CARTESIAN_POINT('Ctrl Pts',(33.8643441157457,30.6954832622999,41.7030935521556));
#40796=CARTESIAN_POINT('Ctrl Pts',(34.1071753300863,32.85875199049,41.8142233413754));
#40797=CARTESIAN_POINT('Ctrl Pts',(32.4214920708779,34.2360339657663,41.925353130595));
#40798=CARTESIAN_POINT('Ctrl Pts',(30.3500893297177,33.5669553663467,42.0364829198148));
#40799=CARTESIAN_POINT('Ctrl Pts',(29.7886540654114,31.4637993058167,42.1476127090344));
#40800=CARTESIAN_POINT('Ctrl Pts',(31.2510251235106,29.851376843886,42.2587424982543));
#40801=CARTESIAN_POINT('Ctrl Pts',(33.3988465808343,30.2053466806888,42.369872287474));
#40802=CARTESIAN_POINT('Ctrl Pts',(34.2664604768241,32.2017659517052,42.4810020766936));
#40803=CARTESIAN_POINT('Ctrl Pts',(33.0598334848532,34.0135301113067,42.5921318659135));
#40804=CARTESIAN_POINT('Ctrl Pts',(30.8832588044191,33.9825339047513,42.7032616551331));
#40805=CARTESIAN_POINT('Ctrl Pts',(29.7287133417236,32.1371438874559,42.8143914443529));
#40806=CARTESIAN_POINT('Ctrl Pts',(30.652824905654,30.1662414134641,42.9255212335726));
#40807=CARTESIAN_POINT('Ctrl Pts',(32.809856451845,29.8735748399382,43.0366510227923));
#40808=CARTESIAN_POINT('Ctrl Pts',(34.2257161834047,31.526989548972,43.1477808120121));
#40809=CARTESIAN_POINT('Ctrl Pts',(33.604624586873,33.6132982749202,43.2589106012318));
#40810=CARTESIAN_POINT('Ctrl Pts',(31.5149979768988,34.2231339243874,43.3700403904515));
#40811=CARTESIAN_POINT('Ctrl Pts',(29.8692399552855,32.798381510474,43.4811701796712));
#40812=CARTESIAN_POINT('Ctrl Pts',(30.1735304212594,30.642958998618,43.592299968891));
#40813=CARTESIAN_POINT('Ctrl Pts',(32.1493860375522,29.7294856935398,43.7034297581107));
#40814=CARTESIAN_POINT('Ctrl Pts',(33.9885251727594,30.8939624596328,43.8145595473304));
#40815=CARTESIAN_POINT('Ctrl Pts',(34.0077876342834,33.0706727878886,43.9256893365501));
#40816=CARTESIAN_POINT('Ctrl Pts',(32.1895446265783,34.267514991785,44.0368191257699));
#40817=CARTESIAN_POINT('Ctrl Pts',(30.1978324320956,33.3891520652985,44.1479489149896));
#40818=CARTESIAN_POINT('Ctrl Pts',(29.8554444520954,31.2394522334168,44.2590787042094));
#40819=CARTESIAN_POINT('Ctrl Pts',(31.4757304527859,29.7857974696952,44.370208493429));
#40820=CARTESIAN_POINT('Ctrl Pts',(33.5758222576279,30.358556849692,44.4813382826489));
#40821=CARTESIAN_POINT('Ctrl Pts',(34.2337386213657,32.4335472001359,44.5924680718684));
#40822=CARTESIAN_POINT('Ctrl Pts',(32.8473616227183,34.1117598546416,44.7035978610883));
#40823=CARTESIAN_POINT('Ctrl Pts',(30.6854884562122,33.85731279126,44.8147276503079));
#40824=CARTESIAN_POINT('Ctrl Pts',(29.7266419992971,31.9030732030364,44.9258574395277));
#40825=CARTESIAN_POINT('Ctrl Pts',(30.8483481310841,30.0375399682662,45.0369872287474));
#40826=CARTESIAN_POINT('Ctrl Pts',(33.0240335641586,29.9680288725461,45.1481170179672));
#40827=CARTESIAN_POINT('Ctrl Pts',(34.2625345844966,31.7581557168625,45.2592468071868));
#40828=CARTESIAN_POINT('Ctrl Pts',(33.4303884892692,33.7696158264143,45.3703765964066));
#40829=CARTESIAN_POINT('Ctrl Pts',(31.2891663605798,34.1615427223163,45.4815063856263));
#40830=CARTESIAN_POINT('Ctrl Pts',(29.798491470018,32.5752491597092,45.5926361748461));
#40831=CARTESIAN_POINT('Ctrl Pts',(30.3226133117298,30.4624938044536,45.7037659640658));
#40832=CARTESIAN_POINT('Ctrl Pts',(32.3818612600453,29.7568474458017,45.8148957532855));
#40833=CARTESIAN_POINT('Ctrl Pts',(34.0916339242804,31.1041099787756,45.9260255425052));
#40834=CARTESIAN_POINT('Ctrl Pts',(33.8871659038393,33.2712813436514,46.0371553317249));
#40835=CARTESIAN_POINT('Ctrl Pts',(31.9555841136666,34.2749898092894,46.1482851209447));
#40836=CARTESIAN_POINT('Ctrl Pts',(30.064651260996,33.1966522727031,46.2594149101643));
#40837=CARTESIAN_POINT('Ctrl Pts',(29.9449285862787,31.0231515532923,46.3705446993842));
#40838=CARTESIAN_POINT('Ctrl Pts',(31.7059849830777,29.7436519388281,46.4816744886038));
#40839=CARTESIAN_POINT('Ctrl Pts',(33.7361207349039,30.5291376008727,46.5928042778236));
#40840=CARTESIAN_POINT('Ctrl Pts',(34.1773776175914,32.6607405797601,46.7039340670433));
#40841=CARTESIAN_POINT('Ctrl Pts',(32.6259221173363,34.1876409454842,46.815063856263));
#40842=CARTESIAN_POINT('Ctrl Pts',(30.5016294831377,33.7124360418794,46.9261936454828));
#40843=CARTESIAN_POINT('Ctrl Pts',(29.7486292968198,31.6700282433421,47.0373234347025));
#40844=CARTESIAN_POINT('Ctrl Pts',(31.0560591629539,29.9296070181035,47.1484532239222));
#40845=CARTESIAN_POINT('Ctrl Pts',(33.2273734465404,30.0839869974196,47.2595830131419));
#40846=CARTESIAN_POINT('Ctrl Pts',(34.2754088621639,31.9918812984015,47.3707128023616));
#40847=CARTESIAN_POINT('Ctrl Pts',(33.2410147629166,33.9072057470427,47.4818425915815));
#40848=CARTESIAN_POINT('Ctrl Pts',(31.0708574108927,34.0770761787755,47.5929723808011));
#40849=CARTESIAN_POINT('Ctrl Pts',(29.751041280288,32.3460290166462,47.7041021700209));
#40850=CARTESIAN_POINT('Ctrl Pts',(30.489447781022,30.2982998510106,47.8152319592405));
#40851=CARTESIAN_POINT('Ctrl Pts',(32.610295291308,29.8079482075606,47.9263617484603));
#40852=CARTESIAN_POINT('Ctrl Pts',(34.1726071693657,31.3237385927392,48.03749153768));
#40853=CARTESIAN_POINT('Ctrl Pts',(33.7465725269636,33.4584360840934,48.1486213268998));
#40854=CARTESIAN_POINT('Ctrl Pts',(31.7220936486748,34.258388687366,48.2597511161194));
#40855=CARTESIAN_POINT('Ctrl Pts',(29.9519516493499,32.9914884551668,48.3708809053392));
#40856=CARTESIAN_POINT('Ctrl Pts',(30.0561612903804,30.8171887410435,48.482010694559));
#40857=CARTESIAN_POINT('Ctrl Pts',(31.9393510384019,29.7253850640632,48.5931404837786));
#40858=CARTESIAN_POINT('Ctrl Pts',(33.8780460583672,30.7152843092805,48.7042702729984));
#40859=CARTESIAN_POINT('Ctrl Pts',(34.0979736922764,32.8809414224827,48.815400062218));
#40860=CARTESIAN_POINT('Ctrl Pts',(32.3978585545914,34.2403704992407,48.9265298514379));
#40861=CARTESIAN_POINT('Ctrl Pts',(30.3336275823409,33.5494367909,49.0376596406575));
#40862=CARTESIAN_POINT('Ctrl Pts',(29.7944425756754,31.4404753344699,49.1487894298773));
#40863=CARTESIAN_POINT('Ctrl Pts',(31.2737598054777,29.8435847841406,49.259919219097));
#40864=CARTESIAN_POINT('Ctrl Pts',(33.4177241855597,30.2202220540166,49.3710490083167));
#40865=CARTESIAN_POINT('Ctrl Pts',(34.2642027655962,32.2256927991686,49.4821787975365));
#40866=CARTESIAN_POINT('Ctrl Pts',(33.0385075288155,34.0246119420578,49.5933085867562));
#40867=CARTESIAN_POINT('Ctrl Pts',(30.8623814638081,33.9706281915781,49.7044383759759));
#40868=CARTESIAN_POINT('Ctrl Pts',(29.7273915461642,32.1131468907389,49.8155681651957));
#40869=CARTESIAN_POINT('Ctrl Pts',(30.6722682400584,30.1521147825225,49.9266979544154));
#40870=CARTESIAN_POINT('Ctrl Pts',(32.8322706419999,29.8822471858606,50.0378277436351));
#40871=CARTESIAN_POINT('Ctrl Pts',(34.2305879779822,31.5505239986264,50.1489575328548));
#40872=CARTESIAN_POINT('Ctrl Pts',(33.5874953862348,33.6301563734847,50.2600873220746));
#40873=CARTESIAN_POINT('Ctrl Pts',(31.4915442326755,34.2178873136402,50.3712171112943));
#40874=CARTESIAN_POINT('Ctrl Pts',(29.8609262833992,32.7758318363371,50.482346900514));
#40875=CARTESIAN_POINT('Ctrl Pts',(30.1879654022659,30.6237434759671,50.5934766897337));
#40876=CARTESIAN_POINT('Ctrl Pts',(32.173358934285,29.7311901615058,50.7046064789535));
#40877=CARTESIAN_POINT('Ctrl Pts',(34.0000962496398,30.9150270070274,50.8157362681732));
#40878=CARTESIAN_POINT('Ctrl Pts',(33.9963671674767,33.0918193696534,50.9268660573929));
#40879=CARTESIAN_POINT('Ctrl Pts',(32.165584503316,34.269390485504,51.0379958466126));
#40880=CARTESIAN_POINT('Ctrl Pts',(30.1832606974559,33.3700400394506,51.1491256358324));
#40881=CARTESIAN_POINT('Ctrl Pts',(29.8635969994753,31.2168438069273,51.2602554250521));
#40882=CARTESIAN_POINT('Ctrl Pts',(31.4991461594303,29.7803836289929,51.3713852142718));
#40883=CARTESIAN_POINT('Ctrl Pts',(33.5930713223822,30.3752922837321,51.4825150034915));
#40884=CARTESIAN_POINT('Ctrl Pts',(34.2290348879394,32.4571158198614,51.5936447927113));
#40885=CARTESIAN_POINT('Ctrl Pts',(32.8250098955248,34.1205919174751,51.704774581931));
#40886=CARTESIAN_POINT('Ctrl Pts',(30.66594479637,33.8433252839165,51.8159043711507));
#40887=CARTESIAN_POINT('Ctrl Pts',(29.727792546839,31.8790673507646,51.9270341603705));
#40888=CARTESIAN_POINT('Ctrl Pts',(30.8691399282894,30.0254856465071,52.0381639495901));
#40889=CARTESIAN_POINT('Ctrl Pts',(33.0454381620998,29.9789581058905,52.14929373881));
#40890=CARTESIAN_POINT('Ctrl Pts',(34.2649627700276,31.7820661102086,52.2604235280296));
#40891=CARTESIAN_POINT('Ctrl Pts',(33.411617928661,33.7846250039935,52.3715533172494));
#40892=CARTESIAN_POINT('Ctrl Pts',(31.2663758349493,34.1539141369164,52.4826831064691));
#40893=CARTESIAN_POINT('Ctrl Pts',(29.7925382894626,32.5519650249647,52.5938128956888));
#40894=CARTESIAN_POINT('Ctrl Pts',(30.3389464194041,30.4448622904655,52.7049426849086));
#40895=CARTESIAN_POINT('Ctrl Pts',(32.4055314725411,29.7610071332449,52.8160724741282));
#40896=CARTESIAN_POINT('Ctrl Pts',(34.100981094166,31.1262491952386,52.9272022633481));
#40897=CARTESIAN_POINT('Ctrl Pts',(33.8736305062165,33.2911479644908,53.0383320525677));
#40898=CARTESIAN_POINT('Ctrl Pts',(31.9315636868498,34.2743834181852,53.1494618417875));
#40899=CARTESIAN_POINT('Ctrl Pts',(30.0521090657699,33.1761648529178,53.2605916310072));
#40900=CARTESIAN_POINT('Ctrl Pts',(29.9553826444794,31.0014596801536,53.3717214202268));
#40901=CARTESIAN_POINT('Ctrl Pts',(31.7297895759754,29.7407528688005,53.4828512094467));
#40902=CARTESIAN_POINT('Ctrl Pts',(33.7516451232423,30.5473972928286,53.5939809986663));
#40903=CARTESIAN_POINT('Ctrl Pts',(34.1701072572945,32.6840167025074,53.7051107878861));
#40904=CARTESIAN_POINT('Ctrl Pts',(32.6031182281109,34.1935043044452,53.8162405771058));
#40905=CARTESIAN_POINT('Ctrl Pts',(30.4829579825565,33.6977665806563,53.9273703663255));
#40906=CARTESIAN_POINT('Ctrl Pts',(29.7535793867421,31.6436327377849,54.0385001555453));
#40907=CARTESIAN_POINT('Ctrl Pts',(30.6346957097411,30.4993465649721,54.1125866816917));
#40908=CARTESIAN_POINT('Ctrl Pts',(31.2199063053491,30.2399657611256,54.149629944765));
#40909=CARTESIAN_POINT('Ctrl Pts',(32.4632995769868,30.2652167256662,40.850370055235));
#40910=CARTESIAN_POINT('Ctrl Pts',(33.0401142382021,30.4192636273712,40.8874133183083));
#40911=CARTESIAN_POINT('Ctrl Pts',(34.0179772655714,31.3456572823766,40.9614998444547));
#40912=CARTESIAN_POINT('Ctrl Pts',(33.6440841150904,33.3440433651185,41.0726296336745));
#40913=CARTESIAN_POINT('Ctrl Pts',(31.7626604047266,34.1084688009882,41.1837594228942));
#40914=CARTESIAN_POINT('Ctrl Pts',(30.0998825112594,32.9451410636651,41.294889212114));
#40915=CARTESIAN_POINT('Ctrl Pts',(30.1753482863305,30.9158801650729,41.4060190013336));
#40916=CARTESIAN_POINT('Ctrl Pts',(31.9210807174123,29.8792734576019,41.5171487905534));
#40917=CARTESIAN_POINT('Ctrl Pts',(33.7388547598464,30.7832905312431,41.6282785797731));
#40918=CARTESIAN_POINT('Ctrl Pts',(33.9653409591104,32.8009492311959,41.7394083689928));
#40919=CARTESIAN_POINT('Ctrl Pts',(32.3931213596747,34.085526095592,41.8505381582126));
#40920=CARTESIAN_POINT('Ctrl Pts',(30.4611451297475,33.4614833035526,41.9616679474322));
#40921=CARTESIAN_POINT('Ctrl Pts',(29.9375001795264,31.4998910762026,42.0727977366521));
#40922=CARTESIAN_POINT('Ctrl Pts',(31.3014387644482,29.9960010758901,42.1839275258717));
#40923=CARTESIAN_POINT('Ctrl Pts',(33.3046899522655,30.326145135867,42.2950573150915));
#40924=CARTESIAN_POINT('Ctrl Pts',(34.1139045924217,32.1881850472423,42.4061871043112));
#40925=CARTESIAN_POINT('Ctrl Pts',(32.9884958920498,33.8779990177615,42.5173168935309));
#40926=CARTESIAN_POINT('Ctrl Pts',(30.958426866021,33.849089171746,42.6284466827506));
#40927=CARTESIAN_POINT('Ctrl Pts',(29.8815940773145,32.1279127063896,42.7395764719704));
#40928=CARTESIAN_POINT('Ctrl Pts',(30.7435035166707,30.2896720515934,42.8507062611901));
#40929=CARTESIAN_POINT('Ctrl Pts',(32.7553448605274,30.0167049206194,42.9618360504098));
#40930=CARTESIAN_POINT('Ctrl Pts',(34.0759028051174,31.5588279721106,43.0729658396296));
#40931=CARTESIAN_POINT('Ctrl Pts',(33.4966170017034,33.5047068621638,43.1840956288492));
#40932=CARTESIAN_POINT('Ctrl Pts',(31.5476435550272,34.0734943584441,43.2952254180691));
#40933=CARTESIAN_POINT('Ctrl Pts',(30.0126618178744,32.7446422996357,43.4063552072887));
#40934=CARTESIAN_POINT('Ctrl Pts',(30.296470434892,30.7343016857078,43.5174849965085));
#40935=CARTESIAN_POINT('Ctrl Pts',(32.1393308350419,29.8823144419834,43.6286147857282));
#40936=CARTESIAN_POINT('Ctrl Pts',(33.8546771663686,30.968410056173,43.739744574948));
#40937=CARTESIAN_POINT('Ctrl Pts',(33.8726430679553,32.9986055995426,43.8508743641676));
#40938=CARTESIAN_POINT('Ctrl Pts',(32.1767863418268,34.1148881277808,43.9620041533874));
#40939=CARTESIAN_POINT('Ctrl Pts',(30.3191366727714,33.2956479764084,44.0731339426071));
#40940=CARTESIAN_POINT('Ctrl Pts',(29.9997948926197,31.2906448477808,44.1842637318268));
#40941=CARTESIAN_POINT('Ctrl Pts',(31.5110191354072,29.9348358618094,44.2953935210465));
#40942=CARTESIAN_POINT('Ctrl Pts',(33.4697533627006,30.469042699347,44.4065233102663));
#40943=CARTESIAN_POINT('Ctrl Pts',(34.0833852512582,32.4043650558968,44.517653099486));
#40944=CARTESIAN_POINT('Ctrl Pts',(32.7903255512385,33.9696168984488,44.6287828887058));
#40945=CARTESIAN_POINT('Ctrl Pts',(30.773968477448,33.732296715145,44.7399126779254));
#40946=CARTESIAN_POINT('Ctrl Pts',(29.8796621573394,31.9095973641168,44.8510424671452));
#40947=CARTESIAN_POINT('Ctrl Pts',(30.9258660367271,30.1696335250728,44.9621722563649));
#40948=CARTESIAN_POINT('Ctrl Pts',(32.9551056708045,30.1048012343845,45.0733020455847));
#40949=CARTESIAN_POINT('Ctrl Pts',(34.1102429526512,31.7744343014126,45.1844318348043));
#40950=CARTESIAN_POINT('Ctrl Pts',(33.3341087688635,33.6505026496298,45.2955616240241));
#40951=CARTESIAN_POINT('Ctrl Pts',(31.337012707619,34.0160488718617,45.4066914132438));
#40952=CARTESIAN_POINT('Ctrl Pts',(29.9466754265638,32.5365290297053,45.5178212024635));
#40953=CARTESIAN_POINT('Ctrl Pts',(30.4355185277397,30.5659836379777,45.6289509916833));
#40954=CARTESIAN_POINT('Ctrl Pts',(32.3561581062331,29.907834469513,45.7400807809029));
#40955=CARTESIAN_POINT('Ctrl Pts',(33.9508456482759,31.1644125059596,45.8512105701228));
#40956=CARTESIAN_POINT('Ctrl Pts',(33.7601404090566,33.1857111553829,45.9623403593423));
#40957=CARTESIAN_POINT('Ctrl Pts',(31.9585737553967,34.1218598139018,46.0734701485622));
#40958=CARTESIAN_POINT('Ctrl Pts',(30.1949199515488,33.1161053813493,46.1845999377819));
#40959=CARTESIAN_POINT('Ctrl Pts',(30.0832558327655,31.0889034074447,46.2957297270016));
#40960=CARTESIAN_POINT('Ctrl Pts',(31.7257751896102,29.8955271546156,46.4068595162213));
#40961=CARTESIAN_POINT('Ctrl Pts',(33.6192621190795,30.6281416278246,46.5179893054411));
#40962=CARTESIAN_POINT('Ctrl Pts',(34.0308179173337,32.616266006064,46.6291190946608));
#40963=CARTESIAN_POINT('Ctrl Pts',(32.5837911809473,34.0403904186801,46.7402488838805));
#40964=CARTESIAN_POINT('Ctrl Pts',(30.6024850867097,33.5971716472329,46.8513786731003));
#40965=CARTESIAN_POINT('Ctrl Pts',(29.9001694856972,31.6922387048434,46.96250846232));
#40966=CARTESIAN_POINT('Ctrl Pts',(31.119595999661,30.068965562249,47.0736382515397));
#40967=CARTESIAN_POINT('Ctrl Pts',(33.1447587071512,30.2129541958878,47.1847680407594));
#40968=CARTESIAN_POINT('Ctrl Pts',(34.1222506602479,31.9924277697453,47.2958978299792));
#40969=CARTESIAN_POINT('Ctrl Pts',(33.1574818239358,33.7788313666146,47.4070276191989));
#40970=CARTESIAN_POINT('Ctrl Pts',(31.1333981747253,33.937267787381,47.5181574084186));
#40971=CARTESIAN_POINT('Ctrl Pts',(29.9024191181009,32.3227377379307,47.6292871976384));
#40972=CARTESIAN_POINT('Ctrl Pts',(30.591123337273,30.4128416106712,47.740416986858));
#40973=CARTESIAN_POINT('Ctrl Pts',(32.5692161995418,29.9554956293095,47.8515467760779));
#40974=CARTESIAN_POINT('Ctrl Pts',(34.0263685688824,31.369257876277,47.9626765652974));
#40975=CARTESIAN_POINT('Ctrl Pts',(33.6290103990342,33.3602684747623,48.0738063545174));
#40976=CARTESIAN_POINT('Ctrl Pts',(31.7407995778718,34.1063761166425,48.1849361437369));
#40977=CARTESIAN_POINT('Ctrl Pts',(30.0898061721298,32.9247511792693,48.2960659329568));
#40978=CARTESIAN_POINT('Ctrl Pts',(30.187001442465,30.8968039911378,48.4071957221765));
#40979=CARTESIAN_POINT('Ctrl Pts',(31.9434333315057,29.8784898266544,48.5183255113961));
#40980=CARTESIAN_POINT('Ctrl Pts',(33.7516344221123,30.8017587659972,48.6294553006159));
#40981=CARTESIAN_POINT('Ctrl Pts',(33.9567586852861,32.8216450883142,48.7405850898356));
#40982=CARTESIAN_POINT('Ctrl Pts',(32.3710786198504,34.0895707361761,48.8517148790554));
#40983=CARTESIAN_POINT('Ctrl Pts',(30.4457914257076,33.4451439067406,48.9628446682751));
#40984=CARTESIAN_POINT('Ctrl Pts',(29.9428990640671,31.4781370457892,49.0739744574948));
#40985=CARTESIAN_POINT('Ctrl Pts',(31.3226431706617,29.9887335011634,49.1851042467146));
#40986=CARTESIAN_POINT('Ctrl Pts',(33.3222969018377,30.340019244996,49.2962340359342));
#40987=CARTESIAN_POINT('Ctrl Pts',(34.1117988481647,32.2105013740665,49.407363825154));
#40988=CARTESIAN_POINT('Ctrl Pts',(32.9686053901562,33.8883349283837,49.5184936143737));
#40989=CARTESIAN_POINT('Ctrl Pts',(30.9389547831648,33.8379848343838,49.6296234035935));
#40990=CARTESIAN_POINT('Ctrl Pts',(29.8803612520648,32.1055309520713,49.7407531928131));
#40991=CARTESIAN_POINT('Ctrl Pts',(30.76163811655,30.2764962868588,49.851882982033));
#40992=CARTESIAN_POINT('Ctrl Pts',(32.7762503472934,30.0247935292935,49.9630127712526));
#40993=CARTESIAN_POINT('Ctrl Pts',(34.0804466782781,31.5807783134968,50.0741425604724));
#40994=CARTESIAN_POINT('Ctrl Pts',(33.4806407708078,33.5204302389176,50.1852723496921));
#40995=CARTESIAN_POINT('Ctrl Pts',(31.5257684867742,34.068600898061,50.2964021389118));
#40996=CARTESIAN_POINT('Ctrl Pts',(30.0049077408191,32.7236104483403,50.4075319281315));
#40997=CARTESIAN_POINT('Ctrl Pts',(30.3099337945902,30.7163795635297,50.5186617173512));
#40998=CARTESIAN_POINT('Ctrl Pts',(32.1616901115504,29.8839041818875,50.629791506571));
#40999=CARTESIAN_POINT('Ctrl Pts',(33.8654693918704,30.9880567448887,50.7409212957908));
#41000=CARTESIAN_POINT('Ctrl Pts',(33.8619913149347,33.0183288008796,50.8520510850104));
#41001=CARTESIAN_POINT('Ctrl Pts',(32.154438979004,34.116637381662,50.9631808742302));
#41002=CARTESIAN_POINT('Ctrl Pts',(30.305545764353,33.2778223846438,51.0743106634499));
#41003=CARTESIAN_POINT('Ctrl Pts',(30.0073986904897,31.2695581987648,51.1854404526696));
#41004=CARTESIAN_POINT('Ctrl Pts',(31.5328587263979,29.9297864277512,51.2965702418893));
#41005=CARTESIAN_POINT('Ctrl Pts',(33.4858413896359,30.4846516681489,51.407700031109));
#41006=CARTESIAN_POINT('Ctrl Pts',(34.0789981270206,32.4263472673601,51.5188298203288));
#41007=CARTESIAN_POINT('Ctrl Pts',(32.7694783230401,33.9778544734584,51.6299596095485));
#41008=CARTESIAN_POINT('Ctrl Pts',(30.7557403050552,33.7192507095727,51.7410893987683));
#41009=CARTESIAN_POINT('Ctrl Pts',(29.8807352613081,31.8872073503127,51.8522191879879));
#41010=CARTESIAN_POINT('Ctrl Pts',(30.9452583341205,30.1583905819967,51.9633489772077));
#41011=CARTESIAN_POINT('Ctrl Pts',(32.9750695212001,30.1149948189604,52.0744787664274));
#41012=CARTESIAN_POINT('Ctrl Pts',(34.1125076965538,31.7967352816494,52.1856085556472));
#41013=CARTESIAN_POINT('Ctrl Pts',(33.3166016582486,33.6645015566205,52.2967383448668));
#41014=CARTESIAN_POINT('Ctrl Pts',(31.3157562165896,34.0089337679915,52.4078681340867));
#41015=CARTESIAN_POINT('Ctrl Pts',(29.9411229557203,32.5148121544851,52.5189979233063));
#41016=CARTESIAN_POINT('Ctrl Pts',(30.4507522508398,30.549538904539,52.6301277125261));
#41017=CARTESIAN_POINT('Ctrl Pts',(32.378235072238,29.9117141676057,52.7412575017457));
#41018=CARTESIAN_POINT('Ctrl Pts',(33.9595636583843,31.185061527565,52.8523872909655));
#41019=CARTESIAN_POINT('Ctrl Pts',(33.7475160816141,33.204240550207,52.9635170801852));
#41020=CARTESIAN_POINT('Ctrl Pts',(31.936170148063,34.1212942390978,53.074646869405));
#41021=CARTESIAN_POINT('Ctrl Pts',(30.1832219738614,33.0969969736741,53.1857766586247));
#41022=CARTESIAN_POINT('Ctrl Pts',(30.0930062263266,31.0686716183996,53.2969064478444));
#41023=CARTESIAN_POINT('Ctrl Pts',(31.7479774908468,29.8928232215412,53.4080362370642));
#41024=CARTESIAN_POINT('Ctrl Pts',(33.6337415578955,30.645172256453,53.5191660262839));
#41025=CARTESIAN_POINT('Ctrl Pts',(34.0240369263667,32.6379754085762,53.6302958155036));
#41026=CARTESIAN_POINT('Ctrl Pts',(32.5625222258292,34.0458591138378,53.7414256047233));
#41027=CARTESIAN_POINT('Ctrl Pts',(30.5850703683726,33.583489590226,53.8525553939431));
#41028=CARTESIAN_POINT('Ctrl Pts',(29.9047863841283,31.6676198857696,53.9636851831627));
#41029=CARTESIAN_POINT('Ctrl Pts',(30.7265946003719,30.6003558321987,54.0377717093093));
#41030=CARTESIAN_POINT('Ctrl Pts',(31.2724145598371,30.3584339994361,54.0748149723825));
#41031=CARTESIAN_POINT('Ctrl Pts',(32.4298642568859,30.3904122513352,40.7755550828525));
#41032=CARTESIAN_POINT('Ctrl Pts',(32.9650514619268,30.5333419240918,40.8125983459258));
#41033=CARTESIAN_POINT('Ctrl Pts',(33.8723442471483,31.3928797693077,40.8866848720722));
#41034=CARTESIAN_POINT('Ctrl Pts',(33.525434149946,33.2470466865665,40.997814661292));
#41035=CARTESIAN_POINT('Ctrl Pts',(31.7797886857239,33.9563052057992,41.1089444505117));
#41036=CARTESIAN_POINT('Ctrl Pts',(30.2370098466189,32.8769322942773,41.2200742397314));
#41037=CARTESIAN_POINT('Ctrl Pts',(30.3070294212799,30.9941187292959,41.3312040289512));
#41038=CARTESIAN_POINT('Ctrl Pts',(31.9267761499284,30.0323216672566,41.4423338181709));
#41039=CARTESIAN_POINT('Ctrl Pts',(33.6133654039472,30.8710978001861,41.5534636073906));
#41040=CARTESIAN_POINT('Ctrl Pts',(33.8235065881346,32.7431464719018,41.6645933966104));
#41041=CARTESIAN_POINT('Ctrl Pts',(32.3647506484716,33.9350182254177,41.7757231858301));
#41042=CARTESIAN_POINT('Ctrl Pts',(30.5722009297773,33.3560112407585,41.8868529750498));
#41043=CARTESIAN_POINT('Ctrl Pts',(30.0863462936415,31.5359828465885,41.9979827642696));
#41044=CARTESIAN_POINT('Ctrl Pts',(31.3518524053858,30.1406253078941,42.1091125534893));
#41045=CARTESIAN_POINT('Ctrl Pts',(33.2105333236966,30.4469435910453,42.220242342709));
#41046=CARTESIAN_POINT('Ctrl Pts',(33.9613487080195,32.1746041427795,42.3313721319287));
#41047=CARTESIAN_POINT('Ctrl Pts',(32.9171582992462,33.7424679242163,42.4425019211484));
#41048=CARTESIAN_POINT('Ctrl Pts',(31.033594927623,33.7156444387407,42.5536317103682));
#41049=CARTESIAN_POINT('Ctrl Pts',(30.0344748129053,32.1186815253233,42.6647614995878));
#41050=CARTESIAN_POINT('Ctrl Pts',(30.8341821276874,30.4131026897227,42.7758912888076));
#41051=CARTESIAN_POINT('Ctrl Pts',(32.7008332692098,30.1598350013005,42.8870210780273));
#41052=CARTESIAN_POINT('Ctrl Pts',(33.9260894268301,31.5906663952492,42.9981508672471));
#41053=CARTESIAN_POINT('Ctrl Pts',(33.3886094165338,33.3961154494072,43.1092806564668));
#41054=CARTESIAN_POINT('Ctrl Pts',(31.5802891331557,33.9238547925008,43.2204104456866));
#41055=CARTESIAN_POINT('Ctrl Pts',(30.1560836804634,32.6909030887974,43.3315402349062));
#41056=CARTESIAN_POINT('Ctrl Pts',(30.4194104485247,30.8256443727976,43.442670024126));
#41057=CARTESIAN_POINT('Ctrl Pts',(32.1292756325315,30.0351431904271,43.5537998133457));
#41058=CARTESIAN_POINT('Ctrl Pts',(33.7208291599778,31.0428576527132,43.6649296025654));
#41059=CARTESIAN_POINT('Ctrl Pts',(33.7374985016273,32.9265384111968,43.7760593917852));
#41060=CARTESIAN_POINT('Ctrl Pts',(32.1640280570753,33.9622612637765,43.8871891810049));
#41061=CARTESIAN_POINT('Ctrl Pts',(30.4404409134472,33.2021438875183,43.9983189702246));
#41062=CARTESIAN_POINT('Ctrl Pts',(30.1441453331439,31.3418374621448,44.1094487594444));
#41063=CARTESIAN_POINT('Ctrl Pts',(31.5463078180286,30.0838742539237,44.220578548664));
#41064=CARTESIAN_POINT('Ctrl Pts',(33.3636844677732,30.579528549002,44.3317083378838));
#41065=CARTESIAN_POINT('Ctrl Pts',(33.9330318811508,32.3751829116577,44.4428381271035));
#41066=CARTESIAN_POINT('Ctrl Pts',(32.7332894797586,33.8274739422559,44.5539679163233));
#41067=CARTESIAN_POINT('Ctrl Pts',(30.8624484986839,33.6072806390299,44.665097705543));
#41068=CARTESIAN_POINT('Ctrl Pts',(30.0326823153817,31.9161215251971,44.7762274947627));
#41069=CARTESIAN_POINT('Ctrl Pts',(31.0033839423701,30.3017270818794,44.8873572839824));
#41070=CARTESIAN_POINT('Ctrl Pts',(32.8861777774504,30.2415735962229,44.9984870732022));
#41071=CARTESIAN_POINT('Ctrl Pts',(33.9579513208059,31.7907128859628,45.1096168624218));
#41072=CARTESIAN_POINT('Ctrl Pts',(33.2378290484577,33.5313894728454,45.2207466516416));
#41073=CARTESIAN_POINT('Ctrl Pts',(31.3848590546582,33.8705550214071,45.3318764408613));
#41074=CARTESIAN_POINT('Ctrl Pts',(30.0948593831097,32.4978088997016,45.4430062300811));
#41075=CARTESIAN_POINT('Ctrl Pts',(30.5484237437495,30.6694734715018,45.5541360193008));
#41076=CARTESIAN_POINT('Ctrl Pts',(32.3304549524208,30.0588214932243,45.6652658085205));
#41077=CARTESIAN_POINT('Ctrl Pts',(33.8100573722714,31.2247150331435,45.7763955977402));
#41078=CARTESIAN_POINT('Ctrl Pts',(33.6331149142739,33.1001409671145,45.88752538696));
#41079=CARTESIAN_POINT('Ctrl Pts',(31.9615633971268,33.9687298185142,45.9986551761796));
#41080=CARTESIAN_POINT('Ctrl Pts',(30.3251886421016,33.0355584899957,46.1097849653995));
#41081=CARTESIAN_POINT('Ctrl Pts',(30.2215830792522,31.1546552615972,46.2209147546191));
#41082=CARTESIAN_POINT('Ctrl Pts',(31.7455653961428,30.0474023704031,46.3320445438389));
#41083=CARTESIAN_POINT('Ctrl Pts',(33.5024035032551,30.7271456547765,46.4431743330586));
#41084=CARTESIAN_POINT('Ctrl Pts',(33.884258217076,32.5717914323679,46.5543041222783));
#41085=CARTESIAN_POINT('Ctrl Pts',(32.5416602445583,33.893139891876,46.665433911498));
#41086=CARTESIAN_POINT('Ctrl Pts',(30.7033406902817,33.4819072525865,46.7765637007178));
#41087=CARTESIAN_POINT('Ctrl Pts',(30.0517096745746,31.7144491663447,46.8876934899375));
#41088=CARTESIAN_POINT('Ctrl Pts',(31.183132836368,30.2083241063945,46.9988232791572));
#41089=CARTESIAN_POINT('Ctrl Pts',(33.0621439677619,30.341921394356,47.109953068377));
#41090=CARTESIAN_POINT('Ctrl Pts',(33.9690924583318,31.9929742410892,47.2210828575967));
#41091=CARTESIAN_POINT('Ctrl Pts',(33.073948884955,33.6504569861864,47.3322126468164));
#41092=CARTESIAN_POINT('Ctrl Pts',(31.195938938558,33.7974593959865,47.4433424360361));
#41093=CARTESIAN_POINT('Ctrl Pts',(30.0537969559137,32.2994464592152,47.5544722252559));
#41094=CARTESIAN_POINT('Ctrl Pts',(30.6927988935239,30.5273833703318,47.6656020144756));
#41095=CARTESIAN_POINT('Ctrl Pts',(32.5281371077755,30.1030430510584,47.7767318036953));
#41096=CARTESIAN_POINT('Ctrl Pts',(33.8801299683993,31.4147771598148,47.887861592915));
#41097=CARTESIAN_POINT('Ctrl Pts',(33.5114482711046,33.2621008654313,47.9989913821348));
#41098=CARTESIAN_POINT('Ctrl Pts',(31.7595055070689,33.954363545919,48.1101211713544));
#41099=CARTESIAN_POINT('Ctrl Pts',(30.2276606949097,32.8580139033718,48.2212509605743));
#41100=CARTESIAN_POINT('Ctrl Pts',(30.3178415945496,30.976419241232,48.3323807497939));
#41101=CARTESIAN_POINT('Ctrl Pts',(31.9475156246096,30.0315945892456,48.4435105390137));
#41102=CARTESIAN_POINT('Ctrl Pts',(33.6252227858574,30.8882332227139,48.5546403282333));
#41103=CARTESIAN_POINT('Ctrl Pts',(33.8155436782958,32.7623487541457,48.6657701174532));
#41104=CARTESIAN_POINT('Ctrl Pts',(32.3442986851092,33.9387709731115,48.7768999066728));
#41105=CARTESIAN_POINT('Ctrl Pts',(30.5579552690744,33.3408510225813,48.8880296958926));
#41106=CARTESIAN_POINT('Ctrl Pts',(30.0913555524588,31.5157987571086,48.9991594851122));
#41107=CARTESIAN_POINT('Ctrl Pts',(31.3715265358458,30.1338822181863,49.1102892743321));
#41108=CARTESIAN_POINT('Ctrl Pts',(33.2268696181157,30.4598164359753,49.2214190635517));
#41109=CARTESIAN_POINT('Ctrl Pts',(33.9593949307332,32.1953099489645,49.3325488527716));
#41110=CARTESIAN_POINT('Ctrl Pts',(32.8987032514968,33.7520579147096,49.4436786419912));
#41111=CARTESIAN_POINT('Ctrl Pts',(31.0155281025215,33.7053414771894,49.554808431211));
#41112=CARTESIAN_POINT('Ctrl Pts',(30.0333309579654,32.0979150134037,49.6659382204306));
#41113=CARTESIAN_POINT('Ctrl Pts',(30.8510079930416,30.4008777911951,49.7770680096504));
#41114=CARTESIAN_POINT('Ctrl Pts',(32.7202300525869,30.1673398727264,49.8881977988701));
#41115=CARTESIAN_POINT('Ctrl Pts',(33.9303053785741,31.6110326283673,49.9993275880898));
#41116=CARTESIAN_POINT('Ctrl Pts',(33.3737861553808,33.4107041043505,50.1104573773096));
#41117=CARTESIAN_POINT('Ctrl Pts',(31.559992740873,33.9193144824819,50.2215871665293));
#41118=CARTESIAN_POINT('Ctrl Pts',(30.148889198239,32.6713890603434,50.332716955749));
#41119=CARTESIAN_POINT('Ctrl Pts',(30.4319021869145,30.8090156510923,50.4438467449687));
#41120=CARTESIAN_POINT('Ctrl Pts',(32.1500212888159,30.0366182022692,50.5549765341885));
#41121=CARTESIAN_POINT('Ctrl Pts',(33.7308425341009,31.06108648275,50.6661063234082));
#41122=CARTESIAN_POINT('Ctrl Pts',(33.7276154623926,32.9448382321059,50.7772361126279));
#41123=CARTESIAN_POINT('Ctrl Pts',(32.143293454692,33.96388427782,50.8883659018477));
#41124=CARTESIAN_POINT('Ctrl Pts',(30.42783083125,33.1856047298371,50.9994956910674));
#41125=CARTESIAN_POINT('Ctrl Pts',(30.1512003815042,31.3222725906022,51.1106254802871));
#41126=CARTESIAN_POINT('Ctrl Pts',(31.5665712933655,30.0791892265096,51.2217552695068));
#41127=CARTESIAN_POINT('Ctrl Pts',(33.3786114568897,30.5940110525657,51.3328850587266));
#41128=CARTESIAN_POINT('Ctrl Pts',(33.9289613661019,32.3955787148589,51.4440148479463));
#41129=CARTESIAN_POINT('Ctrl Pts',(32.7139467505554,33.8351170294417,51.555144637166));
#41130=CARTESIAN_POINT('Ctrl Pts',(30.8455358137404,33.5951761352289,51.6662744263858));
#41131=CARTESIAN_POINT('Ctrl Pts',(30.0336779757772,31.8953473498609,51.7774042156054));
#41132=CARTESIAN_POINT('Ctrl Pts',(31.0213767399516,30.2912955174864,51.8885340048252));
#41133=CARTESIAN_POINT('Ctrl Pts',(32.9047008803004,30.2510315320302,51.9996637940449));
#41134=CARTESIAN_POINT('Ctrl Pts',(33.9600526230799,31.8114044530902,52.1107935832647));
#41135=CARTESIAN_POINT('Ctrl Pts',(33.2215853878362,33.5443781092476,52.2219233724843));
#41136=CARTESIAN_POINT('Ctrl Pts',(31.3651365982299,33.8639533990665,52.3330531617042));
#41137=CARTESIAN_POINT('Ctrl Pts',(30.089707621978,32.4776592840055,52.4441829509237));
#41138=CARTESIAN_POINT('Ctrl Pts',(30.5625580822755,30.6542155186125,52.5553127401437));
#41139=CARTESIAN_POINT('Ctrl Pts',(32.350938671935,30.0624212019666,52.6664425293632));
#41140=CARTESIAN_POINT('Ctrl Pts',(33.8181462226027,31.2438738598914,52.7775723185831));
#41141=CARTESIAN_POINT('Ctrl Pts',(33.6214016570116,33.1173331359233,52.8887021078027));
#41142=CARTESIAN_POINT('Ctrl Pts',(31.9407766092763,33.9682050600104,52.9998318970225));
#41143=CARTESIAN_POINT('Ctrl Pts',(30.3143348819528,33.0178290944304,53.1109616862422));
#41144=CARTESIAN_POINT('Ctrl Pts',(30.2306298081738,31.1358835566457,53.2220914754619));
#41145=CARTESIAN_POINT('Ctrl Pts',(31.7661654057182,30.0448935742819,53.3332212646817));
#41146=CARTESIAN_POINT('Ctrl Pts',(33.5158379925487,30.7429472200775,53.4443510539014));
#41147=CARTESIAN_POINT('Ctrl Pts',(33.877966595439,32.5919341146449,53.5554808431211));
#41148=CARTESIAN_POINT('Ctrl Pts',(32.5219262235475,33.8982139232304,53.6666106323408));
#41149=CARTESIAN_POINT('Ctrl Pts',(30.6871827541888,33.4692125997957,53.7777404215606));
#41150=CARTESIAN_POINT('Ctrl Pts',(30.0559933815144,31.6916070337544,53.8888702107803));
#41151=CARTESIAN_POINT('Ctrl Pts',(30.8184934910026,30.7013650994253,53.9629567369268));
#41152=CARTESIAN_POINT('Ctrl Pts',(31.3249228143251,30.4769022377466,54.));
#41153=CARTESIAN_POINT('Ctrl Pts',(33.6638410485742,32.0009454217316,41.6214803633902));
#41154=CARTESIAN_POINT('Ctrl Pts',(33.664961233117,32.2165036710547,41.6358513744636));
#41155=CARTESIAN_POINT('Ctrl Pts',(33.6260908500516,32.431674600308,41.650222385537));
#41156=CARTESIAN_POINT('Ctrl Pts',(33.5453570674928,32.6297836522019,41.6645933966103));
#41157=CARTESIAN_POINT('Ctrl Pts',(33.3372546082469,33.1404370564071,41.7016366596836));
#41158=CARTESIAN_POINT('Ctrl Pts',(32.8510026283593,33.5377276409124,41.7386799227568));
#41159=CARTESIAN_POINT('Ctrl Pts',(32.3091183519664,33.6398717690552,41.7757231858301));
#41160=CARTESIAN_POINT('Ctrl Pts',(31.7672340755735,33.742015897198,41.8127664489033));
#41161=CARTESIAN_POINT('Ctrl Pts',(31.1697175026754,33.5490135689782,41.8498097119765));
#41162=CARTESIAN_POINT('Ctrl Pts',(30.7899834435371,33.1491743391734,41.8868529750498));
#41163=CARTESIAN_POINT('Ctrl Pts',(30.4102493843987,32.7493351093685,41.923896238123));
#41164=CARTESIAN_POINT('Ctrl Pts',(30.2482978390201,32.1426589779785,41.9609395011963));
#41165=CARTESIAN_POINT('Ctrl Pts',(30.3782397516215,31.6067613225011,41.9979827642696));
#41166=CARTESIAN_POINT('Ctrl Pts',(30.5081816642229,31.0708636670237,42.0350260273428));
#41167=CARTESIAN_POINT('Ctrl Pts',(30.9300170348044,30.6057444874589,42.072069290416));
#41168=CARTESIAN_POINT('Ctrl Pts',(31.4507148731469,30.4242379448684,42.1091125534893));
#41169=CARTESIAN_POINT('Ctrl Pts',(31.9714127114894,30.2427314022778,42.1461558165625));
#41170=CARTESIAN_POINT('Ctrl Pts',(32.590973017593,30.3448374966616,42.1831990796357));
#41171=CARTESIAN_POINT('Ctrl Pts',(33.025889068032,30.6838339691425,42.220242342709));
#41172=CARTESIAN_POINT('Ctrl Pts',(33.422092825981,30.9926560422594,42.2539883496027));
#41173=CARTESIAN_POINT('Ctrl Pts',(33.6650601237133,31.4980736870518,42.2877343564965));
#41174=CARTESIAN_POINT('Ctrl Pts',(33.6682077659727,32.0008552789479,42.3214803633902));
#41175=CARTESIAN_POINT('Ctrl Pts',(32.5301702171886,30.0148256743283,41.));
#41176=CARTESIAN_POINT('Ctrl Pts',(32.5988371051268,30.0402504771426,41.));
#41177=CARTESIAN_POINT('Ctrl Pts',(32.6658006438088,30.0695646181114,41.));
#41178=CARTESIAN_POINT('Ctrl Pts',(32.7308718531578,30.1024741754033,41.));
#41179=CARTESIAN_POINT('Ctrl Pts',(32.7977521620216,30.1362986790245,41.));
#41180=CARTESIAN_POINT('Ctrl Pts',(32.8626342298991,30.1739219849321,41.));
#41181=CARTESIAN_POINT('Ctrl Pts',(32.9252816572652,30.2150696094253,41.));
#41182=CARTESIAN_POINT('Ctrl Pts',(32.9782123144213,30.2498351360624,41.));
#41183=CARTESIAN_POINT('Ctrl Pts',(33.0295474349744,30.2871175547814,41.));
#41184=CARTESIAN_POINT('Ctrl Pts',(33.0791217023575,30.3267693252569,41.));
#41185=CARTESIAN_POINT('Ctrl Pts',(33.101152415551,30.3443904990851,41.));
#41186=CARTESIAN_POINT('Ctrl Pts',(33.1228350751178,30.3624797744732,41.));
#41187=CARTESIAN_POINT('Ctrl Pts',(33.144153618539,30.381024926788,41.));
#41188=CARTESIAN_POINT('Ctrl Pts',(33.1558677004653,30.3912150898427,41.));
#41189=CARTESIAN_POINT('Ctrl Pts',(33.1674718283393,30.4015429009028,41.));
#41190=CARTESIAN_POINT('Ctrl Pts',(33.1789632030502,30.4120063735654,41.));
#41191=CARTESIAN_POINT('Ctrl Pts',(33.1895551793566,30.4216508988997,41.));
#41192=CARTESIAN_POINT('Ctrl Pts',(33.2000527926184,30.43141219387,41.));
#41193=CARTESIAN_POINT('Ctrl Pts',(33.2104379695418,30.4412732542948,41.));
#41194=CARTESIAN_POINT('Ctrl Pts',(33.2635230176514,30.4916792195395,41.));
#41195=CARTESIAN_POINT('Ctrl Pts',(33.3137680834773,30.544773476948,41.));
#41196=CARTESIAN_POINT('Ctrl Pts',(33.3609544746693,30.6002966936962,41.));
#41197=CARTESIAN_POINT('Ctrl Pts',(33.4077742912829,30.6553885699823,41.));
#41198=CARTESIAN_POINT('Ctrl Pts',(33.4515832805539,30.7128726958201,41.));
#41199=CARTESIAN_POINT('Ctrl Pts',(33.4921230168721,30.7725199761025,41.));
#41200=CARTESIAN_POINT('Ctrl Pts',(33.5258091298193,30.8220833231556,41.));
#41201=CARTESIAN_POINT('Ctrl Pts',(33.5572373028608,30.8731408983435,41.));
#41202=CARTESIAN_POINT('Ctrl Pts',(33.5862316727688,30.9255677386219,41.));
#41203=CARTESIAN_POINT('Ctrl Pts',(33.5983395518361,30.947460880083,41.));
#41204=CARTESIAN_POINT('Ctrl Pts',(33.6100226907185,30.9695928397964,41.));
#41205=CARTESIAN_POINT('Ctrl Pts',(33.6212668406506,30.9919546008952,41.));
#41206=CARTESIAN_POINT('Ctrl Pts',(33.6264664374306,31.0022952795331,41.));
#41207=CARTESIAN_POINT('Ctrl Pts',(33.6315721490351,31.0126850985308,41.));
#41208=CARTESIAN_POINT('Ctrl Pts',(33.6365825013037,31.0231231642912,41.));
#41209=CARTESIAN_POINT('Ctrl Pts',(33.6418162986447,31.0340267331209,41.));
#41210=CARTESIAN_POINT('Ctrl Pts',(33.6469424358502,31.0449755037995,41.));
#41211=CARTESIAN_POINT('Ctrl Pts',(33.6519578428112,31.0559641469038,41.));
#41212=CARTESIAN_POINT('Ctrl Pts',(33.6804982000358,31.1184954234379,41.));
#41213=CARTESIAN_POINT('Ctrl Pts',(33.705477565471,31.1823600897106,41.));
#41214=CARTESIAN_POINT('Ctrl Pts',(33.72667246219,31.2473538141253,41.));
#41215=CARTESIAN_POINT('Ctrl Pts',(33.7458696283766,31.3062215380506,41.));
#41216=CARTESIAN_POINT('Ctrl Pts',(33.7619617929881,31.3660161089348,41.));
#41217=CARTESIAN_POINT('Ctrl Pts',(33.7747462387311,31.4265905234075,41.));
#41218=CARTESIAN_POINT('Ctrl Pts',(33.7898804231815,31.4982983142678,41.));
#41219=CARTESIAN_POINT('Ctrl Pts',(33.8003798600472,31.571100476734,41.));
#41220=CARTESIAN_POINT('Ctrl Pts',(33.8063196987879,31.6445738174103,41.));
#41221=CARTESIAN_POINT('Ctrl Pts',(33.8076266382734,31.6607401165739,41.));
#41222=CARTESIAN_POINT('Ctrl Pts',(33.8087126104153,31.6769388277567,41.));
#41223=CARTESIAN_POINT('Ctrl Pts',(33.8095780467764,31.6931652787845,41.));
#41224=CARTESIAN_POINT('Ctrl Pts',(33.8104756849897,31.7099954966529,41.));
#41225=CARTESIAN_POINT('Ctrl Pts',(33.8111360806015,31.7268617851126,41.));
#41226=CARTESIAN_POINT('Ctrl Pts',(33.8115591521967,31.7437245298023,41.));
#41227=CARTESIAN_POINT('Ctrl Pts',(33.8132793295231,31.8122871830253,41.));
#41228=CARTESIAN_POINT('Ctrl Pts',(33.8110878793106,31.8808777362401,41.));
#41229=CARTESIAN_POINT('Ctrl Pts',(33.8051053822439,31.9491577488549,41.));
#41230=CARTESIAN_POINT('Ctrl Pts',(33.7991241582521,32.0174232314892,41.));
#41231=CARTESIAN_POINT('Ctrl Pts',(33.7893530469936,32.0853793775203,41.));
#41232=CARTESIAN_POINT('Ctrl Pts',(33.7758629482066,32.1526729298985,41.));
#41233=CARTESIAN_POINT('Ctrl Pts',(33.7661049603147,32.2013493465565,41.));
#41234=CARTESIAN_POINT('Ctrl Pts',(33.7544000471896,32.2496788103789,41.));
#41235=CARTESIAN_POINT('Ctrl Pts',(33.7407608534051,32.2975179819387,41.));
#41236=CARTESIAN_POINT('Ctrl Pts',(33.7305262323088,32.3334156898394,41.));
#41237=CARTESIAN_POINT('Ctrl Pts',(33.7192022175004,32.3690371718178,41.));
#41238=CARTESIAN_POINT('Ctrl Pts',(33.7067902391303,32.4043176898062,41.));
#41239=CARTESIAN_POINT('Ctrl Pts',(33.7026575280213,32.4160647444878,41.));
#41240=CARTESIAN_POINT('Ctrl Pts',(33.6984073867442,32.42776482926,41.));
#41241=CARTESIAN_POINT('Ctrl Pts',(33.6940404826521,32.4394153171815,41.));
#41242=CARTESIAN_POINT('Ctrl Pts',(33.6709167132624,32.5011073512387,41.));
#41243=CARTESIAN_POINT('Ctrl Pts',(33.6445204214222,32.5614158634302,41.));
#41244=CARTESIAN_POINT('Ctrl Pts',(33.6149016024334,32.6200066741332,41.));
#41245=CARTESIAN_POINT('Ctrl Pts',(33.5940761769243,32.6612027314195,41.));
#41246=CARTESIAN_POINT('Ctrl Pts',(33.5716567752548,32.7015490788674,41.));
#41247=CARTESIAN_POINT('Ctrl Pts',(33.5476503862663,32.7409182209529,41.));
#41248=CARTESIAN_POINT('Ctrl Pts',(33.5399365462045,32.7535684894111,41.));
#41249=CARTESIAN_POINT('Ctrl Pts',(33.532057703321,32.7661194535318,41.));
#41250=CARTESIAN_POINT('Ctrl Pts',(33.5240173798602,32.778561300404,41.));
#41251=CARTESIAN_POINT('Ctrl Pts',(33.4897744251705,32.8315499147026,41.));
#41252=CARTESIAN_POINT('Ctrl Pts',(33.4526757599804,32.882454648408,41.));
#41253=CARTESIAN_POINT('Ctrl Pts',(33.412755629387,32.9309602071557,41.));
#41254=CARTESIAN_POINT('Ctrl Pts',(33.3759796454528,32.9756454229281,41.));
#41255=CARTESIAN_POINT('Ctrl Pts',(33.3368085492858,33.0182945959076,41.));
#41256=CARTESIAN_POINT('Ctrl Pts',(33.2952476940792,33.0586283498916,41.));
#41257=CARTESIAN_POINT('Ctrl Pts',(33.2874058553447,33.0662386551351,41.));
#41258=CARTESIAN_POINT('Ctrl Pts',(33.2794788845476,33.0737664244156,41.));
#41259=CARTESIAN_POINT('Ctrl Pts',(33.2714683883714,33.0812109859128,41.));
#41260=CARTESIAN_POINT('Origin',(32.,32.,48.));
#41261=CARTESIAN_POINT('Origin',(32.,-32.,54.));
#41262=CARTESIAN_POINT('Ctrl Pts',(31.3249228143251,-33.5230977622534,54.));
#41263=CARTESIAN_POINT('Ctrl Pts',(31.265239275159,-33.5045114719856,54.));
#41264=CARTESIAN_POINT('Ctrl Pts',(31.206868285946,-33.482350599571,54.));
#41265=CARTESIAN_POINT('Ctrl Pts',(31.1499663996996,-33.4569140176145,54.));
#41266=CARTESIAN_POINT('Ctrl Pts',(31.1138836062791,-33.4407840965766,54.));
#41267=CARTESIAN_POINT('Ctrl Pts',(31.0783915059693,-33.4233358717196,54.));
#41268=CARTESIAN_POINT('Ctrl Pts',(31.0435309165988,-33.4046351138275,54.));
#41269=CARTESIAN_POINT('Ctrl Pts',(31.0197680190607,-33.3918876473705,54.));
#41270=CARTESIAN_POINT('Ctrl Pts',(30.9962985734341,-33.3785580214987,54.));
#41271=CARTESIAN_POINT('Ctrl Pts',(30.973135972271,-33.3646651103166,54.));
#41272=CARTESIAN_POINT('Ctrl Pts',(30.9607872858049,-33.357258377235,54.));
#41273=CARTESIAN_POINT('Ctrl Pts',(30.9485259765169,-33.3496914691038,54.));
#41274=CARTESIAN_POINT('Ctrl Pts',(30.9363661582946,-33.3419751431426,54.));
#41275=CARTESIAN_POINT('Ctrl Pts',(30.8806643177476,-33.3066281050175,54.));
#41276=CARTESIAN_POINT('Ctrl Pts',(30.8270262511519,-33.2681116533153,54.));
#41277=CARTESIAN_POINT('Ctrl Pts',(30.7756337832862,-33.2267282656662,54.));
#41278=CARTESIAN_POINT('Ctrl Pts',(30.7385650270783,-33.196878936153,54.));
#41279=CARTESIAN_POINT('Ctrl Pts',(30.7026646421898,-33.1655368474349,54.));
#41280=CARTESIAN_POINT('Ctrl Pts',(30.6680061457107,-33.1327996377017,54.));
#41281=CARTESIAN_POINT('Ctrl Pts',(30.6585368474332,-33.12385526806,54.));
#41282=CARTESIAN_POINT('Ctrl Pts',(30.6491602875156,-33.1148066861414,54.));
#41283=CARTESIAN_POINT('Ctrl Pts',(30.6398780493963,-33.1056557310545,54.));
#41284=CARTESIAN_POINT('Ctrl Pts',(30.6303147814348,-33.0962277208618,54.));
#41285=CARTESIAN_POINT('Ctrl Pts',(30.6208573412613,-33.0866966156126,54.));
#41286=CARTESIAN_POINT('Ctrl Pts',(30.6115109509391,-33.0770688360442,54.));
#41287=CARTESIAN_POINT('Ctrl Pts',(30.564248583844,-33.0283835536427,54.));
#41288=CARTESIAN_POINT('Ctrl Pts',(30.5197931029259,-32.977199343729,54.));
#41289=CARTESIAN_POINT('Ctrl Pts',(30.4783282142722,-32.9238232967636,54.));
#41290=CARTESIAN_POINT('Ctrl Pts',(30.4362641057054,-32.869675898632,54.));
#41291=CARTESIAN_POINT('Ctrl Pts',(30.397276759,-32.8132722746407,54.));
#41292=CARTESIAN_POINT('Ctrl Pts',(30.3615823177727,-32.7548861115473,54.));
#41293=CARTESIAN_POINT('Ctrl Pts',(30.3394716332882,-32.7187191907038,54.));
#41294=CARTESIAN_POINT('Ctrl Pts',(30.3186249995123,-32.6817906574975,54.));
#41295=CARTESIAN_POINT('Ctrl Pts',(30.2991007045613,-32.6441582896561,54.));
#41296=CARTESIAN_POINT('Ctrl Pts',(30.2831164151376,-32.6133491536137,54.));
#41297=CARTESIAN_POINT('Ctrl Pts',(30.2680185026127,-32.5820681575949,54.));
#41298=CARTESIAN_POINT('Ctrl Pts',(30.2538422753457,-32.5503447932022,54.));
#41299=CARTESIAN_POINT('Ctrl Pts',(30.2480302988927,-32.537338833056,54.));
#41300=CARTESIAN_POINT('Ctrl Pts',(30.2423723901086,-32.5242560222887,54.));
#41301=CARTESIAN_POINT('Ctrl Pts',(30.2368801512033,-32.5111208799825,54.));
#41302=CARTESIAN_POINT('Ctrl Pts',(30.2096895647203,-32.446092349906,54.));
#41303=CARTESIAN_POINT('Ctrl Pts',(30.1865046901109,-32.3796719815527,54.));
#41304=CARTESIAN_POINT('Ctrl Pts',(30.1675371008066,-32.3121549062884,54.));
#41305=CARTESIAN_POINT('Ctrl Pts',(30.1654370835708,-32.3046796800225,54.));
#41306=CARTESIAN_POINT('Ctrl Pts',(30.1633887977462,-32.2971909716448,54.));
#41307=CARTESIAN_POINT('Ctrl Pts',(30.1613925585069,-32.2896891540652,54.));
#41308=CARTESIAN_POINT('Ctrl Pts',(30.1440544308544,-32.2245329001155,54.));
#41309=CARTESIAN_POINT('Ctrl Pts',(30.1306386024233,-32.1583897935046,54.));
#41310=CARTESIAN_POINT('Ctrl Pts',(30.1209910276371,-32.091564292141,54.));
#41311=CARTESIAN_POINT('Ctrl Pts',(30.1106125640439,-32.0196761701662,54.));
#41312=CARTESIAN_POINT('Ctrl Pts',(30.1045943189643,-31.9469975500423,54.));
#41313=CARTESIAN_POINT('Ctrl Pts',(30.1028046617085,-31.8738849141495,54.));
#41314=CARTESIAN_POINT('Ctrl Pts',(30.1024845931803,-31.8608091960565,54.));
#41315=CARTESIAN_POINT('Ctrl Pts',(30.1022999347513,-31.8477195615237,54.));
#41316=CARTESIAN_POINT('Ctrl Pts',(30.1022501401139,-31.834618015092,54.));
#41317=CARTESIAN_POINT('Ctrl Pts',(30.1022051724613,-31.8227865043478,54.));
#41318=CARTESIAN_POINT('Ctrl Pts',(30.1022702435749,-31.8109538847267,54.));
#41319=CARTESIAN_POINT('Ctrl Pts',(30.1024444017349,-31.7991251289033,54.));
#41320=CARTESIAN_POINT('Ctrl Pts',(30.1034906362357,-31.7280652805266,54.));
#41321=CARTESIAN_POINT('Ctrl Pts',(30.1084694479729,-31.657107539816,54.));
#41322=CARTESIAN_POINT('Ctrl Pts',(30.1172007059819,-31.5865875101679,54.));
#41323=CARTESIAN_POINT('Ctrl Pts',(30.1261162000589,-31.5145794552014,54.));
#41324=CARTESIAN_POINT('Ctrl Pts',(30.1389441161484,-31.4430268429001,54.));
#41325=CARTESIAN_POINT('Ctrl Pts',(30.1555453764766,-31.3722707824218,54.));
#41326=CARTESIAN_POINT('Ctrl Pts',(30.1722475569473,-31.3010845912446,54.));
#41327=CARTESIAN_POINT('Ctrl Pts',(30.1927691766452,-31.2307035954258,54.));
#41328=CARTESIAN_POINT('Ctrl Pts',(30.2170210079531,-31.1614742347,54.));
#41329=CARTESIAN_POINT('Ctrl Pts',(30.2230020127514,-31.1444008379149,54.));
#41330=CARTESIAN_POINT('Ctrl Pts',(30.2292101405796,-31.1273975251947,54.));
#41331=CARTESIAN_POINT('Ctrl Pts',(30.2356445302325,-31.1104696030387,54.));
#41332=CARTESIAN_POINT('Ctrl Pts',(30.2407135367379,-31.0971338008628,54.));
#41333=CARTESIAN_POINT('Ctrl Pts',(30.2459237428321,-31.0838431856506,54.));
#41334=CARTESIAN_POINT('Ctrl Pts',(30.2512662871439,-31.0706205546988,54.));
#41335=CARTESIAN_POINT('Ctrl Pts',(30.2794914752907,-31.0007640921922,54.));
#41336=CARTESIAN_POINT('Ctrl Pts',(30.3114528952479,-30.9326785760022,54.));
#41337=CARTESIAN_POINT('Ctrl Pts',(30.3469924394571,-30.8667213482137,54.));
#41338=CARTESIAN_POINT('Ctrl Pts',(30.3825709935462,-30.8006917226613,54.));
#41339=CARTESIAN_POINT('Ctrl Pts',(30.4217357025888,-30.7367939449245,54.));
#41340=CARTESIAN_POINT('Ctrl Pts',(30.4643797046174,-30.6753909583728,54.));
#41341=CARTESIAN_POINT('Ctrl Pts',(30.5060535838732,-30.6153848490545,54.));
#41342=CARTESIAN_POINT('Ctrl Pts',(30.5510505920688,-30.5577603295061,54.));
#41343=CARTESIAN_POINT('Ctrl Pts',(30.5993163303218,-30.5028757509615,54.));
#41344=CARTESIAN_POINT('Ctrl Pts',(30.6096515549672,-30.491123222784,54.));
#41345=CARTESIAN_POINT('Ctrl Pts',(30.6201368170775,-30.4794964310409,54.));
#41346=CARTESIAN_POINT('Ctrl Pts',(30.6307718389113,-30.4679990812668,54.));
#41347=CARTESIAN_POINT('Ctrl Pts',(30.6398828867194,-30.4581492751173,54.));
#41348=CARTESIAN_POINT('Ctrl Pts',(30.6491038508474,-30.448394472897,54.));
#41349=CARTESIAN_POINT('Ctrl Pts',(30.6584328706692,-30.4387350900139,54.));
#41350=CARTESIAN_POINT('Ctrl Pts',(31.6163320011532,-29.9813874990081,54.));
#41351=CARTESIAN_POINT('Ctrl Pts',(31.6906497010824,-29.9743669064257,54.));
#41352=CARTESIAN_POINT('Ctrl Pts',(31.7652155019048,-29.9717482581011,54.));
#41353=CARTESIAN_POINT('Ctrl Pts',(31.8397072864826,-29.973367958639,54.));
#41354=CARTESIAN_POINT('Ctrl Pts',(31.912240978847,-29.9749450837032,54.));
#41355=CARTESIAN_POINT('Ctrl Pts',(31.9847052775767,-29.9805413173162,54.));
#41356=CARTESIAN_POINT('Ctrl Pts',(32.0567896040968,-29.9900494850227,54.));
#41357=CARTESIAN_POINT('Ctrl Pts',(32.0728797819135,-29.9921718341726,54.));
#41358=CARTESIAN_POINT('Ctrl Pts',(32.0889530810813,-29.9944895851625,54.));
#41359=CARTESIAN_POINT('Ctrl Pts',(32.1049990789946,-29.9970007294107,54.));
#41360=CARTESIAN_POINT('Ctrl Pts',(32.1786326509453,-30.0085241336686,54.));
#41361=CARTESIAN_POINT('Ctrl Pts',(32.2515465731326,-30.0240920503004,54.));
#41362=CARTESIAN_POINT('Ctrl Pts',(32.3234089125773,-30.0435649879731,54.));
#41363=CARTESIAN_POINT('Ctrl Pts',(32.3738561635597,-30.0572349600577,54.));
#41364=CARTESIAN_POINT('Ctrl Pts',(32.4237849187537,-30.0728304248785,54.));
#41365=CARTESIAN_POINT('Ctrl Pts',(32.473072408561,-30.0903162675955,54.));
#41366=CARTESIAN_POINT('Ctrl Pts',(32.4917998053197,-30.0969602317232,54.));
#41367=CARTESIAN_POINT('Ctrl Pts',(32.5104345384574,-30.1038772152795,54.));
#41368=CARTESIAN_POINT('Ctrl Pts',(32.5289695397006,-30.1110656544418,54.));
#41369=CARTESIAN_POINT('Ctrl Pts',(32.5466571041536,-30.1179254317535,54.));
#41370=CARTESIAN_POINT('Ctrl Pts',(32.5642593093968,-30.1250348632197,54.));
#41371=CARTESIAN_POINT('Ctrl Pts',(32.5817390991713,-30.1323793623939,54.));
#41372=CARTESIAN_POINT('Ctrl Pts',(32.6486662599213,-30.1605002084223,54.));
#41373=CARTESIAN_POINT('Ctrl Pts',(32.7138732955257,-30.1920890980459,54.));
#41374=CARTESIAN_POINT('Ctrl Pts',(32.7770519997321,-30.2270188807991,54.));
#41375=CARTESIAN_POINT('Ctrl Pts',(32.8388737020017,-30.2611984141851,54.));
#41376=CARTESIAN_POINT('Ctrl Pts',(32.8987539659087,-30.2985774919006,54.));
#41377=CARTESIAN_POINT('Ctrl Pts',(32.9563716570095,-30.3390737986648,54.));
#41378=CARTESIAN_POINT('Ctrl Pts',(33.012725896401,-30.3786820946978,54.));
#41379=CARTESIAN_POINT('Ctrl Pts',(33.0669162651064,-30.4212729344113,54.));
#41380=CARTESIAN_POINT('Ctrl Pts',(33.1186018592923,-30.4667965224927,54.));
#41381=CARTESIAN_POINT('Ctrl Pts',(33.1354286838459,-30.4816172368864,54.));
#41382=CARTESIAN_POINT('Ctrl Pts',(33.1519896670425,-30.4967489798192,54.));
#41383=CARTESIAN_POINT('Ctrl Pts',(33.1682719417363,-30.5121905362843,54.));
#41384=CARTESIAN_POINT('Ctrl Pts',(33.1774025508037,-30.5208496958996,54.));
#41385=CARTESIAN_POINT('Ctrl Pts',(33.1864463369616,-30.5296072430981,54.));
#41386=CARTESIAN_POINT('Ctrl Pts',(33.1953885762173,-30.5384503466276,54.));
#41387=CARTESIAN_POINT('Ctrl Pts',(33.2439540244105,-30.5864773870649,54.));
#41388=CARTESIAN_POINT('Ctrl Pts',(33.2896151649663,-30.6371069762407,54.));
#41389=CARTESIAN_POINT('Ctrl Pts',(33.3320796339295,-30.6902581242221,54.));
#41390=CARTESIAN_POINT('Ctrl Pts',(33.33818556757,-30.6979006872969,54.));
#41391=CARTESIAN_POINT('Ctrl Pts',(33.3442253363571,-30.70559543444,54.));
#41392=CARTESIAN_POINT('Ctrl Pts',(33.3501979952662,-30.7133421733983,54.));
#41393=CARTESIAN_POINT('Ctrl Pts',(33.3925564663094,-30.76828253126,54.));
#41394=CARTESIAN_POINT('Ctrl Pts',(33.4315435515063,-30.8258365623855,54.));
#41395=CARTESIAN_POINT('Ctrl Pts',(33.4670920125223,-30.8856420553392,54.));
#41396=CARTESIAN_POINT('Ctrl Pts',(33.5002538459271,-30.9414323691067,54.));
#41397=CARTESIAN_POINT('Ctrl Pts',(33.5304228740683,-30.9991829559989,54.));
#41398=CARTESIAN_POINT('Ctrl Pts',(33.5575048000099,-31.0586052133472,54.));
#41399=CARTESIAN_POINT('Ctrl Pts',(33.5633986166787,-31.0715372290249,54.));
#41400=CARTESIAN_POINT('Ctrl Pts',(33.5691460742209,-31.0845484113474,54.));
#41401=CARTESIAN_POINT('Ctrl Pts',(33.5747459551106,-31.0976357581545,54.));
#41402=CARTESIAN_POINT('Ctrl Pts',(33.5792732531105,-31.1082163973129,54.));
#41403=CARTESIAN_POINT('Ctrl Pts',(33.5837038690107,-31.1188465199639,54.));
#41404=CARTESIAN_POINT('Ctrl Pts',(33.5880321351824,-31.1295115045319,54.));
#41405=CARTESIAN_POINT('Ctrl Pts',(33.613744906356,-31.1928685849159,54.));
#41406=CARTESIAN_POINT('Ctrl Pts',(33.6359003814639,-31.2575713836811,54.));
#41407=CARTESIAN_POINT('Ctrl Pts',(33.6544522928069,-31.3232698329539,54.));
#41408=CARTESIAN_POINT('Ctrl Pts',(33.6729185655388,-31.3886650076021,54.));
#41409=CARTESIAN_POINT('Ctrl Pts',(33.6878144745088,-31.4550477976694,54.));
#41410=CARTESIAN_POINT('Ctrl Pts',(33.6990433279385,-31.5220755917657,54.));
#41411=CARTESIAN_POINT('Ctrl Pts',(33.7100316003106,-31.5876672982249,54.));
#41412=CARTESIAN_POINT('Ctrl Pts',(33.7175081391197,-31.6538776300524,54.));
#41413=CARTESIAN_POINT('Ctrl Pts',(33.7213344466344,-31.7203726467958,54.));
#41414=CARTESIAN_POINT('Ctrl Pts',(33.7224477448494,-31.7397199635403,54.));
#41415=CARTESIAN_POINT('Ctrl Pts',(33.7232517169047,-31.7590912458322,54.));
#41416=CARTESIAN_POINT('Ctrl Pts',(33.7237421900973,-31.7784778815483,54.));
#41417=CARTESIAN_POINT('Ctrl Pts',(33.7240143304393,-31.7892346074059,54.));
#41418=CARTESIAN_POINT('Ctrl Pts',(33.7241897036422,-31.7999863091244,54.));
#41419=CARTESIAN_POINT('Ctrl Pts',(33.7242680787914,-31.8107315297782,54.));
#41420=CARTESIAN_POINT('Ctrl Pts',(33.7247442136253,-31.8760095407784,54.));
#41421=CARTESIAN_POINT('Ctrl Pts',(33.7216445542006,-31.9410503644791,54.));
#41422=CARTESIAN_POINT('Ctrl Pts',(33.7148888654324,-32.0055441705781,54.));
#41423=CARTESIAN_POINT('Ctrl Pts',(33.7079758296589,-32.0715401043794,54.));
#41424=CARTESIAN_POINT('Ctrl Pts',(33.6972346760188,-32.1369643866012,54.));
#41425=CARTESIAN_POINT('Ctrl Pts',(33.6825254951079,-32.2014643004376,54.));
#41426=CARTESIAN_POINT('Ctrl Pts',(33.6688931922852,-32.2612420924698,54.));
#41427=CARTESIAN_POINT('Ctrl Pts',(33.6518520468801,-32.3202263589063,54.));
#41428=CARTESIAN_POINT('Ctrl Pts',(33.6312489060068,-32.3781081241769,54.));
#41429=CARTESIAN_POINT('Ctrl Pts',(33.6296213694678,-32.3826804701361,54.));
#41430=CARTESIAN_POINT('Ctrl Pts',(33.6279715848248,-32.3872459188163,54.));
#41431=CARTESIAN_POINT('Ctrl Pts',(33.6262994659155,-32.3918043085367,54.));
#41432=CARTESIAN_POINT('Ctrl Pts',(33.6225368115429,-32.4020617399414,54.));
#41433=CARTESIAN_POINT('Ctrl Pts',(33.6186610677504,-32.4122834302941,54.));
#41434=CARTESIAN_POINT('Ctrl Pts',(33.6146732908669,-32.4224680167337,54.));
#41435=CARTESIAN_POINT('Origin',(32.,-32.,39.4540747194623));
#41436=CARTESIAN_POINT('Ctrl Pts',(34.0565678057143,-31.9985073856871,41.2040747194623));
#41437=CARTESIAN_POINT('Ctrl Pts',(34.057384193637,-31.9004172745425,41.2094078928853));
#41438=CARTESIAN_POINT('Ctrl Pts',(34.006411839884,-31.1218371113704,41.2517843293816));
#41439=CARTESIAN_POINT('Ctrl Pts',(33.0117214699854,-29.7919912031069,41.3312040289512));
#41440=CARTESIAN_POINT('Ctrl Pts',(30.6939306582022,-29.9526094198962,41.4423338181709));
#41441=CARTESIAN_POINT('Ctrl Pts',(29.5714563100008,-31.9866292389199,41.5534636073906));
#41442=CARTESIAN_POINT('Ctrl Pts',(30.6715507437682,-34.0330616484485,41.6645933966103));
#41443=CARTESIAN_POINT('Ctrl Pts',(32.9874316054104,-34.2187692724043,41.7757231858301));
#41444=CARTESIAN_POINT('Ctrl Pts',(34.0018419810914,-32.893577087834,41.8555502934474));
#41445=CARTESIAN_POINT('Ctrl Pts',(34.0572700298053,-32.1072436615327,41.8983341379915));
#41446=CARTESIAN_POINT('Ctrl Pts',(34.056362032224,-32.0016080177294,41.9040747194623));
#41447=CARTESIAN_POINT('Ctrl Pts',(34.0526762468981,-32.0023611642388,41.1459252805377));
#41448=CARTESIAN_POINT('Ctrl Pts',(34.0491258424523,-31.5322384053065,41.1713700465049));
#41449=CARTESIAN_POINT('Ctrl Pts',(33.656679719616,-30.3706653288645,41.2338580755454));
#41450=CARTESIAN_POINT('Ctrl Pts',(31.7284038562778,-29.5872042670172,41.3333893676592));
#41451=CARTESIAN_POINT('Ctrl Pts',(29.825627898444,-30.918441305227,41.4445191568789));
#41452=CARTESIAN_POINT('Ctrl Pts',(29.9119860544063,-33.2405970018638,41.5556489460987));
#41453=CARTESIAN_POINT('Ctrl Pts',(31.9096898625478,-34.4268228681169,41.6667787353183));
#41454=CARTESIAN_POINT('Ctrl Pts',(33.7208347448527,-33.5261026599319,41.7635375134647));
#41455=CARTESIAN_POINT('Ctrl Pts',(34.0499076026638,-32.4182605719717,41.8232530285378));
#41456=CARTESIAN_POINT('Ctrl Pts',(34.0520872241698,-31.9988339725263,41.8459252805377));
#41457=CARTESIAN_POINT('Ctrl Pts',(30.7309291201476,-30.9206413469515,41.));
#41458=CARTESIAN_POINT('Ctrl Pts',(30.3720428517593,-31.3426068457262,41.0370432630732));
#41459=CARTESIAN_POINT('Ctrl Pts',(30.1147036008868,-32.565620122978,41.1111297892197));
#41460=CARTESIAN_POINT('Ctrl Pts',(31.4546601281911,-33.8933249778742,41.2222595784395));
#41461=CARTESIAN_POINT('Ctrl Pts',(33.293843349898,-33.4837762398447,41.3333893676592));
#41462=CARTESIAN_POINT('Ctrl Pts',(33.9488200270038,-31.7184950982882,41.4445191568789));
#41463=CARTESIAN_POINT('Ctrl Pts',(32.8203080515856,-30.2097371185673,41.5556489460986));
#41464=CARTESIAN_POINT('Ctrl Pts',(30.941033447653,-30.3399670488123,41.6667787353184));
#41465=CARTESIAN_POINT('Ctrl Pts',(30.0309264934718,-31.9891589303032,41.7779085245381));
#41466=CARTESIAN_POINT('Ctrl Pts',(30.9228877182713,-33.6484149927315,41.8890383137578));
#41467=CARTESIAN_POINT('Ctrl Pts',(32.8006137265428,-33.7989875205381,42.0001681029776));
#41468=CARTESIAN_POINT('Ctrl Pts',(33.9456250655374,-32.303182554366,42.1112978921973));
#41469=CARTESIAN_POINT('Ctrl Pts',(33.3100222870931,-30.5298898271833,42.222427681417));
#41470=CARTESIAN_POINT('Ctrl Pts',(31.4755008922015,-30.1020352696771,42.3335574706367));
#41471=CARTESIAN_POINT('Ctrl Pts',(30.1209956079544,-31.4111727618922,42.4446872598565));
#41472=CARTESIAN_POINT('Ctrl Pts',(30.4861346576737,-33.2592009254551,42.5558170490762));
#41473=CARTESIAN_POINT('Ctrl Pts',(32.2367469064035,-33.9548208610104,42.6669468382959));
#41474=CARTESIAN_POINT('Ctrl Pts',(33.7706909260737,-32.8614105481285,42.7780766275156));
#41475=CARTESIAN_POINT('Ctrl Pts',(33.6841178265537,-30.9796463378902,42.8892064167354));
#41476=CARTESIAN_POINT('Ctrl Pts',(32.0562583485925,-30.0316988881712,43.0003362059551));
#41477=CARTESIAN_POINT('Ctrl Pts',(30.3769118436706,-30.8851191927514,43.1114659951748));
#41478=CARTESIAN_POINT('Ctrl Pts',(30.1829980159574,-32.7588663611027,43.2225957843945));
#41479=CARTESIAN_POINT('Ctrl Pts',(31.6519847003862,-33.9381072454552,43.3337255736142));
#41480=CARTESIAN_POINT('Ctrl Pts',(33.439471212492,-33.3436134067076,43.444855362834));
#41481=CARTESIAN_POINT('Ctrl Pts',(33.9095692815731,-31.5194591439489,43.5559851520537));
#41482=CARTESIAN_POINT('Ctrl Pts',(32.6320502524575,-30.1350906639621,43.6671149412734));
#41483=CARTESIAN_POINT('Ctrl Pts',(30.7760856866517,-30.4574669829232,43.7782447304932));
#41484=CARTESIAN_POINT('Ctrl Pts',(30.0402342275943,-32.1915527916928,43.8893745197128));
#41485=CARTESIAN_POINT('Ctrl Pts',(31.0979391506829,-33.7503315624784,44.0005043089327));
#41486=CARTESIAN_POINT('Ctrl Pts',(32.9812003806163,-33.707225869006,44.1116340981523));
#41487=CARTESIAN_POINT('Ctrl Pts',(33.9664776628886,-32.1016855742286,44.2227638873721));
#41488=CARTESIAN_POINT('Ctrl Pts',(33.1520559136455,-30.4030837446939,44.3338936765918));
#41489=CARTESIAN_POINT('Ctrl Pts',(31.2832850857612,-30.1659623541582,44.4450234658115));
#41490=CARTESIAN_POINT('Ctrl Pts',(30.0704439749381,-31.6073323277977,44.5561532550313));
#41491=CARTESIAN_POINT('Ctrl Pts',(30.6235116130882,-33.4080674967277,44.6672830442509));
#41492=CARTESIAN_POINT('Ctrl Pts',(32.4363264955448,-33.9201545625114,44.7784128334708));
#41493=CARTESIAN_POINT('Ctrl Pts',(33.8498201010428,-32.6749369958924,44.8895426226904));
#41494=CARTESIAN_POINT('Ctrl Pts',(33.5703784105299,-30.8120244100204,45.0006724119102));
#41495=CARTESIAN_POINT('Ctrl Pts',(31.8537434287449,-30.0363342010384,45.1118022011298));
#41496=CARTESIAN_POINT('Ctrl Pts',(30.270960874886,-31.0577696361976,45.2229319903497));
#41497=CARTESIAN_POINT('Ctrl Pts',(30.270576177683,-32.9415240822457,45.3340617795693));
#41498=CARTESIAN_POINT('Ctrl Pts',(31.852941407844,-33.9636058986261,45.4451915687891));
#41499=CARTESIAN_POINT('Ctrl Pts',(33.5698930667622,-33.1886168910032,45.5563213580087));
#41500=CARTESIAN_POINT('Ctrl Pts',(33.850095615761,-31.3258185947475,45.6674511472286));
#41501=CARTESIAN_POINT('Ctrl Pts',(32.4371107206668,-30.0800238093861,45.7785809364483));
#41502=CARTESIAN_POINT('Ctrl Pts',(30.6240868342867,-30.5913704123997,45.8897107256679));
#41503=CARTESIAN_POINT('Ctrl Pts',(30.0702837560105,-32.3918795380334,46.0008405148877));
#41504=CARTESIAN_POINT('Ctrl Pts',(31.2825360573322,-33.8337447602155,46.1119703041074));
#41505=CARTESIAN_POINT('Ctrl Pts',(33.151403578411,-33.5973866639823,46.2231000933271));
#41506=CARTESIAN_POINT('Ctrl Pts',(33.9665190309799,-31.8991176158095,46.3342298825469));
#41507=CARTESIAN_POINT('Ctrl Pts',(32.9818975924069,-30.293175031624,46.4453596717666));
#41508=CARTESIAN_POINT('Ctrl Pts',(31.098654125499,-30.2493001487501,46.5564894609863));
#41509=CARTESIAN_POINT('Ctrl Pts',(30.0403126282455,-31.8076467841909,46.6676192502061));
#41510=CARTESIAN_POINT('Ctrl Pts',(30.7754557616971,-33.5420329967564,46.7787490394258));
#41511=CARTESIAN_POINT('Ctrl Pts',(32.6312885024143,-33.8651673333419,46.8898788286455));
#41512=CARTESIAN_POINT('Ctrl Pts',(33.9093728517606,-32.4813207533504,47.0010086178652));
#41513=CARTESIAN_POINT('Ctrl Pts',(33.4400198734621,-30.6569746395988,47.1121384070849));
#41514=CARTESIAN_POINT('Ctrl Pts',(31.6527763233362,-30.0617507711828,47.2232681963047));
#41515=CARTESIAN_POINT('Ctrl Pts',(30.1833081166092,-31.2403915775427,47.3343979855244));
#41516=CARTESIAN_POINT('Ctrl Pts',(30.3764566203582,-33.1142177745252,47.4455277747442));
#41517=CARTESIAN_POINT('Ctrl Pts',(32.0554544185607,-33.9683239474508,47.5566575639638));
#41518=CARTESIAN_POINT('Ctrl Pts',(33.6837009342745,-33.0210413892538,47.6677873531837));
#41519=CARTESIAN_POINT('Ctrl Pts',(33.7710426139166,-31.1393128243445,47.7789171424032));
#41520=CARTESIAN_POINT('Ctrl Pts',(32.2375452994596,-30.0452758288314,47.8900469316231));
#41521=CARTESIAN_POINT('Ctrl Pts',(30.4866491030086,-30.7401811966708,48.0011767208427));
#41522=CARTESIAN_POINT('Ctrl Pts',(30.1207552358772,-32.5880590711511,48.1123065100626));
#41523=CARTESIAN_POINT('Ctrl Pts',(31.47472579731,-33.897751660949,48.2234362992821));
#41524=CARTESIAN_POINT('Ctrl Pts',(33.3094216126832,-33.4706425109062,48.3345660885021));
#41525=CARTESIAN_POINT('Ctrl Pts',(33.9457489682148,-31.6976172833359,48.4456958777216));
#41526=CARTESIAN_POINT('Ctrl Pts',(32.8013479688052,-30.2013294388527,48.5568256669415));
#41527=CARTESIAN_POINT('Ctrl Pts',(30.9235619986018,-30.3511653861614,48.6679554561611));
#41528=CARTESIAN_POINT('Ctrl Pts',(30.0309204137941,-32.0099968911885,48.7790852453809));
#41529=CARTESIAN_POINT('Ctrl Pts',(30.9403591125031,-33.6596793498116,48.8902150346005));
#41530=CARTESIAN_POINT('Ctrl Pts',(32.8195696601223,-33.7904412659602,49.0013448238204));
#41531=CARTESIAN_POINT('Ctrl Pts',(33.9487189426605,-32.2826107520291,49.11247461304));
#41532=CARTESIAN_POINT('Ctrl Pts',(33.2944217818527,-30.5161379426269,49.2236044022598));
#41533=CARTESIAN_POINT('Ctrl Pts',(31.455483843713,-30.1076795963187,49.3347341914795));
#41534=CARTESIAN_POINT('Ctrl Pts',(30.1148811867754,-31.4310523620993,49.4458639806992));
#41535=CARTESIAN_POINT('Ctrl Pts',(30.4995188244386,-33.2751198361065,49.556993769919));
#41536=CARTESIAN_POINT('Ctrl Pts',(32.2573805619349,-33.9522114642078,49.6681235591386));
#41537=CARTESIAN_POINT('Ctrl Pts',(33.7796904003243,-32.8426603311179,49.7792533483585));
#41538=CARTESIAN_POINT('Ctrl Pts',(33.6732468842757,-30.9619156012597,49.8903831375781));
#41539=CARTESIAN_POINT('Ctrl Pts',(32.0354659653448,-30.0312144555721,50.0015129267979));
#41540=CARTESIAN_POINT('Ctrl Pts',(30.3652269795427,-30.9023244895547,50.1126427160176));
#41541=CARTESIAN_POINT('Ctrl Pts',(30.1911145336881,-32.7780152469018,50.2237725052374));
#41542=CARTESIAN_POINT('Ctrl Pts',(31.6724744500558,-33.9416748875081,50.334902294457));
#41543=CARTESIAN_POINT('Ctrl Pts',(33.4535821978664,-33.3283347276548,50.4460320836768));
#41544=CARTESIAN_POINT('Ctrl Pts',(33.9043872816309,-31.4993170302414,50.5571618728964));
#41545=CARTESIAN_POINT('Ctrl Pts',(32.6123177774694,-30.1285189570716,50.6682916621163));
#41546=CARTESIAN_POINT('Ctrl Pts',(30.7598616836728,-30.4704800390206,50.7794214513359));
#41547=CARTESIAN_POINT('Ctrl Pts',(30.0423667282485,-32.2122412023096,50.8905512405557));
#41548=CARTESIAN_POINT('Ctrl Pts',(31.1164765134632,-33.7597615188951,51.0016810297753));
#41549=CARTESIAN_POINT('Ctrl Pts',(32.9991774121812,-33.696767177226,51.1128108189952));
#41550=CARTESIAN_POINT('Ctrl Pts',(33.9674419788235,-32.0809099155954,51.2239406082148));
#41551=CARTESIAN_POINT('Ctrl Pts',(33.1351249826154,-30.391004776719,51.3350703974346));
#41552=CARTESIAN_POINT('Ctrl Pts',(31.2639539119407,-30.1736346172128,51.4462001866543));
#41553=CARTESIAN_POINT('Ctrl Pts',(30.0664042395539,-31.6277342502227,51.5573299758739));
#41554=CARTESIAN_POINT('Ctrl Pts',(30.6384604369997,-33.4225274597867,51.6684597650938));
#41555=CARTESIAN_POINT('Ctrl Pts',(32.4565828795076,-33.9154389659862,51.7795895543135));
#41556=CARTESIAN_POINT('Ctrl Pts',(33.8568456176001,-32.6553615002807,51.8907193435332));
#41557=CARTESIAN_POINT('Ctrl Pts',(33.5577433920753,-30.7955043011809,52.0018491327529));
#41558=CARTESIAN_POINT('Ctrl Pts',(31.8330112894132,-30.0379884943954,52.1129789219727));
#41559=CARTESIAN_POINT('Ctrl Pts',(30.2611054788687,-31.0760843582921,52.2241087111923));
#41560=CARTESIAN_POINT('Ctrl Pts',(30.2806170070421,-32.9597377626332,52.3352385004122));
#41561=CARTESIAN_POINT('Ctrl Pts',(31.8736893420127,-33.9650496446109,52.4463682896318));
#41562=CARTESIAN_POINT('Ctrl Pts',(33.5823595490477,-33.1719692631936,52.5574980788516));
#41563=CARTESIAN_POINT('Ctrl Pts',(33.8428719959032,-31.3063155961969,52.6686278680713));
#41564=CARTESIAN_POINT('Ctrl Pts',(32.416806909947,-30.0755138292301,52.7797576572911));
#41565=CARTESIAN_POINT('Ctrl Pts',(30.6092867728801,-30.6059820117572,52.8908874465107));
#41566=CARTESIAN_POINT('Ctrl Pts',(30.074528117115,-32.4122382091939,53.0020172357305));
#41567=CARTESIAN_POINT('Ctrl Pts',(31.3019487274169,-33.8412226855446,53.1131470249502));
#41568=CARTESIAN_POINT('Ctrl Pts',(33.1682019017076,-33.5851317784421,53.2242768141699));
#41569=CARTESIAN_POINT('Ctrl Pts',(33.965361811241,-31.8783619852648,53.3354066033896));
#41570=CARTESIAN_POINT('Ctrl Pts',(32.9637796720064,-30.2828812659777,53.4465363926094));
#41571=CARTESIAN_POINT('Ctrl Pts',(31.0802839845962,-30.2589537602268,53.557666181829));
#41572=CARTESIAN_POINT('Ctrl Pts',(30.0382506967122,-31.8282846681807,53.6687959710489));
#41573=CARTESIAN_POINT('Ctrl Pts',(30.7920874688999,-33.5550214868453,53.7799257602685));
#41574=CARTESIAN_POINT('Ctrl Pts',(32.6504054262519,-33.8581160689002,53.8910555494883));
#41575=CARTESIAN_POINT('Ctrl Pts',(33.9154419847816,-32.461689344216,54.002185338708));
#41576=CARTESIAN_POINT('Ctrl Pts',(33.4235041713429,-30.6406234847563,54.1133151279277));
#41577=CARTESIAN_POINT('Ctrl Pts',(32.2331222331376,-30.2598665970073,54.1874016540742));
#41578=CARTESIAN_POINT('Ctrl Pts',(31.6889203620495,-30.3633004372052,54.2244449171475));
#41579=CARTESIAN_POINT('Ctrl Pts',(30.6322193753411,-30.8366876301903,40.9251850276175));
#41580=CARTESIAN_POINT('Ctrl Pts',(30.2454185337564,-31.2914740748731,40.9622282906908));
#41581=CARTESIAN_POINT('Ctrl Pts',(29.9680631496753,-32.6096146853645,41.0363148168372));
#41582=CARTESIAN_POINT('Ctrl Pts',(31.4122429863013,-34.0405899008731,41.147444606057));
#41583=CARTESIAN_POINT('Ctrl Pts',(33.3944799249825,-33.5991860063993,41.2585743952767));
#41584=CARTESIAN_POINT('Ctrl Pts',(34.1004014166593,-31.6965993338744,41.3697041844964));
#41585=CARTESIAN_POINT('Ctrl Pts',(32.8841125243855,-30.0704884800805,41.4808339737162));
#41586=CARTESIAN_POINT('Ctrl Pts',(30.8586658511694,-30.2108478391736,41.5919637629359));
#41587=CARTESIAN_POINT('Ctrl Pts',(29.8777697656481,-31.9883156998422,41.7030935521556));
#41588=CARTESIAN_POINT('Ctrl Pts',(30.8391087267702,-33.7766305446372,41.8142233413754));
#41589=CARTESIAN_POINT('Ctrl Pts',(32.862886352832,-33.9389147711602,41.925353130595));
#41590=CARTESIAN_POINT('Ctrl Pts',(34.0969579475357,-32.3267644307185,42.0364829198148));
#41591=CARTESIAN_POINT('Ctrl Pts',(33.4119172779109,-30.415543022525,42.1476127090345));
#41592=CARTESIAN_POINT('Ctrl Pts',(31.4347047681205,-29.9544094615713,42.2587424982542));
#41593=CARTESIAN_POINT('Ctrl Pts',(29.9748445560521,-31.3653731242743,42.369872287474));
#41594=CARTESIAN_POINT('Ctrl Pts',(30.3683845272556,-33.3571429742288,42.4810020766937));
#41595=CARTESIAN_POINT('Ctrl Pts',(32.2551613441515,-34.1068690022105,42.5921318659134));
#41596=CARTESIAN_POINT('Ctrl Pts',(33.9084172360999,-32.9284120188338,42.7032616551332));
#41597=CARTESIAN_POINT('Ctrl Pts',(33.8151103845915,-30.900282094964,42.8143914443528));
#41598=CARTESIAN_POINT('Ctrl Pts',(32.0606341855303,-29.8786022380665,42.9255212335726));
#41599=CARTESIAN_POINT('Ctrl Pts',(30.250666241275,-30.79840252332,43.0366510227923));
#41600=CARTESIAN_POINT('Ctrl Pts',(30.0416695803239,-32.8178918308664,43.1477808120121));
#41601=CARTESIAN_POINT('Ctrl Pts',(31.6249156832344,-34.0888553830443,43.2589106012317));
#41602=CARTESIAN_POINT('Ctrl Pts',(33.5514348847322,-33.4481211521773,43.3700403904515));
#41603=CARTESIAN_POINT('Ctrl Pts',(34.0580977045846,-31.4820821415899,43.4811701796712));
#41604=CARTESIAN_POINT('Ctrl Pts',(32.6812118242147,-29.9900359411961,43.592299968891));
#41605=CARTESIAN_POINT('Ctrl Pts',(30.6808882698222,-30.3374870488719,43.7034297581107));
#41606=CARTESIAN_POINT('Ctrl Pts',(29.8878014656849,-32.2064519809226,43.8145595473304));
#41607=CARTESIAN_POINT('Ctrl Pts',(31.02777585433,-33.8864742985555,43.9256893365501));
#41608=CARTESIAN_POINT('Ctrl Pts',(33.0575192377521,-33.8400157962921,44.0368191257698));
#41609=CARTESIAN_POINT('Ctrl Pts',(34.1194324831063,-32.1095947913117,44.1479489149896));
#41610=CARTESIAN_POINT('Ctrl Pts',(33.2416641042077,-30.2788738218748,44.2590787042093));
#41611=CARTESIAN_POINT('Ctrl Pts',(31.2275382024258,-30.0233088657986,44.3702084934291));
#41612=CARTESIAN_POINT('Ctrl Pts',(29.9203609607839,-31.5767901994327,44.4813382826487));
#41613=CARTESIAN_POINT('Ctrl Pts',(30.5164468150866,-33.5175885530207,44.5924680718685));
#41614=CARTESIAN_POINT('Ctrl Pts',(32.4702644557575,-34.0695063204498,44.7035978610882));
#41615=CARTESIAN_POINT('Ctrl Pts',(33.9937011663249,-32.7274343462632,44.814727650308));
#41616=CARTESIAN_POINT('Ctrl Pts',(33.6925241902605,-30.7196223470743,44.9258574395277));
#41617=CARTESIAN_POINT('Ctrl Pts',(31.8423674299303,-29.8835980907251,45.0369872287474));
#41618=CARTESIAN_POINT('Ctrl Pts',(30.1364742882738,-30.9844819103215,45.1481170179671));
#41619=CARTESIAN_POINT('Ctrl Pts',(30.1360596688943,-33.0147568727565,45.2592468071868));
#41620=CARTESIAN_POINT('Ctrl Pts',(31.8415030269516,-34.1163373498248,45.3703765964066));
#41621=CARTESIAN_POINT('Ctrl Pts',(33.6920010959146,-33.2810688350563,45.4815063856262));
#41622=CARTESIAN_POINT('Ctrl Pts',(33.9939981108845,-31.2733800150573,45.5926361748461));
#41623=CARTESIAN_POINT('Ctrl Pts',(32.4711096787818,-29.9306859254122,45.7037659640657));
#41624=CARTESIAN_POINT('Ctrl Pts',(30.5170667776298,-30.4818056360532,45.8148957532856));
#41625=CARTESIAN_POINT('Ctrl Pts',(29.9201882798498,-32.422360364446,45.9260255425052));
#41626=CARTESIAN_POINT('Ctrl Pts',(31.2267309137324,-33.9763754676053,46.037155331725));
#41627=CARTESIAN_POINT('Ctrl Pts',(33.240961029613,-33.7216331757116,46.1482851209446));
#41628=CARTESIAN_POINT('Ctrl Pts',(34.1194770688537,-31.8912708717411,46.2594149101644));
#41629=CARTESIAN_POINT('Ctrl Pts',(33.0582706794513,-30.1604162868348,46.3705446993841));
#41630=CARTESIAN_POINT('Ctrl Pts',(31.0285464406826,-30.1131287667627,46.4816744886039));
#41631=CARTESIAN_POINT('Ctrl Pts',(29.8878859644261,-31.7926853370829,46.5928042778235));
#41632=CARTESIAN_POINT('Ctrl Pts',(30.6802093486038,-33.661974038671,46.7039340670433));
#41633=CARTESIAN_POINT('Ctrl Pts',(32.6803908244057,-34.0102421234253,46.815063856263));
#41634=CARTESIAN_POINT('Ctrl Pts',(34.0578859962428,-32.5187584169888,46.9261936454828));
#41635=CARTESIAN_POINT('Ctrl Pts',(33.5520262211627,-30.552512633025,47.0373234347024));
#41636=CARTESIAN_POINT('Ctrl Pts',(31.6257688794981,-29.9109915899698,47.1484532239222));
#41637=CARTESIAN_POINT('Ctrl Pts',(30.0420038009492,-31.1813083894214,47.2595830131419));
#41638=CARTESIAN_POINT('Ctrl Pts',(30.2501756101871,-33.2008828725337,47.3707128023617));
#41639=CARTESIAN_POINT('Ctrl Pts',(32.0597677249264,-34.1214223737356,47.4818425915814));
#41640=CARTESIAN_POINT('Ctrl Pts',(33.814661065967,-33.1004591243624,47.5929723808012));
#41641=CARTESIAN_POINT('Ctrl Pts',(33.9087962786145,-31.0723676183549,47.7041021700208));
#41642=CARTESIAN_POINT('Ctrl Pts',(32.2560218371077,-29.8932352082748,47.8152319592406));
#41643=CARTESIAN_POINT('Ctrl Pts',(30.3689389867211,-30.6421910886687,47.9263617484603));
#41644=CARTESIAN_POINT('Ctrl Pts',(29.9745854875673,-32.6337989598886,48.03749153768));
#41645=CARTESIAN_POINT('Ctrl Pts',(31.4338693854861,-34.0453608962819,48.1486213268997));
#41646=CARTESIAN_POINT('Ctrl Pts',(33.4112698823772,-33.5850307214133,48.2597511161195));
#41647=CARTESIAN_POINT('Ctrl Pts',(34.0970914875013,-31.6740976192497,48.3708809053391));
#41648=CARTESIAN_POINT('Ctrl Pts',(32.8636777052743,-30.0614268416845,48.4820106945589));
#41649=CARTESIAN_POINT('Ctrl Pts',(30.839835453375,-30.2229171956593,48.5931404837787));
#41650=CARTESIAN_POINT('Ctrl Pts',(29.8777632130863,-32.010774460506,48.7042702729984));
#41651=CARTESIAN_POINT('Ctrl Pts',(30.8579390654813,-33.7887710559419,48.8154000622181));
#41652=CARTESIAN_POINT('Ctrl Pts',(32.8833167000128,-33.929703779394,48.9265298514378));
#41653=CARTESIAN_POINT('Ctrl Pts',(34.1002924698632,-32.3045925307108,49.0376596406576));
#41654=CARTESIAN_POINT('Ctrl Pts',(33.3951033480182,-30.4007215010895,49.1487894298773));
#41655=CARTESIAN_POINT('Ctrl Pts',(31.4131307713328,-29.960492810218,49.259919219097));
#41656=CARTESIAN_POINT('Ctrl Pts',(29.9682545483917,-31.3867989819005,49.3710490083168));
#41657=CARTESIAN_POINT('Ctrl Pts',(30.3828097294008,-33.3743000754595,49.4821787975364));
#41658=CARTESIAN_POINT('Ctrl Pts',(32.2773999083639,-34.1040566436217,49.5933085867562));
#41659=CARTESIAN_POINT('Ctrl Pts',(33.9181166994692,-32.9082033890855,49.7044383759759));
#41660=CARTESIAN_POINT('Ctrl Pts',(33.8033938883297,-30.8811722419139,49.8155681651957));
#41661=CARTESIAN_POINT('Ctrl Pts',(32.0382245475832,-29.8780801257608,49.9266979544153));
#41662=CARTESIAN_POINT('Ctrl Pts',(30.2380725154165,-30.8169460672487,50.0378277436351));
#41663=CARTESIAN_POINT('Ctrl Pts',(30.0504174098328,-32.8385301383049,50.1489575328548));
#41664=CARTESIAN_POINT('Ctrl Pts',(31.646999148427,-34.092700520265,50.2600873220746));
#41665=CARTESIAN_POINT('Ctrl Pts',(33.5666434382467,-33.431654080471,50.3712171112942));
#41666=CARTESIAN_POINT('Ctrl Pts',(34.0525126429222,-31.4603733518713,50.4823469005141));
#41667=CARTESIAN_POINT('Ctrl Pts',(32.6599445353708,-29.982953079633,50.5934766897336));
#41668=CARTESIAN_POINT('Ctrl Pts',(30.6634023458432,-30.3515122749489,50.7046064789535));
#41669=CARTESIAN_POINT('Ctrl Pts',(29.8900998346124,-32.2287495591319,50.8157362681731));
#41670=CARTESIAN_POINT('Ctrl Pts',(31.0477550738091,-33.8966377274726,50.926866057393));
#41671=CARTESIAN_POINT('Ctrl Pts',(33.0768945428305,-33.8287436158309,51.0379958466126));
#41672=CARTESIAN_POINT('Ctrl Pts',(34.1204718046074,-32.0872031788381,51.1491256358324));
#41673=CARTESIAN_POINT('Ctrl Pts',(33.2234162665272,-30.2658553383336,51.2602554250521));
#41674=CARTESIAN_POINT('Ctrl Pts',(31.2067034284007,-30.0315778860086,51.3713852142719));
#41675=CARTESIAN_POINT('Ctrl Pts',(29.9160070102875,-31.5987790060798,51.4825150034915));
#41676=CARTESIAN_POINT('Ctrl Pts',(30.5325583751517,-33.5331732280924,51.5936447927113));
#41677=CARTESIAN_POINT('Ctrl Pts',(32.4920964037991,-34.064423939581,51.704774581931));
#41678=CARTESIAN_POINT('Ctrl Pts',(34.0012731353756,-32.7063362468262,51.8159043711507));
#41679=CARTESIAN_POINT('Ctrl Pts',(33.6789064060147,-30.7018172857916,51.9270341603705));
#41680=CARTESIAN_POINT('Ctrl Pts',(31.820022721738,-29.8853810568597,52.0381639495902));
#41681=CARTESIAN_POINT('Ctrl Pts',(30.1258523285906,-31.0042211718748,52.1492937388099));
#41682=CARTESIAN_POINT('Ctrl Pts',(30.1468814851308,-33.0343872334662,52.2604235280297));
#41683=CARTESIAN_POINT('Ctrl Pts',(31.8638647585208,-34.1178933919783,52.3715533172493));
#41684=CARTESIAN_POINT('Ctrl Pts',(33.7054372350606,-33.2631263362361,52.4826831064691));
#41685=CARTESIAN_POINT('Ctrl Pts',(33.9862126298382,-31.2523600515833,52.5938128956889));
#41686=CARTESIAN_POINT('Ctrl Pts',(32.4492266150774,-29.9258251539826,52.7049426849085));
#41687=CARTESIAN_POINT('Ctrl Pts',(30.5011155509827,-30.4975537418634,52.8160724741283));
#41688=CARTESIAN_POINT('Ctrl Pts',(29.9247627720828,-32.4443025556973,52.9272022633479));
#41689=CARTESIAN_POINT('Ctrl Pts',(31.2476535228917,-33.9844350342852,53.0383320525678));
#41690=CARTESIAN_POINT('Ctrl Pts',(33.2590659451828,-33.7084250915412,53.1494618417874));
#41691=CARTESIAN_POINT('Ctrl Pts',(34.1182298392761,-31.8689008451631,53.2605916310072));
#41692=CARTESIAN_POINT('Ctrl Pts',(33.038743527047,-30.1493218606453,53.3717214202269));
#41693=CARTESIAN_POINT('Ctrl Pts',(31.0087474497846,-30.1235332468791,53.4828512094467));
#41694=CARTESIAN_POINT('Ctrl Pts',(29.8856636535643,-31.8149284586479,53.5939809986663));
#41695=CARTESIAN_POINT('Ctrl Pts',(30.6981346884947,-33.6759727879679,53.7051107878861));
#41696=CARTESIAN_POINT('Ctrl Pts',(32.700994683846,-34.0026424037911,53.8162405771058));
#41697=CARTESIAN_POINT('Ctrl Pts',(34.0644271931817,-32.497600055013,53.9273703663256));
#41698=CARTESIAN_POINT('Ctrl Pts',(33.53422590936,-30.5348896671691,54.0385001555452));
#41699=CARTESIAN_POINT('Ctrl Pts',(32.2512547397667,-30.1245170851199,54.1125866816917));
#41700=CARTESIAN_POINT('Ctrl Pts',(31.6647242417508,-30.2359961244728,54.149629944765));
#41701=CARTESIAN_POINT('Ctrl Pts',(30.5335096305347,-30.7527339134291,40.850370055235));
#41702=CARTESIAN_POINT('Ctrl Pts',(30.1187942157535,-31.24034130402,40.8874133183083));
#41703=CARTESIAN_POINT('Ctrl Pts',(29.8214226984638,-32.653609247751,40.9614998444547));
#41704=CARTESIAN_POINT('Ctrl Pts',(31.3698258444113,-34.187854823872,41.0726296336745));
#41705=CARTESIAN_POINT('Ctrl Pts',(33.4951165000671,-33.7145957729538,41.1837594228942));
#41706=CARTESIAN_POINT('Ctrl Pts',(34.2519828063147,-31.6747035694605,41.2948892121139));
#41707=CARTESIAN_POINT('Ctrl Pts',(32.9479169971854,-29.9312398415937,41.4060190013337));
#41708=CARTESIAN_POINT('Ctrl Pts',(30.7762982546858,-30.0817286295349,41.5171487905534));
#41709=CARTESIAN_POINT('Ctrl Pts',(29.7246130378245,-31.9874724693811,41.6282785797731));
#41710=CARTESIAN_POINT('Ctrl Pts',(30.7553297352692,-33.9048460965428,41.7394083689928));
#41711=CARTESIAN_POINT('Ctrl Pts',(32.9251589791213,-34.0788420217823,41.8505381582126));
#41712=CARTESIAN_POINT('Ctrl Pts',(34.248290829534,-32.350346307071,41.9616679474322));
#41713=CARTESIAN_POINT('Ctrl Pts',(33.5138122687288,-30.3011962178666,42.0727977366521));
#41714=CARTESIAN_POINT('Ctrl Pts',(31.3939086440396,-29.8067836534655,42.1839275258717));
#41715=CARTESIAN_POINT('Ctrl Pts',(29.8286935041498,-31.3195734866563,42.2950573150915));
#41716=CARTESIAN_POINT('Ctrl Pts',(30.2506343968376,-33.4550850230024,42.4061871043112));
#41717=CARTESIAN_POINT('Ctrl Pts',(32.2735757818995,-34.2589171434105,42.5173168935309));
#41718=CARTESIAN_POINT('Ctrl Pts',(34.0461435461261,-32.9954134895391,42.6284466827507));
#41719=CARTESIAN_POINT('Ctrl Pts',(33.9461029426293,-30.8209178520377,42.7395764719703));
#41720=CARTESIAN_POINT('Ctrl Pts',(32.0650100224681,-29.7255055879618,42.8507062611902));
#41721=CARTESIAN_POINT('Ctrl Pts',(30.1244206388795,-30.7116858538886,42.9618360504098));
#41722=CARTESIAN_POINT('Ctrl Pts',(29.9003411446903,-32.8769173006301,43.0729658396296));
#41723=CARTESIAN_POINT('Ctrl Pts',(31.5978466660826,-34.2396035206334,43.1840956288493));
#41724=CARTESIAN_POINT('Ctrl Pts',(33.6633985569723,-33.5526288976471,43.295225418069));
#41725=CARTESIAN_POINT('Ctrl Pts',(34.2066261275962,-31.444705139231,43.4063552072888));
#41726=CARTESIAN_POINT('Ctrl Pts',(32.730373395972,-29.8449812184301,43.5174849965084));
#41727=CARTESIAN_POINT('Ctrl Pts',(30.5856908529926,-30.2175071148205,43.6286147857282));
#41728=CARTESIAN_POINT('Ctrl Pts',(29.7353687037756,-32.2213511701524,43.7397445749478));
#41729=CARTESIAN_POINT('Ctrl Pts',(30.957612557977,-34.0226170346326,43.8508743641677));
#41730=CARTESIAN_POINT('Ctrl Pts',(33.1338380948878,-33.9728057235782,43.9620041533873));
#41731=CARTESIAN_POINT('Ctrl Pts',(34.272387303324,-32.1175040083948,44.0731339426071));
#41732=CARTESIAN_POINT('Ctrl Pts',(33.3312722947699,-30.1546638990556,44.1842637318268));
#41733=CARTESIAN_POINT('Ctrl Pts',(31.1717913190904,-29.8806553774391,44.2953935210465));
#41734=CARTESIAN_POINT('Ctrl Pts',(29.7702779466297,-31.5462480710675,44.4065233102663));
#41735=CARTESIAN_POINT('Ctrl Pts',(30.409382017085,-33.6271096093139,44.517653099486));
#41736=CARTESIAN_POINT('Ctrl Pts',(32.5042024159702,-34.2188580783882,44.6287828887057));
#41737=CARTESIAN_POINT('Ctrl Pts',(34.1375822316071,-32.779931696634,44.7399126779255));
#41738=CARTESIAN_POINT('Ctrl Pts',(33.8146699699911,-30.6272202841281,44.8510424671452));
#41739=CARTESIAN_POINT('Ctrl Pts',(31.8309914311157,-29.7308619804117,44.9621722563648));
#41740=CARTESIAN_POINT('Ctrl Pts',(30.0019877016615,-30.9111941844455,45.0733020455847));
#41741=CARTESIAN_POINT('Ctrl Pts',(30.0015431601057,-33.0879896632673,45.1844318348043));
#41742=CARTESIAN_POINT('Ctrl Pts',(31.8300646460591,-34.2690688010235,45.2955616240241));
#41743=CARTESIAN_POINT('Ctrl Pts',(33.8141091250671,-33.3735207791094,45.4066914132438));
#41744=CARTESIAN_POINT('Ctrl Pts',(34.1379006060079,-31.2209414353671,45.5178212024636));
#41745=CARTESIAN_POINT('Ctrl Pts',(32.505108636897,-29.7813480414384,45.6289509916832));
#41746=CARTESIAN_POINT('Ctrl Pts',(30.4100467209729,-30.3722408597067,45.740080780903));
#41747=CARTESIAN_POINT('Ctrl Pts',(29.7700928036892,-32.4528411908587,45.8512105701227));
#41748=CARTESIAN_POINT('Ctrl Pts',(31.1709257701325,-34.1190061749949,45.9623403593425));
#41749=CARTESIAN_POINT('Ctrl Pts',(33.3305184808149,-33.8458796874409,46.0734701485621));
#41750=CARTESIAN_POINT('Ctrl Pts',(34.2724351067276,-31.8834241276727,46.1845999377819));
#41751=CARTESIAN_POINT('Ctrl Pts',(33.1346437664958,-30.0276575420456,46.2957297270016));
#41752=CARTESIAN_POINT('Ctrl Pts',(30.9584387558662,-29.9769573847752,46.4068595162214));
#41753=CARTESIAN_POINT('Ctrl Pts',(29.7354593006066,-31.7777238899748,46.517989305441));
#41754=CARTESIAN_POINT('Ctrl Pts',(30.5849629355105,-33.7819150805856,46.6291190946608));
#41755=CARTESIAN_POINT('Ctrl Pts',(32.7294931463973,-34.1553169135087,46.7402488838805));
#41756=CARTESIAN_POINT('Ctrl Pts',(34.2063991407249,-32.5561960806273,46.8513786731002));
#41757=CARTESIAN_POINT('Ctrl Pts',(33.6640325688636,-30.4480506264512,46.96250846232));
#41758=CARTESIAN_POINT('Ctrl Pts',(31.5987614356599,-29.7602324087568,47.0736382515397));
#41759=CARTESIAN_POINT('Ctrl Pts',(29.9006994852894,-31.1222252013001,47.1847680407595));
#41760=CARTESIAN_POINT('Ctrl Pts',(30.1238946000158,-33.2875479705422,47.2958978299791));
#41761=CARTESIAN_POINT('Ctrl Pts',(32.064081031292,-34.2745208000205,47.407027619199));
#41762=CARTESIAN_POINT('Ctrl Pts',(33.9456211976595,-33.1798768594709,47.5181574084186));
#41763=CARTESIAN_POINT('Ctrl Pts',(34.0465499433124,-31.0054224123653,47.6292871976384));
#41764=CARTESIAN_POINT('Ctrl Pts',(32.2744983747557,-29.7411945877182,47.740416986858));
#41765=CARTESIAN_POINT('Ctrl Pts',(30.2512288704335,-30.5442009806667,47.8515467760778));
#41766=CARTESIAN_POINT('Ctrl Pts',(29.8284157392574,-32.6795388486261,47.9626765652975));
#41767=CARTESIAN_POINT('Ctrl Pts',(31.3930129736622,-34.1929701316148,48.0738063545172));
#41768=CARTESIAN_POINT('Ctrl Pts',(33.5131181520712,-33.6994189319205,48.184936143737));
#41769=CARTESIAN_POINT('Ctrl Pts',(34.2484340067877,-31.6505779551634,48.2960659329566));
#41770=CARTESIAN_POINT('Ctrl Pts',(32.9260074417436,-29.9215242445165,48.4071957221765));
#41771=CARTESIAN_POINT('Ctrl Pts',(30.7561089081482,-30.0946690051571,48.5183255113961));
#41772=CARTESIAN_POINT('Ctrl Pts',(29.7246060123785,-32.0115520298237,48.6294553006159));
#41773=CARTESIAN_POINT('Ctrl Pts',(30.7755190184597,-33.9178627620722,48.7405850898356));
#41774=CARTESIAN_POINT('Ctrl Pts',(32.9470637399033,-34.0689662928278,48.8517148790554));
#41775=CARTESIAN_POINT('Ctrl Pts',(34.2518659970659,-32.3265743093926,48.962844668275));
#41776=CARTESIAN_POINT('Ctrl Pts',(33.4957849141838,-30.2853050595522,49.0739744574949));
#41777=CARTESIAN_POINT('Ctrl Pts',(31.3707776989525,-29.8133060241173,49.1851042467144));
#41778=CARTESIAN_POINT('Ctrl Pts',(29.8216279100082,-31.3425456017016,49.2962340359344));
#41779=CARTESIAN_POINT('Ctrl Pts',(30.2661006343628,-33.4734803148125,49.4073638251539));
#41780=CARTESIAN_POINT('Ctrl Pts',(32.2974192547929,-34.2559018230357,49.5184936143738));
#41781=CARTESIAN_POINT('Ctrl Pts',(34.056542998614,-32.9737464470531,49.6296234035933));
#41782=CARTESIAN_POINT('Ctrl Pts',(33.9335408923838,-30.8004288825681,49.7407531928132));
#41783=CARTESIAN_POINT('Ctrl Pts',(32.0409831298217,-29.7249457959496,49.8518829820328));
#41784=CARTESIAN_POINT('Ctrl Pts',(30.1109180512903,-30.7315676449427,49.9630127712527));
#41785=CARTESIAN_POINT('Ctrl Pts',(29.9097202859775,-32.8990450297081,50.0741425604723));
#41786=CARTESIAN_POINT('Ctrl Pts',(31.6215238467982,-34.2437261530219,50.1852723496921));
#41787=CARTESIAN_POINT('Ctrl Pts',(33.6797046786269,-33.5349734332873,50.2964021389118));
#41788=CARTESIAN_POINT('Ctrl Pts',(34.2006380042136,-31.4214296735012,50.4075319281315));
#41789=CARTESIAN_POINT('Ctrl Pts',(32.7075712932722,-29.8373872021944,50.5186617173513));
#41790=CARTESIAN_POINT('Ctrl Pts',(30.5669430080136,-30.2325445108771,50.6297915065709));
#41791=CARTESIAN_POINT('Ctrl Pts',(29.7378329409762,-32.2452579159542,50.7409212957907));
#41792=CARTESIAN_POINT('Ctrl Pts',(30.979033634155,-34.0335139360501,50.8520510850104));
#41793=CARTESIAN_POINT('Ctrl Pts',(33.1546116734798,-33.9607200544356,50.9631808742302));
#41794=CARTESIAN_POINT('Ctrl Pts',(34.2735016303912,-32.093496442081,51.0743106634498));
#41795=CARTESIAN_POINT('Ctrl Pts',(33.3117075504391,-30.1407058999481,51.1854404526696));
#41796=CARTESIAN_POINT('Ctrl Pts',(31.1494529448607,-29.8895211548044,51.2965702418893));
#41797=CARTESIAN_POINT('Ctrl Pts',(29.7656097810211,-31.5698237619369,51.4077000311091));
#41798=CARTESIAN_POINT('Ctrl Pts',(30.4266563133037,-33.6438189963982,51.5188298203287));
#41799=CARTESIAN_POINT('Ctrl Pts',(32.5276099280905,-34.2134089131759,51.6299596095486));
#41800=CARTESIAN_POINT('Ctrl Pts',(34.1457006531511,-32.7573109933717,51.7410893987682));
#41801=CARTESIAN_POINT('Ctrl Pts',(33.8000694199542,-30.6081302704023,51.852219187988));
#41802=CARTESIAN_POINT('Ctrl Pts',(31.8070341540629,-29.7327736193239,51.9633489772077));
#41803=CARTESIAN_POINT('Ctrl Pts',(29.9905991783125,-30.9323579854575,52.0744787664274));
#41804=CARTESIAN_POINT('Ctrl Pts',(30.0131459632196,-33.1090367042992,52.1856085556471));
#41805=CARTESIAN_POINT('Ctrl Pts',(31.8540401750289,-34.2707371393458,52.2967383448669));
#41806=CARTESIAN_POINT('Ctrl Pts',(33.8285149210735,-33.3542834092786,52.4078681340866));
#41807=CARTESIAN_POINT('Ctrl Pts',(34.1295532637732,-31.1984045069698,52.5189979233063));
#41808=CARTESIAN_POINT('Ctrl Pts',(32.4816463202079,-29.7761364787351,52.630127712526));
#41809=CARTESIAN_POINT('Ctrl Pts',(30.3929443290853,-30.3891254719696,52.7412575017458));
#41810=CARTESIAN_POINT('Ctrl Pts',(29.7749974270505,-32.4763669022007,52.8523872909655));
#41811=CARTESIAN_POINT('Ctrl Pts',(31.1933583183665,-34.1276473830258,52.9635170801852));
#41812=CARTESIAN_POINT('Ctrl Pts',(33.349929988658,-33.8317184046403,53.0746468694049));
#41813=CARTESIAN_POINT('Ctrl Pts',(34.2710978673113,-31.8594397050614,53.1857766586247));
#41814=CARTESIAN_POINT('Ctrl Pts',(33.1137073820875,-30.015762455313,53.2969064478444));
#41815=CARTESIAN_POINT('Ctrl Pts',(30.9372109149731,-29.9881127335314,53.4080362370641));
#41816=CARTESIAN_POINT('Ctrl Pts',(29.7330766104164,-31.8015722491152,53.5191660262839));
#41817=CARTESIAN_POINT('Ctrl Pts',(30.6041819080895,-33.7969240890906,53.6302958155036));
#41818=CARTESIAN_POINT('Ctrl Pts',(32.7515839414401,-34.1471687386821,53.7414256047233));
#41819=CARTESIAN_POINT('Ctrl Pts',(34.2134124015819,-32.5335107658101,53.852555393943));
#41820=CARTESIAN_POINT('Ctrl Pts',(33.6449476473772,-30.4291558495818,53.9636851831628));
#41821=CARTESIAN_POINT('Ctrl Pts',(32.2693872463958,-29.9891675732325,54.0377717093093));
#41822=CARTESIAN_POINT('Ctrl Pts',(31.640528121452,-30.1086918117405,54.0748149723825));
#41823=CARTESIAN_POINT('Ctrl Pts',(30.4347998857282,-30.6687801966678,40.7755550828525));
#41824=CARTESIAN_POINT('Ctrl Pts',(29.9921698977506,-31.1892085331669,40.8125983459258));
#41825=CARTESIAN_POINT('Ctrl Pts',(29.6747822472522,-32.6976038101375,40.8866848720723));
#41826=CARTESIAN_POINT('Ctrl Pts',(31.3274087025214,-34.3351197468709,40.997814661292));
#41827=CARTESIAN_POINT('Ctrl Pts',(33.5957530751518,-33.8300055395084,41.1089444505117));
#41828=CARTESIAN_POINT('Ctrl Pts',(34.40356419597,-31.6528078050466,41.2200742397314));
#41829=CARTESIAN_POINT('Ctrl Pts',(33.0117214699854,-29.7919912031069,41.3312040289512));
#41830=CARTESIAN_POINT('Ctrl Pts',(30.6939306582022,-29.9526094198962,41.4423338181709));
#41831=CARTESIAN_POINT('Ctrl Pts',(29.5714563100008,-31.9866292389199,41.5534636073906));
#41832=CARTESIAN_POINT('Ctrl Pts',(30.6715507437682,-34.0330616484485,41.6645933966103));
#41833=CARTESIAN_POINT('Ctrl Pts',(32.9874316054104,-34.2187692724043,41.7757231858301));
#41834=CARTESIAN_POINT('Ctrl Pts',(34.3996237115323,-32.3739281834235,41.8868529750498));
#41835=CARTESIAN_POINT('Ctrl Pts',(33.6157072595466,-30.1868494132083,41.9979827642695));
#41836=CARTESIAN_POINT('Ctrl Pts',(31.3531125199586,-29.6591578453596,42.1091125534892));
#41837=CARTESIAN_POINT('Ctrl Pts',(29.6825424522475,-31.2737738490384,42.220242342709));
#41838=CARTESIAN_POINT('Ctrl Pts',(30.1328842664196,-33.553027071776,42.3313721319287));
#41839=CARTESIAN_POINT('Ctrl Pts',(32.2919902196474,-34.4109652846105,42.4425019211484));
#41840=CARTESIAN_POINT('Ctrl Pts',(34.1838698561524,-33.0624149602443,42.5536317103682));
#41841=CARTESIAN_POINT('Ctrl Pts',(34.077095500667,-30.7415536091116,42.6647614995879));
#41842=CARTESIAN_POINT('Ctrl Pts',(32.0693858594061,-29.572408937857,42.7758912888076));
#41843=CARTESIAN_POINT('Ctrl Pts',(29.9981750364838,-30.6249691844573,42.8870210780273));
#41844=CARTESIAN_POINT('Ctrl Pts',(29.7590127090568,-32.9359427703937,42.9981508672471));
#41845=CARTESIAN_POINT('Ctrl Pts',(31.5707776489307,-34.3903516582226,43.1092806564667));
#41846=CARTESIAN_POINT('Ctrl Pts',(33.7753622292125,-33.6571366431167,43.2204104456866));
#41847=CARTESIAN_POINT('Ctrl Pts',(34.3551545506076,-31.4073281368721,43.3315402349062));
#41848=CARTESIAN_POINT('Ctrl Pts',(32.7795349677293,-29.699926495664,43.442670024126));
#41849=CARTESIAN_POINT('Ctrl Pts',(30.490493436163,-30.0975271807692,43.5537998133457));
#41850=CARTESIAN_POINT('Ctrl Pts',(29.5829359418664,-32.2362503593823,43.6649296025654));
#41851=CARTESIAN_POINT('Ctrl Pts',(30.887449261624,-34.1587597707098,43.7760593917852));
#41852=CARTESIAN_POINT('Ctrl Pts',(33.2101569520236,-34.1055956508643,43.8871891810049));
#41853=CARTESIAN_POINT('Ctrl Pts',(34.4253421235416,-32.1254132254779,43.9983189702246));
#41854=CARTESIAN_POINT('Ctrl Pts',(33.420880485332,-30.0304539762364,44.1094487594444));
#41855=CARTESIAN_POINT('Ctrl Pts',(31.116044435755,-29.7380018890796,44.220578548664));
#41856=CARTESIAN_POINT('Ctrl Pts',(29.6201949324755,-31.5157059427025,44.3317083378838));
#41857=CARTESIAN_POINT('Ctrl Pts',(30.3023172190834,-33.7366306656069,44.4428381271035));
#41858=CARTESIAN_POINT('Ctrl Pts',(32.538140376183,-34.3682098363267,44.5539679163233));
#41859=CARTESIAN_POINT('Ctrl Pts',(34.2814632968893,-32.8324290470048,44.6650977055429));
#41860=CARTESIAN_POINT('Ctrl Pts',(33.9368157497217,-30.5348182211821,44.7762274947627));
#41861=CARTESIAN_POINT('Ctrl Pts',(31.819615432301,-29.5781258700983,44.8873572839824));
#41862=CARTESIAN_POINT('Ctrl Pts',(29.8675011150493,-30.8379064585695,44.9984870732022));
#41863=CARTESIAN_POINT('Ctrl Pts',(29.867026651317,-33.1612224537781,45.1096168624218));
#41864=CARTESIAN_POINT('Ctrl Pts',(31.8186262651666,-34.4218002522221,45.2207466516416));
#41865=CARTESIAN_POINT('Ctrl Pts',(33.9362171542195,-33.4659727231625,45.3318764408613));
#41866=CARTESIAN_POINT('Ctrl Pts',(34.2818031011314,-31.1685028556768,45.443006230081));
#41867=CARTESIAN_POINT('Ctrl Pts',(32.539107595012,-29.6320101574646,45.5541360193008));
#41868=CARTESIAN_POINT('Ctrl Pts',(30.3030266643161,-30.2626760833603,45.6652658085204));
#41869=CARTESIAN_POINT('Ctrl Pts',(29.6199973275285,-32.4833220172713,45.7763955977403));
#41870=CARTESIAN_POINT('Ctrl Pts',(31.1151206265327,-34.2616368823846,45.88752538696));
#41871=CARTESIAN_POINT('Ctrl Pts',(33.4200759320169,-33.9701261991703,45.9986551761797));
#41872=CARTESIAN_POINT('Ctrl Pts',(34.4253931446014,-31.8755773836041,46.1097849653994));
#41873=CARTESIAN_POINT('Ctrl Pts',(33.2110168535402,-29.8948987972565,46.2209147546191));
#41874=CARTESIAN_POINT('Ctrl Pts',(30.8883310710498,-29.8407860027877,46.3320445438389));
#41875=CARTESIAN_POINT('Ctrl Pts',(29.5830326367871,-31.7627624428669,46.4431743330586));
#41876=CARTESIAN_POINT('Ctrl Pts',(30.4897165224173,-33.9018561225001,46.5543041222784));
#41877=CARTESIAN_POINT('Ctrl Pts',(32.7785954683888,-34.300391703592,46.665433911498));
#41878=CARTESIAN_POINT('Ctrl Pts',(34.3549122852071,-32.5936337442658,46.7765637007178));
#41879=CARTESIAN_POINT('Ctrl Pts',(33.7760389165643,-30.3435886198774,46.8876934899375));
#41880=CARTESIAN_POINT('Ctrl Pts',(31.5717539918218,-29.6094732275437,46.9988232791572));
#41881=CARTESIAN_POINT('Ctrl Pts',(29.7593951696295,-31.0631420131788,47.1099530683769));
#41882=CARTESIAN_POINT('Ctrl Pts',(29.9976135898446,-33.3742130685507,47.2210828575967));
#41883=CARTESIAN_POINT('Ctrl Pts',(32.0683943376577,-34.4276192263053,47.3322126468163));
#41884=CARTESIAN_POINT('Ctrl Pts',(34.0765813293521,-33.2592945945794,47.4433424360362));
#41885=CARTESIAN_POINT('Ctrl Pts',(34.1843036080103,-30.9384772063757,47.5544722252558));
#41886=CARTESIAN_POINT('Ctrl Pts',(32.2929749124037,-29.5891539671616,47.6656020144756));
#41887=CARTESIAN_POINT('Ctrl Pts',(30.1335187541459,-30.4462108726646,47.7767318036953));
#41888=CARTESIAN_POINT('Ctrl Pts',(29.6822459909475,-32.7252787373636,47.8878615929151));
#41889=CARTESIAN_POINT('Ctrl Pts',(31.3521565618384,-34.3405793669477,47.9989913821348));
#41890=CARTESIAN_POINT('Ctrl Pts',(33.6149664217652,-33.8138071424277,48.1101211713545));
#41891=CARTESIAN_POINT('Ctrl Pts',(34.3997765260741,-31.6270582910771,48.2212509605742));
#41892=CARTESIAN_POINT('Ctrl Pts',(32.9883371782127,-29.7816216473485,48.3323807497939));
#41893=CARTESIAN_POINT('Ctrl Pts',(30.6723823629214,-29.966420814655,48.4435105390137));
#41894=CARTESIAN_POINT('Ctrl Pts',(29.5714488116707,-32.0123295991414,48.5546403282333));
#41895=CARTESIAN_POINT('Ctrl Pts',(30.693098971438,-34.0469544682025,48.6657701174531));
#41896=CARTESIAN_POINT('Ctrl Pts',(33.0108107797937,-34.2082288062616,48.7768999066728));
#41897=CARTESIAN_POINT('Ctrl Pts',(34.4034395242687,-32.3485560880743,48.8880296958926));
#41898=CARTESIAN_POINT('Ctrl Pts',(33.5964664803493,-30.1698886180148,48.9991594851123));
#41899=CARTESIAN_POINT('Ctrl Pts',(31.3284246265722,-29.6661192380166,49.1102892743321));
#41900=CARTESIAN_POINT('Ctrl Pts',(29.6750012716246,-31.2982922215028,49.2214190635517));
#41901=CARTESIAN_POINT('Ctrl Pts',(30.1493915393249,-33.5726605541655,49.3325488527715));
#41902=CARTESIAN_POINT('Ctrl Pts',(32.317438601222,-34.4077470024496,49.4436786419912));
#41903=CARTESIAN_POINT('Ctrl Pts',(34.1949692977589,-33.0392895050207,49.5548084312109));
#41904=CARTESIAN_POINT('Ctrl Pts',(34.0636878964378,-30.7196855232223,49.6659382204306));
#41905=CARTESIAN_POINT('Ctrl Pts',(32.0437417120601,-29.5718114661385,49.7770680096504));
#41906=CARTESIAN_POINT('Ctrl Pts',(29.9837635871641,-30.6461892226366,49.8881977988701));
#41907=CARTESIAN_POINT('Ctrl Pts',(29.7690231621222,-32.9595599211113,49.9993275880899));
#41908=CARTESIAN_POINT('Ctrl Pts',(31.5960485451694,-34.3947517857787,50.1104573773095));
#41909=CARTESIAN_POINT('Ctrl Pts',(33.7927659190072,-33.6382927861036,50.2215871665294));
#41910=CARTESIAN_POINT('Ctrl Pts',(34.3487633655049,-31.3824859951311,50.332716955749));
#41911=CARTESIAN_POINT('Ctrl Pts',(32.7551980511737,-29.6918213247557,50.4438467449688));
#41912=CARTESIAN_POINT('Ctrl Pts',(30.470483670184,-30.1135767468053,50.5549765341884));
#41913=CARTESIAN_POINT('Ctrl Pts',(29.5855660473401,-32.2617662727765,50.6661063234083));
#41914=CARTESIAN_POINT('Ctrl Pts',(30.9103121945009,-34.1703901446276,50.7772361126279));
#41915=CARTESIAN_POINT('Ctrl Pts',(33.2323288041292,-34.0926964930404,50.8883659018477));
#41916=CARTESIAN_POINT('Ctrl Pts',(34.426531456175,-32.0997897053238,50.9994956910673));
#41917=CARTESIAN_POINT('Ctrl Pts',(33.399998834351,-30.0155564615627,51.1106254802872));
#41918=CARTESIAN_POINT('Ctrl Pts',(31.0922024613207,-29.7474644236002,51.2217552695068));
#41919=CARTESIAN_POINT('Ctrl Pts',(29.6152125517546,-31.5408685177941,51.3328850587265));
#41920=CARTESIAN_POINT('Ctrl Pts',(30.3207542514557,-33.7544647647039,51.4440148479463));
#41921=CARTESIAN_POINT('Ctrl Pts',(32.563123452382,-34.3623938867708,51.555144637166));
#41922=CARTESIAN_POINT('Ctrl Pts',(34.2901281709266,-32.8082857399171,51.6662744263857));
#41923=CARTESIAN_POINT('Ctrl Pts',(33.9212324338936,-30.5144432550129,51.7774042156054));
#41924=CARTESIAN_POINT('Ctrl Pts',(31.7940455863876,-29.5801661817881,51.8885340048252));
#41925=CARTESIAN_POINT('Ctrl Pts',(29.8553460280345,-30.8604947990401,51.9996637940449));
#41926=CARTESIAN_POINT('Ctrl Pts',(29.8794104413083,-33.1836861751323,52.1107935832647));
#41927=CARTESIAN_POINT('Ctrl Pts',(31.844215591537,-34.4235808867133,52.2219233724843));
#41928=CARTESIAN_POINT('Ctrl Pts',(33.9515926070864,-33.4454404823211,52.3330531617041));
#41929=CARTESIAN_POINT('Ctrl Pts',(34.2728938977083,-31.1444489623563,52.4441829509238));
#41930=CARTESIAN_POINT('Ctrl Pts',(32.5140660253384,-29.6264478034877,52.5553127401435));
#41931=CARTESIAN_POINT('Ctrl Pts',(30.284773107188,-30.2806972020757,52.6664425293633));
#41932=CARTESIAN_POINT('Ctrl Pts',(29.6252320820182,-32.5084312487041,52.777572318583));
#41933=CARTESIAN_POINT('Ctrl Pts',(31.1390631138414,-34.2708597317664,52.8887021078028));
#41934=CARTESIAN_POINT('Ctrl Pts',(33.4407940321331,-33.9550117177394,52.9998318970224));
#41935=CARTESIAN_POINT('Ctrl Pts',(34.4239658953466,-31.8499785649598,53.1109616862422));
#41936=CARTESIAN_POINT('Ctrl Pts',(33.188671237128,-29.8822030499806,53.2220914754619));
#41937=CARTESIAN_POINT('Ctrl Pts',(30.8656743801615,-29.8526922201837,53.3332212646816));
#41938=CARTESIAN_POINT('Ctrl Pts',(29.5804895672685,-31.7882160395824,53.4443510539014));
#41939=CARTESIAN_POINT('Ctrl Pts',(30.5102291276843,-33.9178753902133,53.5554808431211));
#41940=CARTESIAN_POINT('Ctrl Pts',(32.8021731990342,-34.291695073573,53.6666106323408));
#41941=CARTESIAN_POINT('Ctrl Pts',(34.362397609982,-32.5694214766073,53.7777404215605));
#41942=CARTESIAN_POINT('Ctrl Pts',(33.7556693853943,-30.3234220319946,53.8888702107803));
#41943=CARTESIAN_POINT('Ctrl Pts',(32.2875197530249,-29.8538180613451,53.9629567369268));
#41944=CARTESIAN_POINT('Ctrl Pts',(31.6163320011532,-29.9813874990081,54.));
#41945=CARTESIAN_POINT('Ctrl Pts',(30.7309291201476,-30.9206413469515,41.));
#41946=CARTESIAN_POINT('Ctrl Pts',(30.6855978806243,-30.9629305822782,41.));
#41947=CARTESIAN_POINT('Ctrl Pts',(30.6429965177354,-31.0077887820157,41.));
#41948=CARTESIAN_POINT('Ctrl Pts',(30.6031236390744,-31.0548709612839,41.));
#41949=CARTESIAN_POINT('Ctrl Pts',(30.5606226453807,-31.1050564375116,41.));
#41950=CARTESIAN_POINT('Ctrl Pts',(30.5212209469281,-31.1577689646829,41.));
#41951=CARTESIAN_POINT('Ctrl Pts',(30.4849456787917,-31.2126454473402,41.));
#41952=CARTESIAN_POINT('Ctrl Pts',(30.4532048191724,-31.2606623696652,41.));
#41953=CARTESIAN_POINT('Ctrl Pts',(30.4238578759431,-31.3103372955829,41.));
#41954=CARTESIAN_POINT('Ctrl Pts',(30.3969459135927,-31.3614545259121,41.));
#41955=CARTESIAN_POINT('Ctrl Pts',(30.383446347189,-31.3870959279109,41.));
#41956=CARTESIAN_POINT('Ctrl Pts',(30.3705598364866,-31.4131006012838,41.));
#41957=CARTESIAN_POINT('Ctrl Pts',(30.3582939048221,-31.4394431609949,41.));
#41958=CARTESIAN_POINT('Ctrl Pts',(30.3526827339958,-31.451493823479,41.));
#41959=CARTESIAN_POINT('Ctrl Pts',(30.3472008500408,-31.4636168867931,41.));
#41960=CARTESIAN_POINT('Ctrl Pts',(30.3418574940955,-31.4757899451731,41.));
#41961=CARTESIAN_POINT('Ctrl Pts',(30.3149359070818,-31.537121822321,41.));
#41962=CARTESIAN_POINT('Ctrl Pts',(30.2914755974925,-31.5998291482412,41.));
#41963=CARTESIAN_POINT('Ctrl Pts',(30.2715001667511,-31.6635542174867,41.));
#41964=CARTESIAN_POINT('Ctrl Pts',(30.2511707190549,-31.7284086618758,41.));
#41965=CARTESIAN_POINT('Ctrl Pts',(30.2344502095525,-31.7943180848097,41.));
#41966=CARTESIAN_POINT('Ctrl Pts',(30.2214028317259,-31.8609419339526,41.));
#41967=CARTESIAN_POINT('Ctrl Pts',(30.2104912353279,-31.9166598384991,41.));
#41968=CARTESIAN_POINT('Ctrl Pts',(30.2021492089366,-31.972878358886,41.));
#41969=CARTESIAN_POINT('Ctrl Pts',(30.1964391172512,-32.0294105816203,41.));
#41970=CARTESIAN_POINT('Ctrl Pts',(30.1938093347234,-32.055446494841,41.));
#41971=CARTESIAN_POINT('Ctrl Pts',(30.1917381369785,-32.0815490593274,41.));
#41972=CARTESIAN_POINT('Ctrl Pts',(30.1902334165381,-32.1077004172633,41.));
#41973=CARTESIAN_POINT('Ctrl Pts',(30.1895753812609,-32.1191367715564,41.));
#41974=CARTESIAN_POINT('Ctrl Pts',(30.1890257975943,-32.1305822670034,41.));
#41975=CARTESIAN_POINT('Ctrl Pts',(30.1885856619553,-32.1420212484968,41.));
#41976=CARTESIAN_POINT('Ctrl Pts',(30.1858874976538,-32.2121456573693,41.));
#41977=CARTESIAN_POINT('Ctrl Pts',(30.1872903022448,-32.2821566391967,41.));
#41978=CARTESIAN_POINT('Ctrl Pts',(30.1928488011416,-32.3516934917122,41.));
#41979=CARTESIAN_POINT('Ctrl Pts',(30.1978161829043,-32.4138354655506,41.));
#41980=CARTESIAN_POINT('Ctrl Pts',(30.2061027353294,-32.4755997535043,41.));
#41981=CARTESIAN_POINT('Ctrl Pts',(30.217780599423,-32.5367410473977,41.));
#41982=CARTESIAN_POINT('Ctrl Pts',(30.230508640649,-32.6033807088163,41.));
#41983=CARTESIAN_POINT('Ctrl Pts',(30.2472642836697,-32.6692811201171,41.));
#41984=CARTESIAN_POINT('Ctrl Pts',(30.267802240865,-32.7342286370083,41.));
#41985=CARTESIAN_POINT('Ctrl Pts',(30.2757344649613,-32.7593128385954,41.));
#41986=CARTESIAN_POINT('Ctrl Pts',(30.2842314436902,-32.7842548517836,41.));
#41987=CARTESIAN_POINT('Ctrl Pts',(30.2932810585363,-32.8090420474308,41.));
#41988=CARTESIAN_POINT('Ctrl Pts',(30.2972495255297,-32.8199118103387,41.));
#41989=CARTESIAN_POINT('Ctrl Pts',(30.3013241696228,-32.8307512478403,41.));
#41990=CARTESIAN_POINT('Ctrl Pts',(30.3054988752419,-32.8415467359126,41.));
#41991=CARTESIAN_POINT('Ctrl Pts',(30.3307215131888,-32.9067706611294,41.));
#41992=CARTESIAN_POINT('Ctrl Pts',(30.3596350679945,-32.9705095691753,41.));
#41993=CARTESIAN_POINT('Ctrl Pts',(30.3919268344823,-33.0325445786466,41.));
#41994=CARTESIAN_POINT('Ctrl Pts',(30.4249669781864,-33.0960172792927,41.));
#41995=CARTESIAN_POINT('Ctrl Pts',(30.461544033557,-33.1577070082778,41.));
#41996=CARTESIAN_POINT('Ctrl Pts',(30.5013791864624,-33.2173756043833,41.));
#41997=CARTESIAN_POINT('Ctrl Pts',(30.5318851553063,-33.2630701279634,41.));
#41998=CARTESIAN_POINT('Ctrl Pts',(30.5643030759919,-33.3075793757001,41.));
#41999=CARTESIAN_POINT('Ctrl Pts',(30.5985273064738,-33.3507902757675,41.));
#42000=CARTESIAN_POINT('Ctrl Pts',(30.6198359272625,-33.3776941584995,41.));
#42001=CARTESIAN_POINT('Ctrl Pts',(30.6418450939684,-33.4040946096701,41.));
#42002=CARTESIAN_POINT('Ctrl Pts',(30.6645322221831,-33.4299626453368,41.));
#42003=CARTESIAN_POINT('Ctrl Pts',(30.6771875615082,-33.444392359223,41.));
#42004=CARTESIAN_POINT('Ctrl Pts',(30.6900582984156,-33.4586609103331,41.));
#42005=CARTESIAN_POINT('Ctrl Pts',(30.7031169141315,-33.4727379551488,41.));
#42006=CARTESIAN_POINT('Ctrl Pts',(30.7539897162477,-33.527578279029,41.));
#42007=CARTESIAN_POINT('Ctrl Pts',(30.8077590845298,-33.5795736788928,41.));
#42008=CARTESIAN_POINT('Ctrl Pts',(30.8641400026091,-33.6284601407826,41.));
#42009=CARTESIAN_POINT('Ctrl Pts',(30.9062939577409,-33.665010764491,41.));
#42010=CARTESIAN_POINT('Ctrl Pts',(30.9499089277002,-33.6998232910283,41.));
#42011=CARTESIAN_POINT('Ctrl Pts',(30.9948821713292,-33.732777639113,41.));
#42012=CARTESIAN_POINT('Ctrl Pts',(31.008966379297,-33.74309790633,41.));
#42013=CARTESIAN_POINT('Ctrl Pts',(31.0231838921667,-33.7532358564134,41.));
#42014=CARTESIAN_POINT('Ctrl Pts',(31.0375317968707,-33.7631875733228,41.));
#42015=CARTESIAN_POINT('Ctrl Pts',(31.0513138213297,-33.7727467952917,41.));
#42016=CARTESIAN_POINT('Ctrl Pts',(31.0652090990272,-33.782129227744,41.));
#42017=CARTESIAN_POINT('Ctrl Pts',(31.0792097130569,-33.791328684408,41.));
#42018=CARTESIAN_POINT('Ctrl Pts',(31.1421653737961,-33.8326952895796,41.));
#42019=CARTESIAN_POINT('Ctrl Pts',(31.2072783450083,-33.8703859700674,41.));
#42020=CARTESIAN_POINT('Ctrl Pts',(31.2742872744703,-33.9041214598101,41.));
#42021=CARTESIAN_POINT('Ctrl Pts',(31.3254777357978,-33.9298931785482,41.));
#42022=CARTESIAN_POINT('Ctrl Pts',(31.3777756457353,-33.9533562526433,41.));
#42023=CARTESIAN_POINT('Ctrl Pts',(31.4310783175737,-33.9743709615764,41.));
#42024=CARTESIAN_POINT('Ctrl Pts',(31.4435634323603,-33.9792932486624,41.));
#42025=CARTESIAN_POINT('Ctrl Pts',(31.4561037167888,-33.9840811412651,41.));
#42026=CARTESIAN_POINT('Ctrl Pts',(31.4686972148566,-33.9887352337365,41.));
#42027=CARTESIAN_POINT('Ctrl Pts',(33.6673070425528,-32.0013037875835,42.1285196366098));
#42028=CARTESIAN_POINT('Ctrl Pts',(33.6680432508362,-32.0869536148502,42.1227790551389));
#42029=CARTESIAN_POINT('Ctrl Pts',(33.6620131902561,-32.1724994405965,42.1170384736681));
#42030=CARTESIAN_POINT('Ctrl Pts',(33.6488560459642,-32.2569345941976,42.1112978921973));
#42031=CARTESIAN_POINT('Ctrl Pts',(33.5639546192058,-32.8017842097567,42.074254629124));
#42032=CARTESIAN_POINT('Ctrl Pts',(33.1822841728743,-33.3003858651474,42.0372113660508));
#42033=CARTESIAN_POINT('Ctrl Pts',(32.6784946149966,-33.5245912715416,42.0001681029776));
#42034=CARTESIAN_POINT('Ctrl Pts',(32.1747050571189,-33.7487966779359,41.9631248399043));
#42035=CARTESIAN_POINT('Ctrl Pts',(31.5487963876951,-33.6986058353337,41.9260815768311));
#42036=CARTESIAN_POINT('Ctrl Pts',(31.0871818488499,-33.3969677369612,41.8890383137578));
#42037=CARTESIAN_POINT('Ctrl Pts',(30.6255673100048,-33.0953296385888,41.8519950506846));
#42038=CARTESIAN_POINT('Ctrl Pts',(30.3282469017383,-32.542244284446,41.8149517876113));
#42039=CARTESIAN_POINT('Ctrl Pts',(30.3312711899686,-31.9908362937928,41.7779085245381));
#42040=CARTESIAN_POINT('Ctrl Pts',(30.3342954781989,-31.4394283031396,41.7408652614648));
#42041=CARTESIAN_POINT('Ctrl Pts',(30.6376644629259,-30.889697675976,41.7038219983916));
#42042=CARTESIAN_POINT('Ctrl Pts',(31.1025613892782,-30.59312737402,41.6667787353184));
#42043=CARTESIAN_POINT('Ctrl Pts',(31.5674583156305,-30.296557072064,41.6297354722451));
#42044=CARTESIAN_POINT('Ctrl Pts',(32.1938831836081,-30.2531470953156,41.5926922091719));
#42045=CARTESIAN_POINT('Ctrl Pts',(32.6951809468332,-30.4829017702283,41.5556489460986));
#42046=CARTESIAN_POINT('Ctrl Pts',(33.1964787100584,-30.7126564451409,41.5186056830254));
#42047=CARTESIAN_POINT('Ctrl Pts',(33.5726493685311,-31.2155757717146,41.4815624199521));
#42048=CARTESIAN_POINT('Ctrl Pts',(33.6515719182498,-31.7612489585941,41.4445191568789));
#42049=CARTESIAN_POINT('Ctrl Pts',(33.6629345145688,-31.839810335117,41.4391859834559));
#42050=CARTESIAN_POINT('Ctrl Pts',(33.6681358153543,-31.9192579045568,41.4338528100328));
#42051=CARTESIAN_POINT('Ctrl Pts',(33.6674738845699,-31.9987897819954,41.4285196366098));
#42052=CARTESIAN_POINT('Ctrl Pts',(32.5301702171886,-33.9851743256717,41.));
#42053=CARTESIAN_POINT('Ctrl Pts',(33.1902397907527,-33.8088929660699,41.0370432630732));
#42054=CARTESIAN_POINT('Ctrl Pts',(34.309243415742,-32.7487884047516,41.1111297892197));
#42055=CARTESIAN_POINT('Ctrl Pts',(33.8813839462517,-30.4619629566307,41.2222595784394));
#42056=CARTESIAN_POINT('Ctrl Pts',(31.7284038562778,-29.5872042670172,41.3333893676592));
#42057=CARTESIAN_POINT('Ctrl Pts',(29.825627898444,-30.918441305227,41.4445191568789));
#42058=CARTESIAN_POINT('Ctrl Pts',(29.9119860544063,-33.2405970018638,41.5556489460987));
#42059=CARTESIAN_POINT('Ctrl Pts',(31.9096898625478,-34.4268228681169,41.6667787353183));
#42060=CARTESIAN_POINT('Ctrl Pts',(33.9898334202982,-33.3923239957753,41.7779085245381));
#42061=CARTESIAN_POINT('Ctrl Pts',(34.2490096530018,-31.0834452595862,41.8890383137578));
#42062=CARTESIAN_POINT('Ctrl Pts',(32.4498627695247,-29.6134582253175,42.0001681029775));
#42063=CARTESIAN_POINT('Ctrl Pts',(30.2390335714705,-30.327572605785,42.1112978921973));
#42064=CARTESIAN_POINT('Ctrl Pts',(29.6398080047623,-32.5722924533201,42.222427681417));
#42065=CARTESIAN_POINT('Ctrl Pts',(31.200611501379,-34.2932473343971,42.3335574706367));
#42066=CARTESIAN_POINT('Ctrl Pts',(33.4930031748503,-33.9154517310286,42.4446872598565));
#42067=CARTESIAN_POINT('Ctrl Pts',(34.4190163057797,-31.7846531484843,42.5558170490762));
#42068=CARTESIAN_POINT('Ctrl Pts',(33.1311710515888,-29.8509388446871,42.6669468382959));
#42069=CARTESIAN_POINT('Ctrl Pts',(30.8080907702464,-29.8840214107802,42.7780766275156));
#42070=CARTESIAN_POINT('Ctrl Pts',(29.5758326618125,-31.8536249348858,42.8892064167354));
#42071=CARTESIAN_POINT('Ctrl Pts',(30.5621463276885,-33.9571891796694,43.0003362059551));
#42072=CARTESIAN_POINT('Ctrl Pts',(32.8643680232945,-34.2695551886057,43.1114659951748));
#42073=CARTESIAN_POINT('Ctrl Pts',(34.3755295071108,-32.5048488625596,43.2225957843945));
#42074=CARTESIAN_POINT('Ctrl Pts',(33.7126321326879,-30.2781103518923,43.3337255736142));
#42075=CARTESIAN_POINT('Ctrl Pts',(31.4823524106659,-29.6272265641889,43.444855362834));
#42076=CARTESIAN_POINT('Ctrl Pts',(29.725818144952,-31.1478792982686,43.5559851520537));
#42077=CARTESIAN_POINT('Ctrl Pts',(30.0505904524204,-33.4483836551904,43.6671149412735));
#42078=CARTESIAN_POINT('Ctrl Pts',(32.1594412363987,-34.4233429992207,43.7782447304931));
#42079=CARTESIAN_POINT('Ctrl Pts',(34.1223731303825,-33.1804851097821,43.8893745197129));
#42080=CARTESIAN_POINT('Ctrl Pts',(34.1429321513712,-30.8572600500235,44.0005043089326));
#42081=CARTESIAN_POINT('Ctrl Pts',(32.2023029066813,-29.5798581998207,44.1116340981523));
#42082=CARTESIAN_POINT('Ctrl Pts',(30.0765282356173,-30.5173438798798,44.2227638873721));
#42083=CARTESIAN_POINT('Ctrl Pts',(29.7110940641655,-32.8117403622951,44.3338936765918));
#42084=CARTESIAN_POINT('Ctrl Pts',(31.4404417830221,-34.3632408681166,44.4450234658115));
#42085=CARTESIAN_POINT('Ctrl Pts',(33.6818911139087,-33.7519289597072,44.5561532550313));
#42086=CARTESIAN_POINT('Ctrl Pts',(34.3840919366917,-31.5372706662576,44.667283044251));
#42087=CARTESIAN_POINT('Ctrl Pts',(32.9043976734169,-29.7460972409556,44.7784128334707));
#42088=CARTESIAN_POINT('Ctrl Pts',(30.5970084672143,-30.0176711781749,44.8895426226904));
#42089=CARTESIAN_POINT('Ctrl Pts',(29.573621897008,-32.1034509556668,45.0006724119102));
#42090=CARTESIAN_POINT('Ctrl Pts',(30.770830253685,-34.0945535404118,45.1118022011299));
#42091=CARTESIAN_POINT('Ctrl Pts',(33.0929614323987,-34.168743439459,45.2229319903496));
#42092=CARTESIAN_POINT('Ctrl Pts',(34.4148261608542,-32.2581228617566,45.3340617795694));
#42093=CARTESIAN_POINT('Ctrl Pts',(33.5266681745953,-30.1112710402004,45.445191568789));
#42094=CARTESIAN_POINT('Ctrl Pts',(31.2413200309736,-29.6929634802401,45.5563213580089));
#42095=CARTESIAN_POINT('Ctrl Pts',(29.6503075674633,-31.3860307243948,45.6674511472285));
#42096=CARTESIAN_POINT('Ctrl Pts',(30.2097081368571,-33.6409959913638,45.7785809364483));
#42097=CARTESIAN_POINT('Ctrl Pts',(32.4075644044926,-34.3941395228971,45.8897107256679));
#42098=CARTESIAN_POINT('Ctrl Pts',(34.2324221489883,-32.956192526437,46.0008405148877));
#42099=CARTESIAN_POINT('Ctrl Pts',(34.01419135234,-30.6431484992579,46.1119703041074));
#42100=CARTESIAN_POINT('Ctrl Pts',(31.9525944730258,-29.5718802511161,46.2231000933272));
#42101=CARTESIAN_POINT('Ctrl Pts',(29.9343826179068,-30.7228008652907,46.3342298825469));
#42102=CARTESIAN_POINT('Ctrl Pts',(29.8066013901918,-33.0426002769034,46.4453596717666));
#42103=CARTESIAN_POINT('Ctrl Pts',(31.6861947837558,-34.4082232216233,46.5564894609863));
#42104=CARTESIAN_POINT('Ctrl Pts',(33.8529793081506,-33.5698663900069,46.6676192502061));
#42105=CARTESIAN_POINT('Ctrl Pts',(34.3239372644498,-31.2947848627483,46.7787490394257));
#42106=CARTESIAN_POINT('Ctrl Pts',(32.6680530383748,-29.6651085813628,46.8898788286456));
#42107=CARTESIAN_POINT('Ctrl Pts',(30.4007739163126,-30.172299605471,47.0010086178652));
#42108=CARTESIAN_POINT('Ctrl Pts',(29.5970891631565,-32.3521822100667,47.112138407085));
#42109=CARTESIAN_POINT('Ctrl Pts',(30.9925223493965,-34.2097514752664,47.2232681963047));
#42110=CARTESIAN_POINT('Ctrl Pts',(33.3099881558288,-34.0449801540592,47.3343979855244));
#42111=CARTESIAN_POINT('Ctrl Pts',(34.4285670082764,-32.0086651727433,47.4455277747442));
#42112=CARTESIAN_POINT('Ctrl Pts',(33.324547671462,-29.9644199193026,47.5566575639638));
#42113=CARTESIAN_POINT('Ctrl Pts',(31.008316669847,-29.7831154807695,47.6677873531836));
#42114=CARTESIAN_POINT('Ctrl Pts',(29.59966349763,-31.6306797131245,47.7789171424033));
#42115=CARTESIAN_POINT('Ctrl Pts',(30.3877722618167,-33.8162418669164,47.8900469316231));
#42116=CARTESIAN_POINT('Ctrl Pts',(32.6513743681069,-34.3395991604291,48.0011767208428));
#42117=CARTESIAN_POINT('Ctrl Pts',(34.3188457165666,-32.7217806742136,48.1123065100625));
#42118=CARTESIAN_POINT('Ctrl Pts',(33.8641346120592,-30.4433963423432,48.2234362992822));
#42119=CARTESIAN_POINT('Ctrl Pts',(31.7033877262933,-29.5895987972966,48.334566088502));
#42120=CARTESIAN_POINT('Ctrl Pts',(29.8140971767976,-30.9417742932515,48.4456958777216));
#42121=CARTESIAN_POINT('Ctrl Pts',(29.9253211859677,-33.2624264800428,48.5568256669414));
#42122=CARTESIAN_POINT('Ctrl Pts',(31.9352687467854,-34.427719642744,48.6679554561611));
#42123=CARTESIAN_POINT('Ctrl Pts',(34.0044576485638,-33.3711901159291,48.7790852453809));
#42124=CARTESIAN_POINT('Ctrl Pts',(34.2391886478147,-31.0597622649535,48.8902150346006));
#42125=CARTESIAN_POINT('Ctrl Pts',(32.4246384795753,-29.6088297926389,49.0013448238203));
#42126=CARTESIAN_POINT('Ctrl Pts',(30.2214637798412,-30.34627036294,49.1124746130401));
#42127=CARTESIAN_POINT('Ctrl Pts',(29.6459861413742,-32.5971863631273,49.2236044022597));
#42128=CARTESIAN_POINT('Ctrl Pts',(31.2248764581043,-34.3015638799969,49.3347341914795));
#42129=CARTESIAN_POINT('Ctrl Pts',(33.5131514345126,-33.8995750933143,49.4458639806993));
#42130=CARTESIAN_POINT('Ctrl Pts',(34.4166066274989,-31.7591157812645,49.5569937699189));
#42131=CARTESIAN_POINT('Ctrl Pts',(33.1084096420059,-29.8391110939209,49.6681235591387));
#42132=CARTESIAN_POINT('Ctrl Pts',(30.785808172351,-29.8967284995564,49.7792533483584));
#42133=CARTESIAN_POINT('Ctrl Pts',(29.5744218959985,-31.8792371733684,49.8903831375781));
#42134=CARTESIAN_POINT('Ctrl Pts',(30.5828983961289,-33.9722666764952,50.0015129267979));
#42135=CARTESIAN_POINT('Ctrl Pts',(32.8882909162952,-34.2602991056352,50.1126427160176));
#42136=CARTESIAN_POINT('Ctrl Pts',(34.3807292229819,-32.4797303052207,50.2237725052373));
#42137=CARTESIAN_POINT('Ctrl Pts',(33.6943499627291,-30.2601175319272,50.334902294457));
#42138=CARTESIAN_POINT('Ctrl Pts',(31.4573199910465,-29.6328263251734,50.4460320836768));
#42139=CARTESIAN_POINT('Ctrl Pts',(29.7169448784392,-31.1719467946929,50.5571618728964));
#42140=CARTESIAN_POINT('Ctrl Pts',(30.0659970543811,-33.4688925778434,50.6682916621163));
#42141=CARTESIAN_POINT('Ctrl Pts',(32.1850277527679,-34.4215238032342,50.7794214513359));
#42142=CARTESIAN_POINT('Ctrl Pts',(34.1347230583577,-33.1580027042254,50.8905512405557));
#42143=CARTESIAN_POINT('Ctrl Pts',(34.1307429710586,-30.8346900883493,51.0016810297754));
#42144=CARTESIAN_POINT('Ctrl Pts',(32.1767300235671,-29.5778564663098,51.1128108189952));
#42145=CARTESIAN_POINT('Ctrl Pts',(30.0609756751137,-30.5377423393424,51.2239406082148));
#42146=CARTESIAN_POINT('Ctrl Pts',(29.7197953608552,-32.8358705657033,51.3350703974346));
#42147=CARTESIAN_POINT('Ctrl Pts',(31.465433604746,-34.3690191153306,51.4462001866543));
#42148=CARTESIAN_POINT('Ctrl Pts',(33.7003012160588,-33.7340670608388,51.5573299758741));
#42149=CARTESIAN_POINT('Ctrl Pts',(34.3790715941924,-31.5121156388489,51.6684597650937));
#42150=CARTESIAN_POINT('Ctrl Pts',(32.8805414477757,-29.736670690513,51.7795895543136));
#42151=CARTESIAN_POINT('Ctrl Pts',(30.5761493204034,-30.0326001869503,51.8907193435332));
#42152=CARTESIAN_POINT('Ctrl Pts',(29.5748498880924,-32.1290726458106,52.001849132753));
#42153=CARTESIAN_POINT('Ctrl Pts',(30.7930215501968,-34.1074192405717,52.1129789219727));
#42154=CARTESIAN_POINT('Ctrl Pts',(33.1158067773521,-34.1570785575888,52.2241087111924));
#42155=CARTESIAN_POINT('Ctrl Pts',(34.4174177879696,-32.2326030559352,52.3352385004122));
#42156=CARTESIAN_POINT('Ctrl Pts',(33.506634164426,-30.0952515923113,52.4463682896318));
#42157=CARTESIAN_POINT('Ctrl Pts',(31.2169954713513,-29.7011055471504,52.5574980788516));
#42158=CARTESIAN_POINT('Ctrl Pts',(29.6439536772523,-31.4108821177788,52.6686278680713));
#42159=CARTESIAN_POINT('Ctrl Pts',(30.2271406288629,-33.6598142860527,52.779757657291));
#42160=CARTESIAN_POINT('Ctrl Pts',(32.432827862626,-34.3896998451232,52.8908874465108));
#42161=CARTESIAN_POINT('Ctrl Pts',(34.2423984788832,-32.9325631176565,53.0020172357305));
#42162=CARTESIAN_POINT('Ctrl Pts',(33.9997448841109,-30.6219446492246,53.1131470249503));
#42163=CARTESIAN_POINT('Ctrl Pts',(31.9269572285084,-29.572527465193,53.2242768141699));
#42164=CARTESIAN_POINT('Ctrl Pts',(29.9209962036954,-30.7446672845728,53.3354066033898));
#42165=CARTESIAN_POINT('Ctrl Pts',(29.8177591150446,-33.0657522553465,53.4465363926093));
#42166=CARTESIAN_POINT('Ctrl Pts',(31.7116016656226,-34.4113173899075,53.5576661818292));
#42167=CARTESIAN_POINT('Ctrl Pts',(33.8695486450878,-33.5503777029091,53.6687959710488));
#42168=CARTESIAN_POINT('Ctrl Pts',(34.3161775453905,-31.269941903344,53.7799257602686));
#42169=CARTESIAN_POINT('Ctrl Pts',(32.6437141768078,-29.658850758076,53.8910555494883));
#42170=CARTESIAN_POINT('Ctrl Pts',(30.3808457446301,-30.1879561271019,54.002185338708));
#42171=CARTESIAN_POINT('Ctrl Pts',(29.6023721664291,-32.3803550971457,54.1133151279277));
#42172=CARTESIAN_POINT('Ctrl Pts',(30.5427968191103,-33.6016627022545,54.1874016540742));
#42173=CARTESIAN_POINT('Ctrl Pts',(31.1673980508611,-33.878502477185,54.2244449171475));
#42174=CARTESIAN_POINT('Ctrl Pts',(32.4967348970877,-33.8599788000028,40.9251850276175));
#42175=CARTESIAN_POINT('Ctrl Pts',(33.1151770144774,-33.6948146693493,40.9622282906908));
#42176=CARTESIAN_POINT('Ctrl Pts',(34.163610390172,-32.7015658728382,41.0363148168372));
#42177=CARTESIAN_POINT('Ctrl Pts',(33.7627339873589,-30.5589596554359,41.147444606057));
#42178=CARTESIAN_POINT('Ctrl Pts',(31.7455321364208,-29.7393678459112,41.2585743952766));
#42179=CARTESIAN_POINT('Ctrl Pts',(29.9627552301519,-30.9866500804378,41.3697041844965));
#42180=CARTESIAN_POINT('Ctrl Pts',(30.0436671869608,-33.1623584352134,41.4808339737161));
#42181=CARTESIAN_POINT('Ctrl Pts',(31.9153852944227,-34.2737746643645,41.5919637629359));
#42182=CARTESIAN_POINT('Ctrl Pts',(33.8643440676371,-33.3045167275176,41.7030935521556));
#42183=CARTESIAN_POINT('Ctrl Pts',(34.1071752850569,-31.1412480182893,41.8142233413753));
#42184=CARTESIAN_POINT('Ctrl Pts',(32.4214920591134,-29.7639660916285,41.925353130595));
#42185=CARTESIAN_POINT('Ctrl Pts',(30.3500893688654,-30.4330446663765,42.0364829198148));
#42186=CARTESIAN_POINT('Ctrl Pts',(29.7886541155055,-32.5362006836436,42.1476127090345));
#42187=CARTESIAN_POINT('Ctrl Pts',(31.2510251411306,-34.1486231057811,42.2587424982542));
#42188=CARTESIAN_POINT('Ctrl Pts',(33.3988465484605,-33.7946532785911,42.369872287474));
#42189=CARTESIAN_POINT('Ctrl Pts',(34.2664604248743,-31.7982340526538,42.4810020766937));
#42190=CARTESIAN_POINT('Ctrl Pts',(33.0598334604292,-29.9864699351082,42.5921318659135));
#42191=CARTESIAN_POINT('Ctrl Pts',(30.8832588301186,-30.0174661407245,42.7032616551331));
#42192=CARTESIAN_POINT('Ctrl Pts',(29.7287133938919,-31.8628561157372,42.8143914443529));
#42193=CARTESIAN_POINT('Ctrl Pts',(30.6528249366209,-33.8337585443777,42.9255212335725));
#42194=CARTESIAN_POINT('Ctrl Pts',(32.8098564332299,-34.1264251112126,43.0366510227924));
#42195=CARTESIAN_POINT('Ctrl Pts',(34.2257161322656,-32.473010440153,43.147780812012));
#42196=CARTESIAN_POINT('Ctrl Pts',(33.6046245500003,-30.3867017621533,43.2589106012318));
#42197=CARTESIAN_POINT('Ctrl Pts',(31.5149979880441,-29.776866126694,43.3700403904514));
#42198=CARTESIAN_POINT('Ctrl Pts',(29.8692400042455,-31.2016185078721,43.4811701796713));
#42199=CARTESIAN_POINT('Ctrl Pts',(30.1735304632281,-33.3570409701995,43.5922999688909));
#42200=CARTESIAN_POINT('Ctrl Pts',(32.1493860341195,-34.2705142542887,43.7034297581108));
#42201=CARTESIAN_POINT('Ctrl Pts',(33.9885251270672,-33.1060375149526,43.8145595473303));
#42202=CARTESIAN_POINT('Ctrl Pts',(34.0077875881485,-30.9293272367134,43.9256893365502));
#42203=CARTESIAN_POINT('Ctrl Pts',(32.189544622223,-29.7324850603179,44.0368191257698));
#42204=CARTESIAN_POINT('Ctrl Pts',(30.1978324735058,-30.6108479666214,44.1479489149896));
#42205=CARTESIAN_POINT('Ctrl Pts',(29.8554445013729,-32.7605477491074,44.2590787042093));
#42206=CARTESIAN_POINT('Ctrl Pts',(31.4757304648326,-34.214202479427,44.370208493429));
#42207=CARTESIAN_POINT('Ctrl Pts',(33.5758222214187,-33.641443112591,44.4813382826487));
#42208=CARTESIAN_POINT('Ctrl Pts',(34.233738570039,-31.5664528098261,44.5924680718685));
#42209=CARTESIAN_POINT('Ctrl Pts',(32.8473616032476,-29.8882401938823,44.7035978610882));
#42210=CARTESIAN_POINT('Ctrl Pts',(30.685488486417,-30.1426872514172,44.8147276503079));
#42211=CARTESIAN_POINT('Ctrl Pts',(29.7266420515343,-32.0969267947364,44.9258574395277));
#42212=CARTESIAN_POINT('Ctrl Pts',(30.8483481575467,-33.9624599866405,45.0369872287473));
#42213=CARTESIAN_POINT('Ctrl Pts',(33.0240335406284,-34.0319710807634,45.1481170179672));
#42214=CARTESIAN_POINT('Ctrl Pts',(34.2625345325082,-32.2418442775805,45.2592468071868));
#42215=CARTESIAN_POINT('Ctrl Pts',(33.4303884564018,-30.2303842142479,45.3703765964066));
#42216=CARTESIAN_POINT('Ctrl Pts',(31.2891663769134,-29.8384573273516,45.4815063856263));
#42217=CARTESIAN_POINT('Ctrl Pts',(29.7984915206042,-31.4247508535089,45.592636174846));
#42218=CARTESIAN_POINT('Ctrl Pts',(30.3226133502727,-33.5375061602177,45.7037659640658));
#42219=CARTESIAN_POINT('Ctrl Pts',(32.3818612512709,-34.2431525026552,45.8148957532854));
#42220=CARTESIAN_POINT('Ctrl Pts',(34.0916338762188,-32.8958900006387,45.9260255425053));
#42221=CARTESIAN_POINT('Ctrl Pts',(33.8871658604762,-30.7287186855601,46.0371553317249));
#42222=CARTESIAN_POINT('Ctrl Pts',(31.9555841146872,-29.7250102429852,46.1482851209447));
#42223=CARTESIAN_POINT('Ctrl Pts',(30.0646513054664,-30.8033477547936,46.2594149101644));
#42224=CARTESIAN_POINT('Ctrl Pts',(29.9449286335,-32.9768484242617,46.3705446993841));
#42225=CARTESIAN_POINT('Ctrl Pts',(31.7059849898336,-34.2563480093256,46.4816744886039));
#42226=CARTESIAN_POINT('Ctrl Pts',(33.7361206950114,-33.4708623653299,46.5928042778235));
#42227=CARTESIAN_POINT('Ctrl Pts',(34.1773775675597,-31.3392594354224,46.7039340670433));
#42228=CARTESIAN_POINT('Ctrl Pts',(32.6259221029539,-29.8123591047833,46.815063856263));
#42229=CARTESIAN_POINT('Ctrl Pts',(30.5016295175672,-30.2875639974689,46.9261936454828));
#42230=CARTESIAN_POINT('Ctrl Pts',(29.7486293485517,-32.3299717490758,47.0373234347024));
#42231=CARTESIAN_POINT('Ctrl Pts',(31.0560591846437,-34.0703929343231,47.1484532239223));
#42232=CARTESIAN_POINT('Ctrl Pts',(33.2273734183378,-33.9160129585544,47.2595830131419));
#42233=CARTESIAN_POINT('Ctrl Pts',(34.2754088098797,-32.008118701412,47.3707128023617));
#42234=CARTESIAN_POINT('Ctrl Pts',(33.2410147344006,-30.092794296781,47.4818425915813));
#42235=CARTESIAN_POINT('Ctrl Pts',(31.0708574322425,-29.9229238689514,47.5929723808012));
#42236=CARTESIAN_POINT('Ctrl Pts',(29.7510413319645,-31.6539709913048,47.7041021700207));
#42237=CARTESIAN_POINT('Ctrl Pts',(30.4894478157314,-33.7017001098877,47.8152319592406));
#42238=CARTESIAN_POINT('Ctrl Pts',(32.6102952772846,-34.1920517420706,47.9263617484602));
#42239=CARTESIAN_POINT('Ctrl Pts',(34.1726071194436,-32.6762613917217,48.0374915376801));
#42240=CARTESIAN_POINT('Ctrl Pts',(33.746572486831,-30.5415639494185,48.1486213268997));
#42241=CARTESIAN_POINT('Ctrl Pts',(31.7220936550605,-29.7416113645272,48.2597511161195));
#42242=CARTESIAN_POINT('Ctrl Pts',(29.9519516964098,-31.0085115676156,48.3708809053392));
#42243=CARTESIAN_POINT('Ctrl Pts',(30.0561613350459,-33.1828112317779,48.4820106945589));
#42244=CARTESIAN_POINT('Ctrl Pts',(31.9393510397954,-34.2746148836708,48.5931404837787));
#42245=CARTESIAN_POINT('Ctrl Pts',(33.8780460152136,-33.2847156611994,48.7042702729983));
#42246=CARTESIAN_POINT('Ctrl Pts',(34.0979736440693,-31.1190585977596,48.8154000622182));
#42247=CARTESIAN_POINT('Ctrl Pts',(32.3978585454495,-29.7596295522384,48.9265298514378));
#42248=CARTESIAN_POINT('Ctrl Pts',(30.3336276206307,-30.4505632447029,49.0376596406576));
#42249=CARTESIAN_POINT('Ctrl Pts',(29.7944426263546,-32.5595246526734,49.1487894298773));
#42250=CARTESIAN_POINT('Ctrl Pts',(31.2737598221652,-34.1564151663094,49.259919219097));
#42251=CARTESIAN_POINT('Ctrl Pts',(33.4177241529833,-33.7797779050877,49.3710490083168));
#42252=CARTESIAN_POINT('Ctrl Pts',(34.2642027135694,-31.7743072060174,49.4821787975364));
#42253=CARTESIAN_POINT('Ctrl Pts',(33.0385075049527,-29.9753881044636,49.5933085867562));
#42254=CARTESIAN_POINT('Ctrl Pts',(30.8623814899483,-30.0293718537029,49.7044383759759));
#42255=CARTESIAN_POINT('Ctrl Pts',(29.7273915983841,-31.886853111861,49.8155681651957));
#42256=CARTESIAN_POINT('Ctrl Pts',(30.672268270567,-33.8478851750169,49.9266979544154));
#42257=CARTESIAN_POINT('Ctrl Pts',(32.832270622876,-34.1177527654777,50.0378277436351));
#42258=CARTESIAN_POINT('Ctrl Pts',(34.2305879267278,-32.4494759910455,50.1489575328549));
#42259=CARTESIAN_POINT('Ctrl Pts',(33.5874953497574,-30.369843663973,50.2600873220745));
#42260=CARTESIAN_POINT('Ctrl Pts',(31.4915442443588,-29.7821127373223,50.3712171112943));
#42261=CARTESIAN_POINT('Ctrl Pts',(29.8609263325507,-31.2241681814899,50.482346900514));
#42262=CARTESIAN_POINT('Ctrl Pts',(30.1879654439028,-33.3762564924093,50.5934766897338));
#42263=CARTESIAN_POINT('Ctrl Pts',(32.1733589303015,-34.2688097863616,50.7046064789534));
#42264=CARTESIAN_POINT('Ctrl Pts',(34.0000962036816,-33.0849729680422,50.8157362681732));
#42265=CARTESIAN_POINT('Ctrl Pts',(33.9963671216043,-30.9081806554344,50.9268660573929));
#42266=CARTESIAN_POINT('Ctrl Pts',(32.1655844995112,-29.7306095666419,51.0379958466127));
#42267=CARTESIAN_POINT('Ctrl Pts',(30.1832607392009,-30.6299599920302,51.1491256358323));
#42268=CARTESIAN_POINT('Ctrl Pts',(29.8635970485653,-32.7831561750772,51.2602554250521));
#42269=CARTESIAN_POINT('Ctrl Pts',(31.499146170939,-34.2196163200051,51.3713852142718));
#42270=CARTESIAN_POINT('Ctrl Pts',(33.5930712857764,-33.6247076789349,51.4825150034915));
#42271=CARTESIAN_POINT('Ctrl Pts',(34.2290348367211,-31.5428841906432,51.5936447927113));
#42272=CARTESIAN_POINT('Ctrl Pts',(32.8250098765671,-29.87940813125,51.704774581931));
#42273=CARTESIAN_POINT('Ctrl Pts',(30.6659448270252,-30.1566747584428,51.8159043711507));
#42274=CARTESIAN_POINT('Ctrl Pts',(29.7277925990474,-32.12093264645,51.9270341603704));
#42275=CARTESIAN_POINT('Ctrl Pts',(30.8691399542786,-33.9745143081351,52.0381639495902));
#42276=CARTESIAN_POINT('Ctrl Pts',(33.0454381380698,-34.0210418476463,52.1492937388099));
#42277=CARTESIAN_POINT('Ctrl Pts',(34.2649627179979,-32.2179338848285,52.2604235280296));
#42278=CARTESIAN_POINT('Ctrl Pts',(33.4116178961986,-30.2153750369296,52.3715533172493));
#42279=CARTESIAN_POINT('Ctrl Pts',(31.2663758518537,-29.8460859127335,52.4826831064691));
#42280=CARTESIAN_POINT('Ctrl Pts',(29.7925383401015,-31.4480349874244,52.5938128956888));
#42281=CARTESIAN_POINT('Ctrl Pts',(30.3389464577195,-33.5551376743476,52.7049426849085));
#42282=CARTESIAN_POINT('Ctrl Pts',(32.4055314629674,-34.2389928142936,52.8160724741283));
#42283=CARTESIAN_POINT('Ctrl Pts',(34.1009810463219,-32.8737507865556,52.927202263348));
#42284=CARTESIAN_POINT('Ctrl Pts',(33.8736304624541,-30.7088520617425,53.0383320525678));
#42285=CARTESIAN_POINT('Ctrl Pts',(31.9315636895405,-29.7256166403411,53.1494618417874));
#42286=CARTESIAN_POINT('Ctrl Pts',(30.0521091088848,-30.8238351627611,53.2605916310072));
#42287=CARTESIAN_POINT('Ctrl Pts',(29.9553826935864,-32.9985403172736,53.3717214202268));
#42288=CARTESIAN_POINT('Ctrl Pts',(31.7297895802091,-34.259247043097,53.4828512094467));
#42289=CARTESIAN_POINT('Ctrl Pts',(33.7516450824844,-33.4526027372595,53.5939809986663));
#42290=CARTESIAN_POINT('Ctrl Pts',(34.1701072171639,-31.3159832035954,53.7051107878861));
#42291=CARTESIAN_POINT('Ctrl Pts',(32.6031181779054,-29.8064959327199,53.8162405771057));
#42292=CARTESIAN_POINT('Ctrl Pts',(30.4829581211195,-30.302233136566,53.9273703663256));
#42293=CARTESIAN_POINT('Ctrl Pts',(29.7535791778743,-32.3563679058385,54.0385001555452));
#42294=CARTESIAN_POINT('Ctrl Pts',(30.634695709741,-33.5006534350279,54.1125866816917));
#42295=CARTESIAN_POINT('Ctrl Pts',(31.2199063053491,-33.7600342388744,54.149629944765));
#42296=CARTESIAN_POINT('Ctrl Pts',(32.4632995769868,-33.7347832743338,40.850370055235));
#42297=CARTESIAN_POINT('Ctrl Pts',(33.0401142382021,-33.5807363726288,40.8874133183083));
#42298=CARTESIAN_POINT('Ctrl Pts',(34.017977364602,-32.6543433409248,40.9614998444548));
#42299=CARTESIAN_POINT('Ctrl Pts',(33.6440840284661,-30.6559563542411,41.0726296336744));
#42300=CARTESIAN_POINT('Ctrl Pts',(31.7626604165639,-29.8915314248051,41.1837594228942));
#42301=CARTESIAN_POINT('Ctrl Pts',(30.0998825618597,-31.0548588556486,41.2948892121139));
#42302=CARTESIAN_POINT('Ctrl Pts',(30.1753483195154,-33.084119868563,41.4060190013337));
#42303=CARTESIAN_POINT('Ctrl Pts',(31.9210807262976,-34.1207264606122,41.5171487905533));
#42304=CARTESIAN_POINT('Ctrl Pts',(33.7388547149761,-33.2167094592598,41.6282785797731));
#42305=CARTESIAN_POINT('Ctrl Pts',(33.965340917112,-31.1990507769925,41.7394083689929));
#42306=CARTESIAN_POINT('Ctrl Pts',(32.3931213487021,-29.9144739579396,41.8505381582125));
#42307=CARTESIAN_POINT('Ctrl Pts',(30.4611451662601,-30.5385167269679,41.9616679474324));
#42308=CARTESIAN_POINT('Ctrl Pts',(29.9375002262487,-32.5001089139672,42.0727977366519));
#42309=CARTESIAN_POINT('Ctrl Pts',(31.3014387808822,-34.0039988771649,42.1839275258718));
#42310=CARTESIAN_POINT('Ctrl Pts',(33.3046899220708,-33.6738548261537,42.2950573150914));
#42311=CARTESIAN_POINT('Ctrl Pts',(34.1139045439687,-31.8118149568232,42.4061871043112));
#42312=CARTESIAN_POINT('Ctrl Pts',(32.9884958692697,-30.1220010255292,42.5173168935309));
#42313=CARTESIAN_POINT('Ctrl Pts',(30.9584268899907,-30.1509108706688,42.6284466827506));
#42314=CARTESIAN_POINT('Ctrl Pts',(29.8815941259713,-31.8720872965886,42.7395764719704));
#42315=CARTESIAN_POINT('Ctrl Pts',(30.7435035455532,-33.7103279090861,42.8507062611901));
#42316=CARTESIAN_POINT('Ctrl Pts',(32.7553448431653,-33.9832950338195,42.9618360504099));
#42317=CARTESIAN_POINT('Ctrl Pts',(34.0759027574205,-32.4411720177464,43.0729658396295));
#42318=CARTESIAN_POINT('Ctrl Pts',(33.4966169673125,-30.4952931724144,43.1840956288493));
#42319=CARTESIAN_POINT('Ctrl Pts',(31.5476435654224,-29.926505689199,43.295225418069));
#42320=CARTESIAN_POINT('Ctrl Pts',(30.012661863539,-31.2553577174755,43.4063552072887));
#42321=CARTESIAN_POINT('Ctrl Pts',(30.2964704740359,-33.2656982852085,43.5174849965084));
#42322=CARTESIAN_POINT('Ctrl Pts',(32.1393308318402,-34.1176855093567,43.6286147857282));
#42323=CARTESIAN_POINT('Ctrl Pts',(33.8546771237519,-33.0315899201231,43.7397445749479));
#42324=CARTESIAN_POINT('Ctrl Pts',(33.8726430249258,-31.0013944234033,43.8508743641676));
#42325=CARTESIAN_POINT('Ctrl Pts',(32.1767863377647,-29.8851119208151,43.9620041533874));
#42326=CARTESIAN_POINT('Ctrl Pts',(30.3191367113942,-30.7043520533629,44.0731339426071));
#42327=CARTESIAN_POINT('Ctrl Pts',(29.9997949385803,-32.7093551359197,44.1842637318268));
#42328=CARTESIAN_POINT('Ctrl Pts',(31.511019146643,-34.0651640907373,44.2953935210465));
#42329=CARTESIAN_POINT('Ctrl Pts',(33.4697533289286,-33.5309572654748,44.4065233102663));
#42330=CARTESIAN_POINT('Ctrl Pts',(34.0833852033863,-31.5956349533947,44.5176530994859));
#42331=CARTESIAN_POINT('Ctrl Pts',(32.7903255330784,-30.030383146809,44.6287828887058));
#42332=CARTESIAN_POINT('Ctrl Pts',(30.7739685056197,-30.2677033246597,44.7399126779254));
#42333=CARTESIAN_POINT('Ctrl Pts',(29.8796622060605,-32.0904026338059,44.8510424671452));
#42334=CARTESIAN_POINT('Ctrl Pts',(30.9258660614085,-33.8303664328691,44.9621722563649));
#42335=CARTESIAN_POINT('Ctrl Pts',(32.9551056488581,-33.8951987220677,45.0733020455846));
#42336=CARTESIAN_POINT('Ctrl Pts',(34.1102429041622,-32.2255656934043,45.1844318348044));
#42337=CARTESIAN_POINT('Ctrl Pts',(33.3341087382084,-30.3494973882954,45.295561624024));
#42338=CARTESIAN_POINT('Ctrl Pts',(31.3370127228531,-29.983951174463,45.4066914132439));
#42339=CARTESIAN_POINT('Ctrl Pts',(29.946675473745,-31.463470982623,45.5178212024635));
#42340=CARTESIAN_POINT('Ctrl Pts',(30.4355185636883,-33.4340163290715,45.6289509916833));
#42341=CARTESIAN_POINT('Ctrl Pts',(32.3561580980493,-34.0921654824133,45.740080780903));
#42342=CARTESIAN_POINT('Ctrl Pts',(33.9508456034494,-32.8355874748403,45.8512105701227));
#42343=CARTESIAN_POINT('Ctrl Pts',(33.7601403686122,-30.8142888718623,45.9623403593424));
#42344=CARTESIAN_POINT('Ctrl Pts',(31.9585737563486,-29.8781402348542,46.0734701485622));
#42345=CARTESIAN_POINT('Ctrl Pts',(30.1949199930259,-30.8838946442965,46.1845999377819));
#42346=CARTESIAN_POINT('Ctrl Pts',(30.0832558768083,-32.9110965716201,46.2957297270016));
#42347=CARTESIAN_POINT('Ctrl Pts',(31.7257751959113,-34.1044727970279,46.4068595162214));
#42348=CARTESIAN_POINT('Ctrl Pts',(33.6192620818722,-33.3718583406529,46.5179893054411));
#42349=CARTESIAN_POINT('Ctrl Pts',(34.0308178706696,-31.3837340080966,46.6291190946608));
#42350=CARTESIAN_POINT('Ctrl Pts',(32.583791167533,-29.9596096282039,46.7402488838806));
#42351=CARTESIAN_POINT('Ctrl Pts',(30.6024851188217,-30.4028283894668,46.8513786731002));
#42352=CARTESIAN_POINT('Ctrl Pts',(29.9001695339471,-32.3077612880849,46.96250846232));
#42353=CARTESIAN_POINT('Ctrl Pts',(31.1195960198908,-33.9310343933798,47.0736382515397));
#42354=CARTESIAN_POINT('Ctrl Pts',(33.1447586808469,-33.7870457630496,47.1847680407594));
#42355=CARTESIAN_POINT('Ctrl Pts',(34.1222506114829,-32.0075722300807,47.2958978299792));
#42356=CARTESIAN_POINT('Ctrl Pts',(33.1574817973392,-30.2211686742594,47.4070276191988));
#42357=CARTESIAN_POINT('Ctrl Pts',(31.1333981946381,-30.0627322571335,47.5181574084187));
#42358=CARTESIAN_POINT('Ctrl Pts',(29.902419166299,-31.6772622694852,47.6292871976383));
#42359=CARTESIAN_POINT('Ctrl Pts',(30.5911233696461,-33.5871583528591,47.740416986858));
#42360=CARTESIAN_POINT('Ctrl Pts',(32.5692161864623,-34.044504323712,47.8515467760779));
#42361=CARTESIAN_POINT('Ctrl Pts',(34.0263685223206,-32.6307421092299,47.9626765652975));
#42362=CARTESIAN_POINT('Ctrl Pts',(33.6290103616028,-30.6397315564939,48.0738063545173));
#42363=CARTESIAN_POINT('Ctrl Pts',(31.7407995838277,-29.8936239317577,48.1849361437369));
#42364=CARTESIAN_POINT('Ctrl Pts',(30.0898062160221,-31.0752488419796,48.2960659329567));
#42365=CARTESIAN_POINT('Ctrl Pts',(30.187001484124,-33.1031959835131,48.4071957221764));
#42366=CARTESIAN_POINT('Ctrl Pts',(31.9434333328055,-34.1215101245977,48.5183255113962));
#42367=CARTESIAN_POINT('Ctrl Pts',(33.7516343818633,-33.1982412064697,48.6294553006159));
#42368=CARTESIAN_POINT('Ctrl Pts',(33.9567586403238,-31.1783549305655,48.7405850898356));
#42369=CARTESIAN_POINT('Ctrl Pts',(32.3710786113237,-29.910429311838,48.8517148790553));
#42370=CARTESIAN_POINT('Ctrl Pts',(30.4457914614202,-30.5548561264658,48.9628446682751));
#42371=CARTESIAN_POINT('Ctrl Pts',(29.9428991113351,-32.5218629422194,49.0739744574948));
#42372=CARTESIAN_POINT('Ctrl Pts',(31.3226431862259,-34.0112664526218,49.1851042467145));
#42373=CARTESIAN_POINT('Ctrl Pts',(33.3222968714541,-33.6599807168611,49.2962340359343));
#42374=CARTESIAN_POINT('Ctrl Pts',(34.1117987996398,-31.7894986307704,49.4073638251539));
#42375=CARTESIAN_POINT('Ctrl Pts',(32.9686053678996,-30.1116651150064,49.5184936143737));
#42376=CARTESIAN_POINT('Ctrl Pts',(30.9389548075454,-30.1620152078494,49.6296234035934));
#42377=CARTESIAN_POINT('Ctrl Pts',(29.8803613007697,-31.8944690503536,49.7407531928132));
#42378=CARTESIAN_POINT('Ctrl Pts',(30.7616381450051,-33.7235036735387,49.8518829820329));
#42379=CARTESIAN_POINT('Ctrl Pts',(32.7762503294566,-33.9752064253202,49.9630127712526));
#42380=CARTESIAN_POINT('Ctrl Pts',(34.0804466304738,-32.4192216768704,50.0741425604724));
#42381=CARTESIAN_POINT('Ctrl Pts',(33.4806407367856,-30.4795697960187,50.185272349692));
#42382=CARTESIAN_POINT('Ctrl Pts',(31.5257684976712,-29.9313991494713,50.2964021389118));
#42383=CARTESIAN_POINT('Ctrl Pts',(30.0049077866622,-31.2763895682868,50.4075319281314));
#42384=CARTESIAN_POINT('Ctrl Pts',(30.3099338334245,-33.2836204069753,50.5186617173513));
#42385=CARTESIAN_POINT('Ctrl Pts',(32.1616901078351,-34.1160957694889,50.6297915065709));
#42386=CARTESIAN_POINT('Ctrl Pts',(33.8654693490056,-33.0119432318589,50.7409212957907));
#42387=CARTESIAN_POINT('Ctrl Pts',(33.8619912721499,-30.9816712225195,50.8520510850104));
#42388=CARTESIAN_POINT('Ctrl Pts',(32.1544389754553,-29.883362666974,50.9631808742301));
#42389=CARTESIAN_POINT('Ctrl Pts',(30.3055458032881,-30.722177644718,51.0743106634499));
#42390=CARTESIAN_POINT('Ctrl Pts',(30.0073987362756,-32.730441784451,51.1854404526696));
#42391=CARTESIAN_POINT('Ctrl Pts',(31.5328587371319,-34.0702135246797,51.2965702418894));
#42392=CARTESIAN_POINT('Ctrl Pts',(33.4858413554941,-33.515348297031,51.4077000311091));
#42393=CARTESIAN_POINT('Ctrl Pts',(34.0789980792498,-31.5736527424373,51.5188298203288));
#42394=CARTESIAN_POINT('Ctrl Pts',(32.7694783053585,-30.022145571987,51.6299596095485));
#42395=CARTESIAN_POINT('Ctrl Pts',(30.7557403336469,-30.2807493299354,51.7410893987682));
#42396=CARTESIAN_POINT('Ctrl Pts',(29.8807353100023,-32.1127926470893,51.8522191879879));
#42397=CARTESIAN_POINT('Ctrl Pts',(30.9452583583604,-33.8416093756986,51.9633489772077));
#42398=CARTESIAN_POINT('Ctrl Pts',(32.9750694987876,-33.8850051377039,52.0744787664274));
#42399=CARTESIAN_POINT('Ctrl Pts',(34.1125076480262,-32.2032647137217,52.1856085556471));
#42400=CARTESIAN_POINT('Ctrl Pts',(33.3166016279713,-30.3354984815481,52.2967383448669));
#42401=CARTESIAN_POINT('Ctrl Pts',(31.3157562323562,-29.9910662783164,52.4078681340865));
#42402=CARTESIAN_POINT('Ctrl Pts',(29.9411230029507,-31.4851878570702,52.5189979233064));
#42403=CARTESIAN_POINT('Ctrl Pts',(30.4507522865762,-33.4504610626425,52.630127712526));
#42404=CARTESIAN_POINT('Ctrl Pts',(32.3782350633087,-34.0882857834639,52.7412575017459));
#42405=CARTESIAN_POINT('Ctrl Pts',(33.9595636137607,-32.8149384554547,52.8523872909654));
#42406=CARTESIAN_POINT('Ctrl Pts',(33.7475160407973,-30.7957594742605,52.9635170801853));
#42407=CARTESIAN_POINT('Ctrl Pts',(31.9361701505726,-29.8787058154891,53.0746468694049));
#42408=CARTESIAN_POINT('Ctrl Pts',(30.1832220140741,-30.9030030409494,53.1857766586248));
#42409=CARTESIAN_POINT('Ctrl Pts',(30.0930062721282,-32.9313283792007,53.2969064478443));
#42410=CARTESIAN_POINT('Ctrl Pts',(31.7479774947954,-34.1071766962865,53.4080362370641));
#42411=CARTESIAN_POINT('Ctrl Pts',(33.6337415198811,-33.3548277716098,53.5191660262838));
#42412=CARTESIAN_POINT('Ctrl Pts',(34.0240368889374,-31.3620245038469,53.6302958155036));
#42413=CARTESIAN_POINT('Ctrl Pts',(32.562522179003,-29.9541411073636,53.7414256047233));
#42414=CARTESIAN_POINT('Ctrl Pts',(30.585070497609,-30.4165101460301,53.8525553939431));
#42415=CARTESIAN_POINT('Ctrl Pts',(29.9047861893194,-32.3323807145313,53.9636851831628));
#42416=CARTESIAN_POINT('Ctrl Pts',(30.7265946003719,-33.3996441678013,54.0377717093093));
#42417=CARTESIAN_POINT('Ctrl Pts',(31.2724145598371,-33.6415660005639,54.0748149723825));
#42418=CARTESIAN_POINT('Ctrl Pts',(32.4298642568859,-33.6095877486649,40.7755550828525));
#42419=CARTESIAN_POINT('Ctrl Pts',(32.9650514619268,-33.4666580759082,40.8125983459258));
#42420=CARTESIAN_POINT('Ctrl Pts',(33.8723443390321,-32.6071208090114,40.8866848720722));
#42421=CARTESIAN_POINT('Ctrl Pts',(33.5254340695732,-30.7529530530463,40.997814661292));
#42422=CARTESIAN_POINT('Ctrl Pts',(31.779788696707,-30.0436950036991,41.1089444505117));
#42423=CARTESIAN_POINT('Ctrl Pts',(30.2370098935675,-31.1230676308593,41.2200742397315));
#42424=CARTESIAN_POINT('Ctrl Pts',(30.30702945207,-33.0058813019126,41.3312040289512));
#42425=CARTESIAN_POINT('Ctrl Pts',(31.9267761581724,-33.9676782568598,41.4423338181709));
#42426=CARTESIAN_POINT('Ctrl Pts',(33.613365362315,-33.1289021910022,41.5534636073906));
#42427=CARTESIAN_POINT('Ctrl Pts',(33.8235065491671,-31.2568535356956,41.6645933966104));
#42428=CARTESIAN_POINT('Ctrl Pts',(32.3647506382908,-30.0649818242506,41.77572318583));
#42429=CARTESIAN_POINT('Ctrl Pts',(30.5722009636549,-30.6439887875594,41.8868529750498));
#42430=CARTESIAN_POINT('Ctrl Pts',(30.0863463369919,-32.4640171442907,41.9979827642695));
#42431=CARTESIAN_POINT('Ctrl Pts',(31.3518524206338,-33.8593746485488,42.1091125534892));
#42432=CARTESIAN_POINT('Ctrl Pts',(33.210533295681,-33.5530563737163,42.220242342709));
#42433=CARTESIAN_POINT('Ctrl Pts',(33.9613486630632,-31.8253958609927,42.3313721319287));
#42434=CARTESIAN_POINT('Ctrl Pts',(32.9171582781102,-30.2575321159502,42.4425019211484));
#42435=CARTESIAN_POINT('Ctrl Pts',(31.0335949498628,-30.2843556006131,42.5536317103682));
#42436=CARTESIAN_POINT('Ctrl Pts',(30.0344748580507,-31.8813184774399,42.6647614995879));
#42437=CARTESIAN_POINT('Ctrl Pts',(30.8341821544855,-33.5868972737945,42.7758912888076));
#42438=CARTESIAN_POINT('Ctrl Pts',(32.7008332531007,-33.8401649564264,42.8870210780274));
#42439=CARTESIAN_POINT('Ctrl Pts',(33.9260893825753,-32.4093335953397,42.998150867247));
#42440=CARTESIAN_POINT('Ctrl Pts',(33.3886093846249,-30.6038845826755,43.1092806564668));
#42441=CARTESIAN_POINT('Ctrl Pts',(31.5802891428005,-30.076145251704,43.2204104456865));
#42442=CARTESIAN_POINT('Ctrl Pts',(30.1560837228325,-31.309096927079,43.3315402349062));
#42443=CARTESIAN_POINT('Ctrl Pts',(30.4194104848436,-33.1743556002176,43.442670024126));
#42444=CARTESIAN_POINT('Ctrl Pts',(32.1292756295609,-33.9648567644247,43.5537998133457));
#42445=CARTESIAN_POINT('Ctrl Pts',(33.7208291204366,-32.9571423252936,43.6649296025654));
#42446=CARTESIAN_POINT('Ctrl Pts',(33.7374984617031,-31.0734616100933,43.7760593917851));
#42447=CARTESIAN_POINT('Ctrl Pts',(32.1640280533063,-30.0377387813122,43.8871891810049));
#42448=CARTESIAN_POINT('Ctrl Pts',(30.4404409492826,-30.7978561401045,43.9983189702246));
#42449=CARTESIAN_POINT('Ctrl Pts',(30.1441453757877,-32.658162522732,44.1094487594443));
#42450=CARTESIAN_POINT('Ctrl Pts',(31.5463078284535,-33.9161257020476,44.2205785486641));
#42451=CARTESIAN_POINT('Ctrl Pts',(33.3636844364385,-33.4204714183585,44.3317083378837));
#42452=CARTESIAN_POINT('Ctrl Pts',(33.9330318367336,-31.6248170969632,44.4428381271036));
#42453=CARTESIAN_POINT('Ctrl Pts',(32.7332894629091,-30.1725260997357,44.5539679163232));
#42454=CARTESIAN_POINT('Ctrl Pts',(30.8624485248225,-30.3927193979021,44.665097705543));
#42455=CARTESIAN_POINT('Ctrl Pts',(30.0326823605866,-32.0838784728755,44.7762274947626));
#42456=CARTESIAN_POINT('Ctrl Pts',(31.0033839652703,-33.6982728790978,44.8873572839824));
#42457=CARTESIAN_POINT('Ctrl Pts',(32.8861777570878,-33.758426363372,44.9984870732021));
#42458=CARTESIAN_POINT('Ctrl Pts',(33.9579512758162,-32.2092871092282,45.1096168624219));
#42459=CARTESIAN_POINT('Ctrl Pts',(33.2378290200149,-30.4686105623428,45.2207466516415));
#42460=CARTESIAN_POINT('Ctrl Pts',(31.3848590687928,-30.1294450215744,45.3318764408614));
#42461=CARTESIAN_POINT('Ctrl Pts',(30.0948594268859,-31.5021911117371,45.443006230081));
#42462=CARTESIAN_POINT('Ctrl Pts',(30.5484237771038,-33.3305264979253,45.5541360193008));
#42463=CARTESIAN_POINT('Ctrl Pts',(32.3304549448276,-33.9411784621714,45.6652658085204));
#42464=CARTESIAN_POINT('Ctrl Pts',(33.81005733068,-32.775284949042,45.7763955977403));
#42465=CARTESIAN_POINT('Ctrl Pts',(33.6331148767482,-30.8998590581646,45.8875253869598));
#42466=CARTESIAN_POINT('Ctrl Pts',(31.96156339801,-30.0312702267232,45.9986551761798));
#42467=CARTESIAN_POINT('Ctrl Pts',(30.3251886805853,-30.9644415337994,46.1097849653993));
#42468=CARTESIAN_POINT('Ctrl Pts',(30.2215831201166,-32.8453447189785,46.2209147546191));
#42469=CARTESIAN_POINT('Ctrl Pts',(31.7455654019891,-33.9525975847302,46.3320445438389));
#42470=CARTESIAN_POINT('Ctrl Pts',(33.5024034687329,-33.2728543159759,46.4431743330586));
#42471=CARTESIAN_POINT('Ctrl Pts',(33.8842581737795,-31.4282085807707,46.5543041222783));
#42472=CARTESIAN_POINT('Ctrl Pts',(32.5416602321121,-30.1068601516244,46.665433911498));
#42473=CARTESIAN_POINT('Ctrl Pts',(30.7033407200763,-30.5180927814648,46.7765637007178));
#42474=CARTESIAN_POINT('Ctrl Pts',(30.0517097193423,-32.2855508270939,46.8876934899375));
#42475=CARTESIAN_POINT('Ctrl Pts',(31.183132855138,-33.7916758524365,46.9988232791572));
#42476=CARTESIAN_POINT('Ctrl Pts',(33.062143943356,-33.6580785675447,47.109953068377));
#42477=CARTESIAN_POINT('Ctrl Pts',(33.9690924130861,-32.0070257587494,47.2210828575967));
#42478=CARTESIAN_POINT('Ctrl Pts',(33.0739488602778,-30.3495430517377,47.3322126468164));
#42479=CARTESIAN_POINT('Ctrl Pts',(31.1959389570337,-30.2025406453155,47.4433424360361));
#42480=CARTESIAN_POINT('Ctrl Pts',(30.0537970006334,-31.7005535476654,47.5544722252559));
#42481=CARTESIAN_POINT('Ctrl Pts',(30.6927989235608,-33.4726165958304,47.6656020144756));
#42482=CARTESIAN_POINT('Ctrl Pts',(32.52813709564,-33.8969569053535,47.7767318036953));
#42483=CARTESIAN_POINT('Ctrl Pts',(33.8801299251977,-32.5852228267379,47.887861592915));
#42484=CARTESIAN_POINT('Ctrl Pts',(33.5114482363745,-30.7378991635692,47.9989913821347));
#42485=CARTESIAN_POINT('Ctrl Pts',(31.759505512595,-30.0456364989882,48.1101211713545));
#42486=CARTESIAN_POINT('Ctrl Pts',(30.2276607356344,-31.1419861163437,48.2212509605742));
#42487=CARTESIAN_POINT('Ctrl Pts',(30.3178416332022,-33.0235807352482,48.3323807497939));
#42488=CARTESIAN_POINT('Ctrl Pts',(31.9475156258155,-33.9684053655245,48.4435105390137));
#42489=CARTESIAN_POINT('Ctrl Pts',(33.6252227485131,-33.11176675174,48.5546403282334));
#42490=CARTESIAN_POINT('Ctrl Pts',(33.8155436365783,-31.2376512633715,48.6657701174532));
#42491=CARTESIAN_POINT('Ctrl Pts',(32.3442986771979,-30.0612290714376,48.7768999066728));
#42492=CARTESIAN_POINT('Ctrl Pts',(30.5579553022097,-30.6591490082288,48.8880296958926));
#42493=CARTESIAN_POINT('Ctrl Pts',(30.0913555963156,-32.4842012317655,48.9991594851123));
#42494=CARTESIAN_POINT('Ctrl Pts',(31.3715265502868,-33.8661177389341,49.110289274332));
#42495=CARTESIAN_POINT('Ctrl Pts',(33.2268695899248,-33.5401835286345,49.2214190635518));
#42496=CARTESIAN_POINT('Ctrl Pts',(33.9593948857103,-31.8046900555234,49.3325488527714));
#42497=CARTESIAN_POINT('Ctrl Pts',(32.8987032308465,-30.2479421255491,49.4436786419912));
#42498=CARTESIAN_POINT('Ctrl Pts',(31.0155281251426,-30.2946585619959,49.554808431211));
#42499=CARTESIAN_POINT('Ctrl Pts',(30.0333310031554,-31.9020849888462,49.6659382204306));
#42500=CARTESIAN_POINT('Ctrl Pts',(30.8510080194431,-33.5991221720603,49.7770680096504));
#42501=CARTESIAN_POINT('Ctrl Pts',(32.7202300360374,-33.8326600851628,49.8881977988701));
#42502=CARTESIAN_POINT('Ctrl Pts',(33.9303053342196,-32.3889673626951,49.9993275880899));
#42503=CARTESIAN_POINT('Ctrl Pts',(33.373786123814,-30.5892959280646,50.1104573773095));
#42504=CARTESIAN_POINT('Ctrl Pts',(31.5599927509835,-30.0806855616201,50.2215871665293));
#42505=CARTESIAN_POINT('Ctrl Pts',(30.1488892407737,-31.3286109550838,50.332716955749));
#42506=CARTESIAN_POINT('Ctrl Pts',(30.4319022229462,-33.1909843215413,50.4438467449688));
#42507=CARTESIAN_POINT('Ctrl Pts',(32.1500212853687,-33.9633817526162,50.5549765341885));
#42508=CARTESIAN_POINT('Ctrl Pts',(33.7308424943297,-32.9389134956757,50.6661063234082));
#42509=CARTESIAN_POINT('Ctrl Pts',(33.7276154226956,-31.0551617896046,50.7772361126279));
#42510=CARTESIAN_POINT('Ctrl Pts',(32.1432934513994,-30.0361157673061,50.8883659018476));
#42511=CARTESIAN_POINT('Ctrl Pts',(30.4278308673753,-30.8143952974057,50.9994956910674));
#42512=CARTESIAN_POINT('Ctrl Pts',(30.1512004239858,-32.677727393825,51.1106254802871));
#42513=CARTESIAN_POINT('Ctrl Pts',(31.5665713033249,-33.9208107293542,51.2217552695069));
#42514=CARTESIAN_POINT('Ctrl Pts',(33.3786114252118,-33.4059889151271,51.3328850587265));
#42515=CARTESIAN_POINT('Ctrl Pts',(33.9289613217785,-31.6044212942316,51.4440148479463));
#42516=CARTESIAN_POINT('Ctrl Pts',(32.7139467341499,-30.164883012724,51.5551446371661));
#42517=CARTESIAN_POINT('Ctrl Pts',(30.8455358402687,-30.404823901428,51.6662744263857));
#42518=CARTESIAN_POINT('Ctrl Pts',(30.0336780209573,-32.1046526477287,51.7774042156055));
#42519=CARTESIAN_POINT('Ctrl Pts',(31.0213767624421,-33.7087044432619,51.8885340048252));
#42520=CARTESIAN_POINT('Ctrl Pts',(32.9047008595054,-33.7489684277615,51.9996637940449));
#42521=CARTESIAN_POINT('Ctrl Pts',(33.9600525780544,-32.1885955426149,52.1107935832646));
#42522=CARTESIAN_POINT('Ctrl Pts',(33.2215853597439,-30.4556219261665,52.2219233724845));
#42523=CARTESIAN_POINT('Ctrl Pts',(31.3651366128586,-30.1360466438995,52.333053161704));
#42524=CARTESIAN_POINT('Ctrl Pts',(30.0897076657999,-31.5223407267159,52.4441829509239));
#42525=CARTESIAN_POINT('Ctrl Pts',(30.5625581154328,-33.3457844509375,52.5553127401435));
#42526=CARTESIAN_POINT('Ctrl Pts',(32.3509386636501,-33.9375787526343,52.6664425293633));
#42527=CARTESIAN_POINT('Ctrl Pts',(33.8181461811994,-32.7561261243537,52.777572318583));
#42528=CARTESIAN_POINT('Ctrl Pts',(33.6214016191404,-30.8826668867785,52.8887021078028));
#42529=CARTESIAN_POINT('Ctrl Pts',(31.9407766116048,-30.0317949906372,52.9998318970224));
#42530=CARTESIAN_POINT('Ctrl Pts',(30.3143349192635,-30.9821709191377,53.1109616862423));
#42531=CARTESIAN_POINT('Ctrl Pts',(30.23062985067,-32.8641164411277,53.2220914754618));
#42532=CARTESIAN_POINT('Ctrl Pts',(31.7661654093819,-33.955106349476,53.3332212646817));
#42533=CARTESIAN_POINT('Ctrl Pts',(33.5158379572776,-33.2570528059602,53.4443510539013));
#42534=CARTESIAN_POINT('Ctrl Pts',(33.8779665607108,-31.4080658040983,53.5554808431211));
#42535=CARTESIAN_POINT('Ctrl Pts',(32.5219261801006,-30.1017862820074,53.6666106323408));
#42536=CARTESIAN_POINT('Ctrl Pts',(30.6871828740984,-30.5307871554942,53.7777404215606));
#42537=CARTESIAN_POINT('Ctrl Pts',(30.0559932007645,-32.3083935232241,53.8888702107803));
#42538=CARTESIAN_POINT('Ctrl Pts',(30.8184934910026,-33.2986349005747,53.9629567369268));
#42539=CARTESIAN_POINT('Ctrl Pts',(31.3249228143251,-33.5230977622534,54.));
#42540=CARTESIAN_POINT('Ctrl Pts',(33.6638410100825,-31.9990545799874,41.6214803633902));
#42541=CARTESIAN_POINT('Ctrl Pts',(33.6649611950912,-31.7834963339009,41.6358513744636));
#42542=CARTESIAN_POINT('Ctrl Pts',(33.6260908134042,-31.5683254077851,41.650222385537));
#42543=CARTESIAN_POINT('Ctrl Pts',(33.5453570328791,-31.3702163596725,41.6645933966103));
#42544=CARTESIAN_POINT('Ctrl Pts',(33.337254578875,-30.8595629652139,41.7016366596836));
#42545=CARTESIAN_POINT('Ctrl Pts',(32.8510026085829,-30.4622723947323,41.7386799227568));
#42546=CARTESIAN_POINT('Ctrl Pts',(32.3091183443309,-30.3601282700429,41.77572318583));
#42547=CARTESIAN_POINT('Ctrl Pts',(31.7672340800789,-30.2579841453535,41.8127664489033));
#42548=CARTESIAN_POINT('Ctrl Pts',(31.1697175218669,-30.4509864664565,41.8498097119765));
#42549=CARTESIAN_POINT('Ctrl Pts',(30.7899834716504,-30.8508256864632,41.8868529750498));
#42550=CARTESIAN_POINT('Ctrl Pts',(30.4102494214339,-31.2506649064699,41.923896238123));
#42551=CARTESIAN_POINT('Ctrl Pts',(30.2482978792129,-31.8573410253802,41.9609395011963));
#42552=CARTESIAN_POINT('Ctrl Pts',(30.3782397887094,-32.3932386688785,41.9979827642695));
#42553=CARTESIAN_POINT('Ctrl Pts',(30.5081816982059,-32.9291363123767,42.0350260273428));
#42554=CARTESIAN_POINT('Ctrl Pts',(30.9300170594198,-33.3942554804628,42.072069290416));
#42555=CARTESIAN_POINT('Ctrl Pts',(31.450714885868,-33.5757620187004,42.1091125534892));
#42556=CARTESIAN_POINT('Ctrl Pts',(31.9714127123162,-33.757268556938,42.1461558165625));
#42557=CARTESIAN_POINT('Ctrl Pts',(32.5909730039986,-33.6551624653271,42.1831990796357));
#42558=CARTESIAN_POINT('Ctrl Pts',(33.0258890444035,-33.3161660007344,42.220242342709));
#42559=CARTESIAN_POINT('Ctrl Pts',(33.4220927932116,-33.0073439348036,42.2539883496027));
#42560=CARTESIAN_POINT('Ctrl Pts',(33.6650600854439,-32.5019263014425,42.2877343564965));
#42561=CARTESIAN_POINT('Ctrl Pts',(33.6682077276635,-31.9991447210259,42.3214803633902));
#42562=CARTESIAN_POINT('Ctrl Pts',(32.5301702171886,-33.9851743256717,41.));
#42563=CARTESIAN_POINT('Ctrl Pts',(32.5988371200409,-33.9597495173352,41.));
#42564=CARTESIAN_POINT('Ctrl Pts',(32.6658006735426,-33.9304353732127,41.));
#42565=CARTESIAN_POINT('Ctrl Pts',(32.7308718973377,-33.8975258144197,41.));
#42566=CARTESIAN_POINT('Ctrl Pts',(32.7977522078449,-33.8637013159338,41.));
#42567=CARTESIAN_POINT('Ctrl Pts',(32.8626342777603,-33.826078018407,41.));
#42568=CARTESIAN_POINT('Ctrl Pts',(32.925281707376,-33.7849304046057,41.));
#42569=CARTESIAN_POINT('Ctrl Pts',(32.9782123635771,-33.7501648888779,41.));
#42570=CARTESIAN_POINT('Ctrl Pts',(33.0295474834986,-33.7128824829906,41.));
#42571=CARTESIAN_POINT('Ctrl Pts',(33.0791217504879,-33.6732307266858,41.));
#42572=CARTESIAN_POINT('Ctrl Pts',(33.1011524559357,-33.6556095652105,41.));
#42573=CARTESIAN_POINT('Ctrl Pts',(33.1228351080429,-33.6375203027614,41.));
#42574=CARTESIAN_POINT('Ctrl Pts',(33.1441536442999,-33.6189751639077,41.));
#42575=CARTESIAN_POINT('Ctrl Pts',(33.1558677305351,-33.6087850010767,41.));
#42576=CARTESIAN_POINT('Ctrl Pts',(33.1674718626525,-33.5984571902042,41.));
#42577=CARTESIAN_POINT('Ctrl Pts',(33.178963241537,-33.5879937176865,41.));
#42578=CARTESIAN_POINT('Ctrl Pts',(33.1895552130653,-33.5783492003393,41.));
#42579=CARTESIAN_POINT('Ctrl Pts',(33.2000528216363,-33.5685879135171,41.));
#42580=CARTESIAN_POINT('Ctrl Pts',(33.210437993979,-33.5587268613668,41.));
#42581=CARTESIAN_POINT('Ctrl Pts',(33.2635230443273,-33.5083209140594,41.));
#42582=CARTESIAN_POINT('Ctrl Pts',(33.3137681124905,-33.4552266753419,41.));
#42583=CARTESIAN_POINT('Ctrl Pts',(33.360954505967,-33.3997034771336,41.));
#42584=CARTESIAN_POINT('Ctrl Pts',(33.4077743219468,-33.3446116226562,41.));
#42585=CARTESIAN_POINT('Ctrl Pts',(33.451583310905,-33.2871275187766,41.));
#42586=CARTESIAN_POINT('Ctrl Pts',(33.4921230471312,-33.2274802596658,41.));
#42587=CARTESIAN_POINT('Ctrl Pts',(33.5258091626199,-33.1779169263528,41.));
#42588=CARTESIAN_POINT('Ctrl Pts',(33.5572373380051,-33.1268593641302,41.));
#42589=CARTESIAN_POINT('Ctrl Pts',(33.5862317099631,-33.0744325355151,41.));
#42590=CARTESIAN_POINT('Ctrl Pts',(33.5983395910643,-33.0525393967949,41.));
#42591=CARTESIAN_POINT('Ctrl Pts',(33.6100227318467,-33.0304074395486,41.));
#42592=CARTESIAN_POINT('Ctrl Pts',(33.6212668835334,-33.0080456806059,41.));
#42593=CARTESIAN_POINT('Ctrl Pts',(33.626466482389,-32.9977050004506,41.));
#42594=CARTESIAN_POINT('Ctrl Pts',(33.6315721959925,-32.9873151798452,41.));
#42595=CARTESIAN_POINT('Ctrl Pts',(33.636582550181,-32.9768771123835,41.));
#42596=CARTESIAN_POINT('Ctrl Pts',(33.6418163462648,-32.9659735485738,41.));
#42597=CARTESIAN_POINT('Ctrl Pts',(33.646942482252,-32.9550247828872,41.));
#42598=CARTESIAN_POINT('Ctrl Pts',(33.6519578880443,-32.9440361447188,41.));
#42599=CARTESIAN_POINT('Ctrl Pts',(33.6804982443946,-32.8815048836164,41.));
#42600=CARTESIAN_POINT('Ctrl Pts',(33.7054776090138,-32.817640230646,41.));
#42601=CARTESIAN_POINT('Ctrl Pts',(33.7266725048855,-32.7526465165606,41.));
#42602=CARTESIAN_POINT('Ctrl Pts',(33.7458696726495,-32.6937787948011,41.));
#42603=CARTESIAN_POINT('Ctrl Pts',(33.7619618380551,-32.6339842234184,41.));
#42604=CARTESIAN_POINT('Ctrl Pts',(33.7747462836708,-32.5734098051776,41.));
#42605=CARTESIAN_POINT('Ctrl Pts',(33.789880467178,-32.5017020136112,41.));
#42606=CARTESIAN_POINT('Ctrl Pts',(33.8003799022934,-32.4288998459686,41.));
#42607=CARTESIAN_POINT('Ctrl Pts',(33.8063197386492,-32.3554264965557,41.));
#42608=CARTESIAN_POINT('Ctrl Pts',(33.8076266775032,-32.3392601967906,41.));
#42609=CARTESIAN_POINT('Ctrl Pts',(33.808712649019,-32.3230614848392,41.));
#42610=CARTESIAN_POINT('Ctrl Pts',(33.809578084761,-32.3068350328842,41.));
#42611=CARTESIAN_POINT('Ctrl Pts',(33.8104757224762,-32.2900048113543,41.));
#42612=CARTESIAN_POINT('Ctrl Pts',(33.8111361175212,-32.2731385190501,41.));
#42613=CARTESIAN_POINT('Ctrl Pts',(33.8115591884844,-32.2562757703559,41.));
#42614=CARTESIAN_POINT('Ctrl Pts',(33.8132793631208,-32.1877131056438,41.));
#42615=CARTESIAN_POINT('Ctrl Pts',(33.8110879096862,-32.1191225382936,41.));
#42616=CARTESIAN_POINT('Ctrl Pts',(33.8051054090175,-32.0508425096977,41.));
#42617=CARTESIAN_POINT('Ctrl Pts',(33.799124181534,-31.9825770123365,41.));
#42618=CARTESIAN_POINT('Ctrl Pts',(33.7893530665424,-31.9146208497202,41.));
#42619=CARTESIAN_POINT('Ctrl Pts',(33.7758629639258,-31.8473272796643,41.));
#42620=CARTESIAN_POINT('Ctrl Pts',(33.7661049760548,-31.7986508641426,41.));
#42621=CARTESIAN_POINT('Ctrl Pts',(33.7544000640131,-31.7503214006864,41.));
#42622=CARTESIAN_POINT('Ctrl Pts',(33.7407608724217,-31.7024822288915,41.));
#42623=CARTESIAN_POINT('Ctrl Pts',(33.7305262530612,-31.6665845211305,41.));
#42624=CARTESIAN_POINT('Ctrl Pts',(33.7192022406327,-31.6309630389482,41.));
#42625=CARTESIAN_POINT('Ctrl Pts',(33.7067902653119,-31.59568252048,41.));
#42626=CARTESIAN_POINT('Ctrl Pts',(33.7026575477152,-31.5839354443118,41.));
#42627=CARTESIAN_POINT('Ctrl Pts',(33.6984073995683,-31.5722353381128,41.));
#42628=CARTESIAN_POINT('Ctrl Pts',(33.6940404882691,-31.560584828957,41.));
#42629=CARTESIAN_POINT('Ctrl Pts',(33.6709167177176,-31.4988927811749,41.));
#42630=CARTESIAN_POINT('Ctrl Pts',(33.6445204253536,-31.4385842551238,41.));
#42631=CARTESIAN_POINT('Ctrl Pts',(33.6149016066083,-31.3799934310527,41.));
#42632=CARTESIAN_POINT('Ctrl Pts',(33.5940761832706,-31.3387973683238,41.));
#42633=CARTESIAN_POINT('Ctrl Pts',(33.5716567844582,-31.2984510155133,41.));
#42634=CARTESIAN_POINT('Ctrl Pts',(33.5476503990608,-31.2590818683295,41.));
#42635=CARTESIAN_POINT('Ctrl Pts',(33.5399365575065,-31.2464315938929,41.));
#42636=CARTESIAN_POINT('Ctrl Pts',(33.5320577131048,-31.2338806239069,41.));
#42637=CARTESIAN_POINT('Ctrl Pts',(33.5240173880638,-31.221438771236,41.));
#42638=CARTESIAN_POINT('Ctrl Pts',(33.4897744370523,-31.168450148347,41.));
#42639=CARTESIAN_POINT('Ctrl Pts',(33.452675776676,-31.117545406851,41.));
#42640=CARTESIAN_POINT('Ctrl Pts',(33.412755652156,-31.0690398416308,41.));
#42641=CARTESIAN_POINT('Ctrl Pts',(33.3759796503983,-31.0243545914407,41.));
#42642=CARTESIAN_POINT('Ctrl Pts',(33.3368085344288,-30.9817053877508,41.));
#42643=CARTESIAN_POINT('Ctrl Pts',(33.295247657559,-30.9413716077237,41.));
#42644=CARTESIAN_POINT('Ctrl Pts',(33.2874058185866,-30.9337613013024,41.));
#42645=CARTESIAN_POINT('Ctrl Pts',(33.279478847569,-30.9262335309294,41.));
#42646=CARTESIAN_POINT('Ctrl Pts',(33.2714683511891,-30.9187889684226,41.));
#42647=CARTESIAN_POINT('Origin',(32.,-32.,48.));
#42648=CARTESIAN_POINT('Origin',(32.,-32.,55.));
#42649=CARTESIAN_POINT('Origin',(-32.,-32.,55.));
#42650=CARTESIAN_POINT('Origin',(-32.,32.,55.));
#42651=CARTESIAN_POINT('Origin',(32.,32.,55.));
#42652=CARTESIAN_POINT('Origin',(-45.,-3.,179.));
#42653=CARTESIAN_POINT('',(-49.9099188538711,-3.,179.));
#42654=CARTESIAN_POINT('',(-49.9099188538711,-3.,41.));
#42655=CARTESIAN_POINT('',(-49.9099188538711,-3.,41.));
#42656=CARTESIAN_POINT('',(-45.,-3.,179.));
#42657=CARTESIAN_POINT('',(-22.5,-3.,179.));
#42658=CARTESIAN_POINT('',(-45.,-3.,41.));
#42659=CARTESIAN_POINT('',(-45.,-3.,179.));
#42660=CARTESIAN_POINT('',(-22.5,-3.,41.));
#42661=CARTESIAN_POINT('Origin',(-45.,3.,179.));
#42662=CARTESIAN_POINT('',(-45.,3.,179.));
#42663=CARTESIAN_POINT('',(-45.,1.5,179.));
#42664=CARTESIAN_POINT('',(-45.,3.,41.));
#42665=CARTESIAN_POINT('',(-45.,3.,179.));
#42666=CARTESIAN_POINT('',(-45.,1.5,41.));
#42667=CARTESIAN_POINT('Origin',(-53.,3.,179.));
#42668=CARTESIAN_POINT('',(-49.9099188538711,3.,41.));
#42669=CARTESIAN_POINT('',(-49.9099188538711,3.,179.));
#42670=CARTESIAN_POINT('',(-49.9099188538711,3.,41.));
#42671=CARTESIAN_POINT('',(-26.5,3.,41.));
#42672=CARTESIAN_POINT('',(-26.5,3.,179.));
#42673=CARTESIAN_POINT('Origin',(0.,0.,41.));
#42674=CARTESIAN_POINT('Origin',(0.,0.,41.));
#42675=CARTESIAN_POINT('',(-40.,-4.89858719658941E-15,41.));
#42676=CARTESIAN_POINT('Origin',(0.,0.,41.));
#42677=CARTESIAN_POINT('Origin',(80.,0.,57.8647410325605));
#42678=CARTESIAN_POINT('Ctrl Pts',(73.8864642614677,0.000114121245111225,
53.4897410325605));
#42679=CARTESIAN_POINT('Ctrl Pts',(73.88634736256,0.135162929769602,53.4835872578684));
#42680=CARTESIAN_POINT('Ctrl Pts',(73.9231853293536,1.26913664614987,53.4319125319522));
#42681=CARTESIAN_POINT('Ctrl Pts',(74.5968874696183,3.36192360377817,53.3347168548118));
#42682=CARTESIAN_POINT('Ctrl Pts',(76.8165950932171,5.51017981513921,53.1981540011394));
#42683=CARTESIAN_POINT('Ctrl Pts',(79.7864084401088,6.36007322196442,53.0615911474669));
#42684=CARTESIAN_POINT('Ctrl Pts',(82.8065504208398,5.71134182197275,52.9250282937945));
#42685=CARTESIAN_POINT('Ctrl Pts',(85.1653847950113,3.71684696339025,52.7884654401221));
#42686=CARTESIAN_POINT('Ctrl Pts',(86.3070993591023,0.846551199044585,52.6519025864497));
#42687=CARTESIAN_POINT('Ctrl Pts',(85.9626718510223,-2.22321740518142,52.5153397327772));
#42688=CARTESIAN_POINT('Ctrl Pts',(84.2132597448983,-4.769129230128,52.3787768791048));
#42689=CARTESIAN_POINT('Ctrl Pts',(81.4710770800909,-6.19129093756104,52.2422140254323));
#42690=CARTESIAN_POINT('Ctrl Pts',(78.3822644661494,-6.15459852582288,52.1056511717599));
#42691=CARTESIAN_POINT('Ctrl Pts',(75.6746389387688,-4.66769782144369,51.9690883180875));
#42692=CARTESIAN_POINT('Ctrl Pts',(74.1666214617889,-2.35736179104307,51.8471182716877));
#42693=CARTESIAN_POINT('Ctrl Pts',(73.8875345335937,-0.678780393631098,
51.7706691765121));
#42694=CARTESIAN_POINT('Ctrl Pts',(73.8869923021753,0.000128310058932178,
51.7397410325606));
#42695=CARTESIAN_POINT('Ctrl Pts',(73.8870077577991,0.000138281717805347,
53.6352589674395));
#42696=CARTESIAN_POINT('Ctrl Pts',(73.8867593267721,0.329017176271155,53.6202764579539));
#42697=CARTESIAN_POINT('Ctrl Pts',(73.9922018351304,1.65695988743391,53.5597729972442));
#42698=CARTESIAN_POINT('Ctrl Pts',(74.9405084533092,3.85979119586914,53.4537485853103));
#42699=CARTESIAN_POINT('Ctrl Pts',(77.3541911747203,5.78754789219838,53.3171857316378));
#42700=CARTESIAN_POINT('Ctrl Pts',(80.391275596298,6.35162199178929,53.1806228779654));
#42701=CARTESIAN_POINT('Ctrl Pts',(83.3361779879638,5.41904570738785,53.044060024293));
#42702=CARTESIAN_POINT('Ctrl Pts',(85.4949699527806,3.20958767782661,52.9074971706206));
#42703=CARTESIAN_POINT('Ctrl Pts',(86.3589850655242,0.243850535977484,52.7709343169481));
#42704=CARTESIAN_POINT('Ctrl Pts',(85.7246308116887,-2.7793433146957,52.6343714632757));
#42705=CARTESIAN_POINT('Ctrl Pts',(83.7413822653001,-5.14764123692896,52.4978086096033));
#42706=CARTESIAN_POINT('Ctrl Pts',(80.8765513474216,-6.30299985802483,52.3612457559308));
#42707=CARTESIAN_POINT('Ctrl Pts',(77.8051787527545,-5.9731825630531,52.2246829022584));
#42708=CARTESIAN_POINT('Ctrl Pts',(75.2509719030383,-4.23590394123515,52.0881200485859));
#42709=CARTESIAN_POINT('Ctrl Pts',(74.0619250280353,-1.96965792532052,51.9749787369797));
#42710=CARTESIAN_POINT('Ctrl Pts',(73.8871918657965,-0.485173931894543,
51.9073583765975));
#42711=CARTESIAN_POINT('Ctrl Pts',(73.8872279103786,-1.26095903429935E-5,
51.8852589674395));
#42712=CARTESIAN_POINT('Ctrl Pts',(83.8799476118145,3.36633437021264,54.));
#42713=CARTESIAN_POINT('Ctrl Pts',(84.4301347069223,2.73220333302164,53.9544790487759));
#42714=CARTESIAN_POINT('Ctrl Pts',(85.2131282914198,1.18960825322011,53.8634371463276));
#42715=CARTESIAN_POINT('Ctrl Pts',(85.1591137460442,-1.40568202732916,53.7268742926551));
#42716=CARTESIAN_POINT('Ctrl Pts',(83.8893923039574,-3.66938767399442,53.5903114389827));
#42717=CARTESIAN_POINT('Ctrl Pts',(81.7032246129214,-5.06866334381662,53.4537485853103));
#42718=CARTESIAN_POINT('Ctrl Pts',(79.1157173213369,-5.27352492015549,53.3171857316378));
#42719=CARTESIAN_POINT('Ctrl Pts',(76.7365771085195,-4.23582589027655,53.1806228779654));
#42720=CARTESIAN_POINT('Ctrl Pts',(75.1263956128531,-2.20002026082073,53.044060024293));
#42721=CARTESIAN_POINT('Ctrl Pts',(74.6645825100926,0.354167410375346,52.9074971706205));
#42722=CARTESIAN_POINT('Ctrl Pts',(75.4599536596021,2.82490673074183,52.7709343169481));
#42723=CARTESIAN_POINT('Ctrl Pts',(77.3250962818604,4.63001123222775,52.6343714632757));
#42724=CARTESIAN_POINT('Ctrl Pts',(79.8205264883211,5.3441469141497,52.4978086096033));
#42725=CARTESIAN_POINT('Ctrl Pts',(82.3582460842022,4.79904062552954,52.3612457559308));
#42726=CARTESIAN_POINT('Ctrl Pts',(84.3402920452745,3.12313640685312,52.2246829022584));
#42727=CARTESIAN_POINT('Ctrl Pts',(85.2996348313694,0.711327341707319,52.088120048586));
#42728=CARTESIAN_POINT('Ctrl Pts',(85.0102244519263,-1.86809176887346,51.9515571949135));
#42729=CARTESIAN_POINT('Ctrl Pts',(83.5402546917934,-4.00733236377704,51.8149943412411));
#42730=CARTESIAN_POINT('Ctrl Pts',(81.2360945799954,-5.2023250682561,51.6784314875687));
#42731=CARTESIAN_POINT('Ctrl Pts',(78.6406734546261,-5.17149371897446,51.5418686338963));
#42732=CARTESIAN_POINT('Ctrl Pts',(76.3655504958444,-3.92210310134558,51.4053057802238));
#42733=CARTESIAN_POINT('Ctrl Pts',(74.9468130152413,-1.74854717831912,51.2687429265514));
#42734=CARTESIAN_POINT('Ctrl Pts',(74.7187581804446,0.837018984838123,51.132180072879));
#42735=CARTESIAN_POINT('Ctrl Pts',(75.7351225611137,3.22535833181042,50.9956172192065));
#42736=CARTESIAN_POINT('Ctrl Pts',(77.7564201786535,4.8537063696547,50.8590543655341));
#42737=CARTESIAN_POINT('Ctrl Pts',(80.306372596804,5.33837538670167,50.7224915118616));
#42738=CARTESIAN_POINT('Ctrl Pts',(82.7841344280458,4.5651628036752,50.5859286581892));
#42739=CARTESIAN_POINT('Ctrl Pts',(84.6058705556718,2.71626073156826,50.4493658045168));
#42740=CARTESIAN_POINT('Ctrl Pts',(85.3423252250402,0.227326037591453,50.3128029508444));
#42741=CARTESIAN_POINT('Ctrl Pts',(84.8199675937518,-2.31517349947107,50.176240097172));
#42742=CARTESIAN_POINT('Ctrl Pts',(83.1618808107925,-4.31214861476392,50.0396772434995));
#42743=CARTESIAN_POINT('Ctrl Pts',(80.7587599293508,-5.29305198416577,49.9031143898271));
#42744=CARTESIAN_POINT('Ctrl Pts',(78.1768524162312,-5.02675330857473,49.7665515361547));
#42745=CARTESIAN_POINT('Ctrl Pts',(76.0245332392176,-3.57600055528289,49.6299886824822));
#42746=CARTESIAN_POINT('Ctrl Pts',(74.8089534497408,-1.28263465200007,49.4934258288098));
#42747=CARTESIAN_POINT('Ctrl Pts',(74.8165401608961,1.31295850424349,49.3568629751374));
#42748=CARTESIAN_POINT('Ctrl Pts',(76.0455057156385,3.59917919704222,49.2203001214649));
#42749=CARTESIAN_POINT('Ctrl Pts',(78.2062689124828,5.03732515559033,49.0837372677925));
#42750=CARTESIAN_POINT('Ctrl Pts',(80.7896890352764,5.28852599171387,48.9471744141201));
#42751=CARTESIAN_POINT('Ctrl Pts',(83.1870346999595,4.29359124262232,48.8106115604476));
#42752=CARTESIAN_POINT('Ctrl Pts',(84.8334192542769,2.2869574219591,48.6740487067752));
#42753=CARTESIAN_POINT('Ctrl Pts',(85.3409050416308,-0.258552265030627,
48.5374858531028));
#42754=CARTESIAN_POINT('Ctrl Pts',(84.5899131661994,-2.74313927175038,48.4009229994303));
#42755=CARTESIAN_POINT('Ctrl Pts',(82.7573998728133,-4.58136026512633,48.2643601457579));
#42756=CARTESIAN_POINT('Ctrl Pts',(80.2751603401001,-5.34007516096028,48.1277972920854));
#42757=CARTESIAN_POINT('Ctrl Pts',(77.7280847657421,-4.84050793882374,47.9912344384131));
#42758=CARTESIAN_POINT('Ctrl Pts',(75.7163406664372,-3.20037164270791,47.8546715847406));
#42759=CARTESIAN_POINT('Ctrl Pts',(74.7139553825858,-0.806131651887682,
47.7181087310682));
#42760=CARTESIAN_POINT('Ctrl Pts',(74.9571209976267,1.77805717143511,47.5815458773958));
#42761=CARTESIAN_POINT('Ctrl Pts',(76.3885403882258,3.94328231426472,47.4449830237233));
#42762=CARTESIAN_POINT('Ctrl Pts',(78.6709281476767,5.17935169194281,47.3084201700509));
#42763=CARTESIAN_POINT('Ctrl Pts',(81.2664851594074,5.19501022890906,47.1718573163784));
#42764=CARTESIAN_POINT('Ctrl Pts',(83.5636202237454,3.98656830348881,47.035294462706));
#42765=CARTESIAN_POINT('Ctrl Pts',(85.0210593160944,1.83877113359181,46.8987316090335));
#42766=CARTESIAN_POINT('Ctrl Pts',(85.2953860064122,-0.742295750063858,
46.7621687553612));
#42767=CARTESIAN_POINT('Ctrl Pts',(84.3219606859846,-3.14845545724768,46.6256059016887));
#42768=CARTESIAN_POINT('Ctrl Pts',(82.3301516009419,-4.81274448252728,46.4890430480163));
#42769=CARTESIAN_POINT('Ctrl Pts',(79.7892888034983,-5.34300633811507,46.3524801943438));
#42770=CARTESIAN_POINT('Ctrl Pts',(77.2980758934855,-4.61429540234531,46.2159173406714));
#42771=CARTESIAN_POINT('Ctrl Pts',(75.4435174658283,-2.79831786136907,46.079354486999));
#42772=CARTESIAN_POINT('Ctrl Pts',(74.6626031950001,-0.322972573830058,
45.9427916333266));
#42773=CARTESIAN_POINT('Ctrl Pts',(75.1393399410234,2.22847475384808,45.8062287796541));
#42774=CARTESIAN_POINT('Ctrl Pts',(76.7613942058816,4.25482648856233,45.6696659259817));
#42775=CARTESIAN_POINT('Ctrl Pts',(79.1465612800289,5.27861329221261,45.5331030723093));
#42776=CARTESIAN_POINT('Ctrl Pts',(81.7328241529721,5.05860024041677,45.3965402186368));
#42777=CARTESIAN_POINT('Ctrl Pts',(83.9107816033226,3.64662901713134,45.2599773649644));
#42778=CARTESIAN_POINT('Ctrl Pts',(85.1672414323057,1.37540245664025,45.123414511292));
#42779=CARTESIAN_POINT('Ctrl Pts',(85.2061439615261,-1.21991023822647,44.9868516576195));
#42780=CARTESIAN_POINT('Ctrl Pts',(84.0183225865111,-3.52777543619547,44.8502888039471));
#42781=CARTESIAN_POINT('Ctrl Pts',(81.8836637040732,-5.00439077085035,44.7137259502747));
#42782=CARTESIAN_POINT('Ctrl Pts',(79.3051570697518,-5.30182131346047,44.5771630966022));
#42783=CARTESIAN_POINT('Ctrl Pts',(76.8903763021125,-4.34998349362811,44.4406002429298));
#42784=CARTESIAN_POINT('Ctrl Pts',(75.20831628743,-2.37315889402526,44.3040373892574));
#42785=CARTESIAN_POINT('Ctrl Pts',(74.6553208923488,0.162853228334741,44.1674745355849));
#42786=CARTESIAN_POINT('Ctrl Pts',(75.3616924434739,2.66049223770987,44.0309116819125));
#42787=CARTESIAN_POINT('Ctrl Pts',(77.1609885844208,4.53123935855979,43.8943488282401));
#42788=CARTESIAN_POINT('Ctrl Pts',(79.6292410961376,5.33429037095907,43.7577859745677));
#42789=CARTESIAN_POINT('Ctrl Pts',(82.1848555418488,4.88042234010467,43.6212231208952));
#42790=CARTESIAN_POINT('Ctrl Pts',(84.2256523932433,3.2765801939049,43.4846602672228));
#42791=CARTESIAN_POINT('Ctrl Pts',(85.2707586024651,0.900677349257217,43.3480974135504));
#42792=CARTESIAN_POINT('Ctrl Pts',(85.0739157663178,-1.68745217721733,43.2115345598779));
#42793=CARTESIAN_POINT('Ctrl Pts',(83.6815059410305,-3.87796718981677,43.0749717062055));
#42794=CARTESIAN_POINT('Ctrl Pts',(81.4216227696065,-5.15471683823141,42.9384088525331));
#42795=CARTESIAN_POINT('Ctrl Pts',(78.8267624800316,-5.21685994000325,42.8018459988606));
#42796=CARTESIAN_POINT('Ctrl Pts',(76.5083523841484,-4.04975502185875,42.6652831451882));
#42797=CARTESIAN_POINT('Ctrl Pts',(75.0126789436487,-1.92840426961145,42.5287202915158));
#42798=CARTESIAN_POINT('Ctrl Pts',(74.6921690274326,0.647332400775962,42.3921574378433));
#42799=CARTESIAN_POINT('Ctrl Pts',(75.6223416665355,3.07054676838256,42.2555945841709));
#42800=CARTESIAN_POINT('Ctrl Pts',(77.5840260405478,4.77022963457038,42.1190317304985));
#42801=CARTESIAN_POINT('Ctrl Pts',(80.1149778044545,5.34594259971938,41.9824688768261));
#42802=CARTESIAN_POINT('Ctrl Pts',(82.6188542837379,4.66190740327312,41.8459060231536));
#42803=CARTESIAN_POINT('Ctrl Pts',(84.5056048859645,2.87956962377209,41.7093431694812));
#42804=CARTESIAN_POINT('Ctrl Pts',(85.3307462672301,0.418352259874965,41.5727803158088));
#42805=CARTESIAN_POINT('Ctrl Pts',(85.0431484786228,-1.28750999880251,41.4817384133605));
#42806=CARTESIAN_POINT('Ctrl Pts',(84.7069873520512,-2.056810791038,41.4362174621363));
#42807=CARTESIAN_POINT('Ctrl Pts',(84.1258079218638,3.57964859370108,54.1879275126212));
#42808=CARTESIAN_POINT('Ctrl Pts',(84.7108586757943,2.90533462905485,54.1424065613971));
#42809=CARTESIAN_POINT('Ctrl Pts',(85.5434681481107,1.26499005814018,54.0513646589488));
#42810=CARTESIAN_POINT('Ctrl Pts',(85.4860308676361,-1.49475576070059,53.9148018052764));
#42811=CARTESIAN_POINT('Ctrl Pts',(84.1358510950097,-3.90190545038712,53.7782389516039));
#42812=CARTESIAN_POINT('Ctrl Pts',(81.8111527019866,-5.38984890246992,53.6416760979315));
#42813=CARTESIAN_POINT('Ctrl Pts',(79.0596830561099,-5.60769192487844,53.5051132442591));
#42814=CARTESIAN_POINT('Ctrl Pts',(76.5297840679439,-4.50423710890409,53.3685503905866));
#42815=CARTESIAN_POINT('Ctrl Pts',(74.8175703385033,-2.33942875741822,53.2319875369142));
#42816=CARTESIAN_POINT('Ctrl Pts',(74.3264935641706,0.376609906521191,53.0954246832418));
#42817=CARTESIAN_POINT('Ctrl Pts',(75.1722649296075,3.00391235508727,52.9588618295694));
#42818=CARTESIAN_POINT('Ctrl Pts',(77.1555958856459,4.9234007598649,52.8222989758969));
#42819=CARTESIAN_POINT('Ctrl Pts',(79.8091538055837,5.68278901675461,52.6857361222245));
#42820=CARTESIAN_POINT('Ctrl Pts',(82.5076808630813,5.10314102434395,52.5491732685521));
#42821=CARTESIAN_POINT('Ctrl Pts',(84.6153229618534,3.32103992569883,52.4126104148796));
#42822=CARTESIAN_POINT('Ctrl Pts',(85.6354563406138,0.756401960819743,52.2760475612072));
#42823=CARTESIAN_POINT('Ctrl Pts',(85.3277069182916,-1.98646698097611,52.1394847075348));
#42824=CARTESIAN_POINT('Ctrl Pts',(83.7645897094951,-4.26126465256069,52.0029218538623));
#42825=CARTESIAN_POINT('Ctrl Pts',(81.3144220800272,-5.53198035802442,51.8663590001899));
#42826=CARTESIAN_POINT('Ctrl Pts',(78.5545371251339,-5.49919532125727,51.7297961465174));
#42827=CARTESIAN_POINT('Ctrl Pts',(76.1352466434858,-4.17063467471162,51.5932332928451));
#42828=CARTESIAN_POINT('Ctrl Pts',(74.6266081457151,-1.85934721852798,51.4566704391726));
#42829=CARTESIAN_POINT('Ctrl Pts',(74.3841021796143,0.890058295601701,51.3201075855002));
#42830=CARTESIAN_POINT('Ctrl Pts',(75.4648704354783,3.42973933867357,51.1835447318277));
#42831=CARTESIAN_POINT('Ctrl Pts',(77.6142514470921,5.16127076802383,51.0469818781553));
#42832=CARTESIAN_POINT('Ctrl Pts',(80.3257864830666,5.67665176541806,50.9104190244829));
#42833=CARTESIAN_POINT('Ctrl Pts',(82.960556437357,4.85444308646029,50.7738561708105));
#42834=CARTESIAN_POINT('Ctrl Pts',(84.8977303631125,2.88838179413223,50.637293317138));
#42835=CARTESIAN_POINT('Ctrl Pts',(85.6808518928265,0.241730987265083,50.5007304634656));
#42836=CARTESIAN_POINT('Ctrl Pts',(85.1253940699802,-2.46187890154005,50.3641676097932));
#42837=CARTESIAN_POINT('Ctrl Pts',(83.3622394429846,-4.58539616897732,50.2276047561207));
#42838=CARTESIAN_POINT('Ctrl Pts',(80.8068402052069,-5.62845635869168,50.0910419024483));
#42839=CARTESIAN_POINT('Ctrl Pts',(78.0613251784804,-5.34528315759231,49.9544790487759));
#42840=CARTESIAN_POINT('Ctrl Pts',(75.7726201753865,-3.80260067807349,49.8179161951034));
#42841=CARTESIAN_POINT('Ctrl Pts',(74.4800128448624,-1.36391125281304,49.681353341431));
#42842=CARTESIAN_POINT('Ctrl Pts',(74.4880803024976,1.39615663402034,49.5447904877586));
#42843=CARTESIAN_POINT('Ctrl Pts',(75.7949216129355,3.82724807885216,49.4082276340861));
#42844=CARTESIAN_POINT('Ctrl Pts',(78.0926057073459,5.35652490993785,49.2716647804137));
#42845=CARTESIAN_POINT('Ctrl Pts',(80.8397291931549,5.62364356806135,49.1351019267413));
#42846=CARTESIAN_POINT('Ctrl Pts',(83.3889872565054,4.56566287341486,48.9985390730688));
#42847=CARTESIAN_POINT('Ctrl Pts',(85.1396981207328,2.43187485824618,48.8619762193964));
#42848=CARTESIAN_POINT('Ctrl Pts',(85.6793417167757,-0.274935924400359,
48.725413365724));
#42849=CARTESIAN_POINT('Ctrl Pts',(84.8807618030997,-2.91696354448211,48.5888505120515));
#42850=CARTESIAN_POINT('Ctrl Pts',(82.9321277958387,-4.87166693107243,48.4522876583791));
#42851=CARTESIAN_POINT('Ctrl Pts',(80.292596401949,-5.67845924912743,48.3157248047067));
#42852=CARTESIAN_POINT('Ctrl Pts',(77.5841205064826,-5.14723599334988,48.1791619510343));
#42853=CARTESIAN_POINT('Ctrl Pts',(75.4448983900806,-3.40316932016962,48.0425990973618));
#42854=CARTESIAN_POINT('Ctrl Pts',(74.3789950432723,-0.857213727653378,
47.9060362436894));
#42855=CARTESIAN_POINT('Ctrl Pts',(74.6375693131429,1.8907271688658,47.7694733900169));
#42856=CARTESIAN_POINT('Ctrl Pts',(76.1596933344209,4.19315594901299,47.6329105363445));
#42857=CARTESIAN_POINT('Ctrl Pts',(78.5867089647436,5.50755122972981,47.4963476826721));
#42858=CARTESIAN_POINT('Ctrl Pts',(81.3467384166979,5.52420199987513,47.3597848289997));
#42859=CARTESIAN_POINT('Ctrl Pts',(83.7894358431213,4.23918483783166,47.2232219753272));
#42860=CARTESIAN_POINT('Ctrl Pts',(85.3392283543752,1.9552883874944,47.0866591216548));
#42861=CARTESIAN_POINT('Ctrl Pts',(85.6309382807271,-0.789332741672519,
46.9500962679824));
#42862=CARTESIAN_POINT('Ctrl Pts',(84.5958300008798,-3.34796336620454,46.8135334143099));
#42863=CARTESIAN_POINT('Ctrl Pts',(82.4778061190918,-5.11771325248156,46.6769705606375));
#42864=CARTESIAN_POINT('Ctrl Pts',(79.7759366850458,-5.68157616593548,46.540407706965));
#42865=CARTESIAN_POINT('Ctrl Pts',(77.126863298621,-4.90668906632807,46.4038448532927));
#42866=CARTESIAN_POINT('Ctrl Pts',(75.154787224942,-2.97563863109226,46.2672819996202));
#42867=CARTESIAN_POINT('Ctrl Pts',(74.3243888259871,-0.343438349423903,
46.1307191459478));
#42868=CARTESIAN_POINT('Ctrl Pts',(74.8313349088149,2.36968632388313,45.9941562922753));
#42869=CARTESIAN_POINT('Ctrl Pts',(76.556173748202,4.52444171648408,45.8575934386029));
#42870=CARTESIAN_POINT('Ctrl Pts',(79.0924815013068,5.61310273137458,45.7210305849305));
#42871=CARTESIAN_POINT('Ctrl Pts',(81.8426278735721,5.37914813125352,45.5844677312581));
#42872=CARTESIAN_POINT('Ctrl Pts',(84.1585957682871,3.87770464765186,45.4479048775857));
#42873=CARTESIAN_POINT('Ctrl Pts',(85.4946735803011,1.46255746703329,45.3113420239132));
#42874=CARTESIAN_POINT('Ctrl Pts',(85.5360412427791,-1.29721218645108,45.1747791702407));
#42875=CARTESIAN_POINT('Ctrl Pts',(84.2729512918033,-3.75131968196986,45.0382163165683));
#42876=CARTESIAN_POINT('Ctrl Pts',(82.003025661668,-5.32150357484349,44.9016534628959));
#42877=CARTESIAN_POINT('Ctrl Pts',(79.2611270169371,-5.63778137332934,44.7650906092235));
#42878=CARTESIAN_POINT('Ctrl Pts',(76.6933290419456,-4.62562852738992,44.628527755551));
#42879=CARTESIAN_POINT('Ctrl Pts',(74.9046820734928,-2.52353865165512,44.4919649018786));
#42880=CARTESIAN_POINT('Ctrl Pts',(74.3166450662836,0.173172734992249,44.3554020482062));
#42881=CARTESIAN_POINT('Ctrl Pts',(75.0677772033611,2.82907942287063,44.2188391945338));
#42882=CARTESIAN_POINT('Ctrl Pts',(76.9810891897119,4.81837001728588,44.0822763408613));
#42883=CARTESIAN_POINT('Ctrl Pts',(79.6057472482362,5.67230789483062,43.9457134871889));
#42884=CARTESIAN_POINT('Ctrl Pts',(82.32330309699,5.18967964709919,43.8091506335164));
#42885=CARTESIAN_POINT('Ctrl Pts',(84.4934189487503,3.48420697214328,43.672587779844));
#42886=CARTESIAN_POINT('Ctrl Pts',(85.6047503141703,0.957750494180222,43.5360249261716));
#42887=CARTESIAN_POINT('Ctrl Pts',(85.3954341547806,-1.7943808156919,43.3994620724992));
#42888=CARTESIAN_POINT('Ctrl Pts',(83.9147916146189,-4.12370200663389,43.2628992188267));
#42889=CARTESIAN_POINT('Ctrl Pts',(81.5117066186369,-5.48135534134026,43.1263363651543));
#42890=CARTESIAN_POINT('Ctrl Pts',(78.7524180379719,-5.54743625975233,42.9897735114818));
#42891=CARTESIAN_POINT('Ctrl Pts',(76.2870974468905,-4.30637550360597,42.8532106578094));
#42892=CARTESIAN_POINT('Ctrl Pts',(74.6966477948012,-2.05060129881445,42.716647804137));
#42893=CARTESIAN_POINT('Ctrl Pts',(74.3558281540067,0.688351857913759,42.5800849504646));
#42894=CARTESIAN_POINT('Ctrl Pts',(75.3449429635535,3.26511784408383,42.4435220967921));
#42895=CARTESIAN_POINT('Ctrl Pts',(77.4309332243115,5.07250436977312,42.3069592431197));
#42896=CARTESIAN_POINT('Ctrl Pts',(80.1222635932022,5.68469848937892,42.1703963894473));
#42897=CARTESIAN_POINT('Ctrl Pts',(82.7848030002136,4.95731809286584,42.0338335357748));
#42898=CARTESIAN_POINT('Ctrl Pts',(84.7911111672477,3.06203906700717,41.8972706821024));
#42899=CARTESIAN_POINT('Ctrl Pts',(85.6685392121824,0.444861951915516,41.76070782843));
#42900=CARTESIAN_POINT('Ctrl Pts',(85.3627172389852,-1.36909553530131,41.6696659259817));
#42901=CARTESIAN_POINT('Ctrl Pts',(85.0052546189208,-2.18714454535403,41.6241449747575));
#42902=CARTESIAN_POINT('Ctrl Pts',(84.371668231913,3.79296281718951,54.3758550252424));
#42903=CARTESIAN_POINT('Ctrl Pts',(84.9915826446663,3.07846592508805,54.3303340740183));
#42904=CARTESIAN_POINT('Ctrl Pts',(85.8738080048016,1.34037186306025,54.23929217157));
#42905=CARTESIAN_POINT('Ctrl Pts',(85.812947989228,-1.58382949407201,54.1027293178976));
#42906=CARTESIAN_POINT('Ctrl Pts',(84.3823098860621,-4.13442322677981,53.9661664642251));
#42907=CARTESIAN_POINT('Ctrl Pts',(81.9190807910518,-5.71103446112322,53.8296036105527));
#42908=CARTESIAN_POINT('Ctrl Pts',(79.0036487908829,-5.94185892960139,53.6930407568803));
#42909=CARTESIAN_POINT('Ctrl Pts',(76.3229910273682,-4.77264832753163,53.5564779032079));
#42910=CARTESIAN_POINT('Ctrl Pts',(74.5087450641535,-2.47883725401571,53.4199150495354));
#42911=CARTESIAN_POINT('Ctrl Pts',(73.9884046182486,0.399052402667041,53.283352195863));
#42912=CARTESIAN_POINT('Ctrl Pts',(74.884576199613,3.18291797943272,53.1467893421906));
#42913=CARTESIAN_POINT('Ctrl Pts',(76.9860954894315,5.21679028750206,53.0102264885181));
#42914=CARTESIAN_POINT('Ctrl Pts',(79.7977811228463,6.02143111935951,52.8736636348457));
#42915=CARTESIAN_POINT('Ctrl Pts',(82.6571156419606,5.40724142315835,52.7371007811733));
#42916=CARTESIAN_POINT('Ctrl Pts',(84.8903538784323,3.51894344454454,52.6005379275008));
#42917=CARTESIAN_POINT('Ctrl Pts',(85.971277849858,0.801476579932164,52.4639750738284));
#42918=CARTESIAN_POINT('Ctrl Pts',(85.6451893846569,-2.10484219307877,52.3274122201559));
#42919=CARTESIAN_POINT('Ctrl Pts',(83.9889247271966,-4.51519694134435,52.1908493664836));
#42920=CARTESIAN_POINT('Ctrl Pts',(81.392749580059,-5.86163564779273,52.0542865128111));
#42921=CARTESIAN_POINT('Ctrl Pts',(78.4684007956417,-5.82689692354007,51.9177236591387));
#42922=CARTESIAN_POINT('Ctrl Pts',(75.9049427911273,-4.41916624807766,51.7811608054662));
#42923=CARTESIAN_POINT('Ctrl Pts',(74.3064032761888,-1.97014725873684,51.6445979517938));
#42924=CARTESIAN_POINT('Ctrl Pts',(74.0494461787839,0.943097606365279,51.5080350981214));
#42925=CARTESIAN_POINT('Ctrl Pts',(75.194618309843,3.63412034553672,51.371472244449));
#42926=CARTESIAN_POINT('Ctrl Pts',(77.4720827155306,5.46883516639296,51.2349093907765));
#42927=CARTESIAN_POINT('Ctrl Pts',(80.3452003693293,6.01492814413444,51.0983465371041));
#42928=CARTESIAN_POINT('Ctrl Pts',(83.1369784466681,5.14372336924537,50.9617836834317));
#42929=CARTESIAN_POINT('Ctrl Pts',(85.1895901705532,3.06050285669621,50.8252208297592));
#42930=CARTESIAN_POINT('Ctrl Pts',(86.0193785606126,0.256135936938712,50.6886579760868));
#42931=CARTESIAN_POINT('Ctrl Pts',(85.4308205462086,-2.60858430360903,50.5520951224144));
#42932=CARTESIAN_POINT('Ctrl Pts',(83.5625980751767,-4.85864372319071,50.415532268742));
#42933=CARTESIAN_POINT('Ctrl Pts',(80.854920481063,-5.96386073321759,50.2789694150695));
#42934=CARTESIAN_POINT('Ctrl Pts',(77.9457979407295,-5.6638130066099,50.1424065613971));
#42935=CARTESIAN_POINT('Ctrl Pts',(75.5207071115553,-4.02920080086409,50.0058437077247));
#42936=CARTESIAN_POINT('Ctrl Pts',(74.1510722399839,-1.44518785362601,49.8692808540522));
#42937=CARTESIAN_POINT('Ctrl Pts',(74.1596204440991,1.4793547637972,49.7327180003798));
#42938=CARTESIAN_POINT('Ctrl Pts',(75.5443375102325,4.05531696066211,49.5961551467073));
#42939=CARTESIAN_POINT('Ctrl Pts',(77.9789425022089,5.67572466428538,49.4595922930349));
#42940=CARTESIAN_POINT('Ctrl Pts',(80.8897693510335,5.95876114440882,49.3230294393625));
#42941=CARTESIAN_POINT('Ctrl Pts',(83.5909398130512,4.8377345042074,49.1864665856901));
#42942=CARTESIAN_POINT('Ctrl Pts',(85.4459769871887,2.57679229453327,49.0499037320176));
#42943=CARTESIAN_POINT('Ctrl Pts',(86.0177783919207,-0.29131958377009,48.9133408783452));
#42944=CARTESIAN_POINT('Ctrl Pts',(85.17161044,-3.09078781721385,48.7767780246728));
#42945=CARTESIAN_POINT('Ctrl Pts',(83.1068557188642,-5.16197359701852,48.6402151710003));
#42946=CARTESIAN_POINT('Ctrl Pts',(80.310032463798,-6.01684333729458,48.5036523173279));
#42947=CARTESIAN_POINT('Ctrl Pts',(77.4401562472232,-5.45396404787602,48.3670894636555));
#42948=CARTESIAN_POINT('Ctrl Pts',(75.173456113724,-3.60596699763133,48.2305266099831));
#42949=CARTESIAN_POINT('Ctrl Pts',(74.0440347039589,-0.908295803419074,
48.0939637563106));
#42950=CARTESIAN_POINT('Ctrl Pts',(74.318017628659,2.0033971662965,47.9574009026382));
#42951=CARTESIAN_POINT('Ctrl Pts',(75.930846280616,4.44302958376126,47.8208380489657));
#42952=CARTESIAN_POINT('Ctrl Pts',(78.5024897818106,5.83575076751681,47.6842751952933));
#42953=CARTESIAN_POINT('Ctrl Pts',(81.4269916739885,5.85339377084119,47.5477123416209));
#42954=CARTESIAN_POINT('Ctrl Pts',(84.0152514624972,4.49180137217451,47.4111494879485));
#42955=CARTESIAN_POINT('Ctrl Pts',(85.657397392656,2.07180564139699,47.274586634276));
#42956=CARTESIAN_POINT('Ctrl Pts',(85.966490555042,-0.83636973328118,47.1380237806036));
#42957=CARTESIAN_POINT('Ctrl Pts',(84.869699315775,-3.5474712751614,47.0014609269311));
#42958=CARTESIAN_POINT('Ctrl Pts',(82.6254606372418,-5.42268202243584,46.8648980732587));
#42959=CARTESIAN_POINT('Ctrl Pts',(79.7625845665931,-6.02014599375589,46.7283352195863));
#42960=CARTESIAN_POINT('Ctrl Pts',(76.9556507037564,-5.19908273031082,46.5917723659139));
#42961=CARTESIAN_POINT('Ctrl Pts',(74.8660569840556,-3.15295940081547,46.4552095122415));
#42962=CARTESIAN_POINT('Ctrl Pts',(73.9861744569741,-0.363904125017746,
46.318646658569));
#42963=CARTESIAN_POINT('Ctrl Pts',(74.5233298766064,2.51089789391818,46.1820838048966));
#42964=CARTESIAN_POINT('Ctrl Pts',(76.3509532905225,4.79405694440583,46.0455209512242));
#42965=CARTESIAN_POINT('Ctrl Pts',(79.0384017225848,5.94759217053654,45.9089580975517));
#42966=CARTESIAN_POINT('Ctrl Pts',(81.9524315941722,5.69969602209027,45.7723952438793));
#42967=CARTESIAN_POINT('Ctrl Pts',(84.4064099332516,4.10878027817237,45.6358323902068));
#42968=CARTESIAN_POINT('Ctrl Pts',(85.8221057282965,1.54971247742632,45.4992695365344));
#42969=CARTESIAN_POINT('Ctrl Pts',(85.8659385240322,-1.37451413467567,45.362706682862));
#42970=CARTESIAN_POINT('Ctrl Pts',(84.5275799970954,-3.97486392774426,45.2261438291896));
#42971=CARTESIAN_POINT('Ctrl Pts',(82.122387619263,-5.63861637883664,45.0895809755171));
#42972=CARTESIAN_POINT('Ctrl Pts',(79.2170969641224,-5.97374143319821,44.9530181218447));
#42973=CARTESIAN_POINT('Ctrl Pts',(76.4962817817787,-4.90127356115173,44.8164552681723));
#42974=CARTESIAN_POINT('Ctrl Pts',(74.6010478595557,-2.67391840928499,44.6798924144998));
#42975=CARTESIAN_POINT('Ctrl Pts',(73.9779692402184,0.183492241649758,44.5433295608274));
#42976=CARTESIAN_POINT('Ctrl Pts',(74.7738619632483,2.9976666080314,44.406766707155));
#42977=CARTESIAN_POINT('Ctrl Pts',(76.801189795003,5.10550067601197,44.2702038534825));
#42978=CARTESIAN_POINT('Ctrl Pts',(79.5822534003349,6.01032541870217,44.1336409998101));
#42979=CARTESIAN_POINT('Ctrl Pts',(82.4617506521313,5.49893695409371,43.9970781461377));
#42980=CARTESIAN_POINT('Ctrl Pts',(84.7611855042573,3.69183375038168,43.8605152924653));
#42981=CARTESIAN_POINT('Ctrl Pts',(85.9387420258757,1.01482363910322,43.7239524387928));
#42982=CARTESIAN_POINT('Ctrl Pts',(85.7169525432435,-1.90130945416647,43.5873895851204));
#42983=CARTESIAN_POINT('Ctrl Pts',(84.1480772882073,-4.36943682345102,43.450826731448));
#42984=CARTESIAN_POINT('Ctrl Pts',(81.6017904676673,-5.8079938444491,43.3142638777755));
#42985=CARTESIAN_POINT('Ctrl Pts',(78.6780735959123,-5.87801257950141,43.1777010241031));
#42986=CARTESIAN_POINT('Ctrl Pts',(76.0658425096326,-4.56299598535319,43.0411381704307));
#42987=CARTESIAN_POINT('Ctrl Pts',(74.3806166459536,-2.17279832801746,42.9045753167582));
#42988=CARTESIAN_POINT('Ctrl Pts',(74.0194872805808,0.729371315051554,42.7680124630858));
#42989=CARTESIAN_POINT('Ctrl Pts',(75.0675442605715,3.45968891978511,42.6314496094134));
#42990=CARTESIAN_POINT('Ctrl Pts',(77.2778404080753,5.37477910497586,42.4948867557409));
#42991=CARTESIAN_POINT('Ctrl Pts',(80.1295493819499,6.02345437903847,42.3583239020685));
#42992=CARTESIAN_POINT('Ctrl Pts',(82.9507517166893,5.25272878245856,42.2217610483961));
#42993=CARTESIAN_POINT('Ctrl Pts',(85.0766174485309,3.24450851024225,42.0851981947236));
#42994=CARTESIAN_POINT('Ctrl Pts',(86.0063321571346,0.471371643956068,41.9486353410512));
#42995=CARTESIAN_POINT('Ctrl Pts',(85.6822859993477,-1.45068107180012,41.8575934386029));
#42996=CARTESIAN_POINT('Ctrl Pts',(85.3035218857904,-2.31747829967006,41.8120724873788));
#42997=CARTESIAN_POINT('Ctrl Pts',(84.6175285419623,4.00627704067795,54.5637825378637));
#42998=CARTESIAN_POINT('Ctrl Pts',(85.2723066135383,3.25159722112125,54.5182615866395));
#42999=CARTESIAN_POINT('Ctrl Pts',(86.2041478614926,1.41575366798031,54.4272196841912));
#43000=CARTESIAN_POINT('Ctrl Pts',(86.13986511082,-1.67290322744343,54.2906568305188));
#43001=CARTESIAN_POINT('Ctrl Pts',(84.6287686771144,-4.36694100317251,54.1540939768463));
#43002=CARTESIAN_POINT('Ctrl Pts',(82.0270088801171,-6.03222001977652,54.0175311231739));
#43003=CARTESIAN_POINT('Ctrl Pts',(78.9476145256559,-6.27602593432435,53.8809682695015));
#43004=CARTESIAN_POINT('Ctrl Pts',(76.1161979867926,-5.04105954615917,53.7444054158291));
#43005=CARTESIAN_POINT('Ctrl Pts',(74.1999197898036,-2.6182457506132,53.6078425621567));
#43006=CARTESIAN_POINT('Ctrl Pts',(73.6503156723266,0.421494898812886,53.4712797084842));
#43007=CARTESIAN_POINT('Ctrl Pts',(74.5968874696183,3.36192360377817,53.3347168548118));
#43008=CARTESIAN_POINT('Ctrl Pts',(76.8165950932171,5.51017981513921,53.1981540011394));
#43009=CARTESIAN_POINT('Ctrl Pts',(79.7864084401088,6.36007322196442,53.0615911474669));
#43010=CARTESIAN_POINT('Ctrl Pts',(82.8065504208398,5.71134182197275,52.9250282937945));
#43011=CARTESIAN_POINT('Ctrl Pts',(85.1653847950113,3.71684696339025,52.7884654401221));
#43012=CARTESIAN_POINT('Ctrl Pts',(86.3070993591023,0.846551199044585,52.6519025864497));
#43013=CARTESIAN_POINT('Ctrl Pts',(85.9626718510223,-2.22321740518142,52.5153397327772));
#43014=CARTESIAN_POINT('Ctrl Pts',(84.2132597448983,-4.769129230128,52.3787768791048));
#43015=CARTESIAN_POINT('Ctrl Pts',(81.4710770800909,-6.19129093756104,52.2422140254323));
#43016=CARTESIAN_POINT('Ctrl Pts',(78.3822644661494,-6.15459852582288,52.1056511717599));
#43017=CARTESIAN_POINT('Ctrl Pts',(75.6746389387688,-4.66769782144369,51.9690883180875));
#43018=CARTESIAN_POINT('Ctrl Pts',(73.9861984066626,-2.0809472989457,51.832525464415));
#43019=CARTESIAN_POINT('Ctrl Pts',(73.7147901779535,0.996136917128858,51.6959626107427));
#43020=CARTESIAN_POINT('Ctrl Pts',(74.9243661842076,3.83850135239988,51.5593997570702));
#43021=CARTESIAN_POINT('Ctrl Pts',(77.3299139839692,5.77639956476208,51.4228369033978));
#43022=CARTESIAN_POINT('Ctrl Pts',(80.3646142555919,6.35320452285083,51.2862740497253));
#43023=CARTESIAN_POINT('Ctrl Pts',(83.3134004559793,5.43300365203046,51.1497111960529));
#43024=CARTESIAN_POINT('Ctrl Pts',(85.481449977994,3.23262391926018,51.0131483423805));
#43025=CARTESIAN_POINT('Ctrl Pts',(86.3579052283988,0.270540886612342,50.8765854887081));
#43026=CARTESIAN_POINT('Ctrl Pts',(85.736247022437,-2.75528970567801,50.7400226350356));
#43027=CARTESIAN_POINT('Ctrl Pts',(83.7629567073689,-5.13189127740411,50.6034597813632));
#43028=CARTESIAN_POINT('Ctrl Pts',(80.903000756919,-6.2992651077435,50.4668969276907));
#43029=CARTESIAN_POINT('Ctrl Pts',(77.8302707029787,-5.98234285562748,50.3303340740183));
#43030=CARTESIAN_POINT('Ctrl Pts',(75.2687940477242,-4.25580092365468,50.1937712203459));
#43031=CARTESIAN_POINT('Ctrl Pts',(73.8221316351055,-1.52646445443898,50.0572083666734));
#43032=CARTESIAN_POINT('Ctrl Pts',(73.8311605857006,1.56255289357405,49.920645513001));
#43033=CARTESIAN_POINT('Ctrl Pts',(75.2937534075295,4.28338584247207,49.7840826593286));
#43034=CARTESIAN_POINT('Ctrl Pts',(77.8652792970721,5.99492441863291,49.6475198056562));
#43035=CARTESIAN_POINT('Ctrl Pts',(80.939809508912,6.2938787207563,49.5109569519837));
#43036=CARTESIAN_POINT('Ctrl Pts',(83.792892369597,5.10980613499994,49.3743940983113));
#43037=CARTESIAN_POINT('Ctrl Pts',(85.7522558536446,2.72170973082036,49.2378312446388));
#43038=CARTESIAN_POINT('Ctrl Pts',(86.3562150670656,-0.307703243139823,
49.1012683909664));
#43039=CARTESIAN_POINT('Ctrl Pts',(85.4624590769004,-3.26461208994559,48.964705537294));
#43040=CARTESIAN_POINT('Ctrl Pts',(83.2815836418895,-5.45228026296463,48.8281426836216));
#43041=CARTESIAN_POINT('Ctrl Pts',(80.3274685256469,-6.35522742546172,48.6915798299491));
#43042=CARTESIAN_POINT('Ctrl Pts',(77.2961919879637,-5.76069210240215,48.5550169762767));
#43043=CARTESIAN_POINT('Ctrl Pts',(74.9020138373674,-3.80876467509304,48.4184541226043));
#43044=CARTESIAN_POINT('Ctrl Pts',(73.7090743646455,-0.959377879184771,
48.2818912689318));
#43045=CARTESIAN_POINT('Ctrl Pts',(73.9984659441751,2.1160671637272,48.1453284152594));
#43046=CARTESIAN_POINT('Ctrl Pts',(75.701999226811,4.69290321850953,48.008765561587));
#43047=CARTESIAN_POINT('Ctrl Pts',(78.4182705988775,6.16395030530382,47.8722027079146));
#43048=CARTESIAN_POINT('Ctrl Pts',(81.507244931279,6.18258554180725,47.7356398542421));
#43049=CARTESIAN_POINT('Ctrl Pts',(84.2410670818731,4.74441790651735,47.5990770005697));
#43050=CARTESIAN_POINT('Ctrl Pts',(85.9755664309368,2.18832289529958,47.4625141468972));
#43051=CARTESIAN_POINT('Ctrl Pts',(86.3020428293569,-0.88340672488984,47.3259512932248));
#43052=CARTESIAN_POINT('Ctrl Pts',(85.1435686306702,-3.74697918411825,47.1893884395524));
#43053=CARTESIAN_POINT('Ctrl Pts',(82.7731151553917,-5.72765079239012,47.05282558588));
#43054=CARTESIAN_POINT('Ctrl Pts',(79.7492324481405,-6.35871582157629,46.9162627322075));
#43055=CARTESIAN_POINT('Ctrl Pts',(76.7844381088919,-5.49147639429357,46.7796998785351));
#43056=CARTESIAN_POINT('Ctrl Pts',(74.5773267431693,-3.33028017053867,46.6431370248627));
#43057=CARTESIAN_POINT('Ctrl Pts',(73.6479600879612,-0.384369900611591,
46.5065741711902));
#43058=CARTESIAN_POINT('Ctrl Pts',(74.2153248443979,2.65210946395323,46.3700113175178));
#43059=CARTESIAN_POINT('Ctrl Pts',(76.1457328328429,5.06367217232759,46.2334484638453));
#43060=CARTESIAN_POINT('Ctrl Pts',(78.9843219438627,6.2820816096985,46.0968856101729));
#43061=CARTESIAN_POINT('Ctrl Pts',(82.0622353147722,6.02024391292702,45.9603227565005));
#43062=CARTESIAN_POINT('Ctrl Pts',(84.6542240982161,4.33985590869289,45.8237599028281));
#43063=CARTESIAN_POINT('Ctrl Pts',(86.149537876292,1.63686748781935,45.6871970491556));
#43064=CARTESIAN_POINT('Ctrl Pts',(86.1958358052853,-1.45181608290028,45.5506341954832));
#43065=CARTESIAN_POINT('Ctrl Pts',(84.7822087023876,-4.19840817351866,45.4140713418108));
#43066=CARTESIAN_POINT('Ctrl Pts',(82.2417495768579,-5.95572918282979,45.2775084881383));
#43067=CARTESIAN_POINT('Ctrl Pts',(79.1730669113078,-6.30970149306707,45.140945634466));
#43068=CARTESIAN_POINT('Ctrl Pts',(76.2992345216118,-5.17691859491353,45.0043827807935));
#43069=CARTESIAN_POINT('Ctrl Pts',(74.2974136456185,-2.82429816691486,44.867819927121));
#43070=CARTESIAN_POINT('Ctrl Pts',(73.6392934141531,0.193811748307269,44.7312570734486));
#43071=CARTESIAN_POINT('Ctrl Pts',(74.4799467231356,3.16625379319216,44.5946942197762));
#43072=CARTESIAN_POINT('Ctrl Pts',(76.621290400294,5.39263133473806,44.4581313661038));
#43073=CARTESIAN_POINT('Ctrl Pts',(79.5587595524336,6.34834294257372,44.3215685124313));
#43074=CARTESIAN_POINT('Ctrl Pts',(82.6001982072725,5.80819426108823,44.1850056587589));
#43075=CARTESIAN_POINT('Ctrl Pts',(85.0289520597644,3.89946052862007,44.0484428050865));
#43076=CARTESIAN_POINT('Ctrl Pts',(86.272733737581,1.07189678402622,43.911879951414));
#43077=CARTESIAN_POINT('Ctrl Pts',(86.0384709317063,-2.00823809264104,43.7753170977416));
#43078=CARTESIAN_POINT('Ctrl Pts',(84.3813629617958,-4.61517164026814,43.6387542440692));
#43079=CARTESIAN_POINT('Ctrl Pts',(81.6918743166977,-6.13463234755794,43.5021913903967));
#43080=CARTESIAN_POINT('Ctrl Pts',(78.6037291538527,-6.20858889925048,43.3656285367243));
#43081=CARTESIAN_POINT('Ctrl Pts',(75.8445875723747,-4.81961646710041,43.2290656830519));
#43082=CARTESIAN_POINT('Ctrl Pts',(74.0645854971062,-2.29499535722046,43.0925028293794));
#43083=CARTESIAN_POINT('Ctrl Pts',(73.6831464071548,0.770390772189351,42.955939975707));
#43084=CARTESIAN_POINT('Ctrl Pts',(74.7901455575896,3.65425999548639,42.8193771220346));
#43085=CARTESIAN_POINT('Ctrl Pts',(77.1247475918389,5.6770538401786,42.6828142683621));
#43086=CARTESIAN_POINT('Ctrl Pts',(80.1368351706977,6.36221026869802,42.5462514146897));
#43087=CARTESIAN_POINT('Ctrl Pts',(83.1167004331651,5.54813947205128,42.4096885610173));
#43088=CARTESIAN_POINT('Ctrl Pts',(85.3621237298141,3.42697795347734,42.2731257073449));
#43089=CARTESIAN_POINT('Ctrl Pts',(86.3441251020869,0.497881335996617,42.1365628536724));
#43090=CARTESIAN_POINT('Ctrl Pts',(86.0018547597101,-1.53226660829892,42.0455209512241));
#43091=CARTESIAN_POINT('Ctrl Pts',(85.6017891526601,-2.4478120539861,42.));
#43092=CARTESIAN_POINT('Ctrl Pts',(85.6017891526601,-2.4478120539861,42.));
#43093=CARTESIAN_POINT('Ctrl Pts',(85.6569254810043,-2.28851462898893,42.));
#43094=CARTESIAN_POINT('Ctrl Pts',(85.705210066224,-2.12723744746175,42.));
#43095=CARTESIAN_POINT('Ctrl Pts',(85.7466571421988,-1.96442654482131,42.));
#43096=CARTESIAN_POINT('Ctrl Pts',(85.788432837758,-1.80032477063183,42.));
#43097=CARTESIAN_POINT('Ctrl Pts',(85.8232622239843,-1.63466409832166,42.));
#43098=CARTESIAN_POINT('Ctrl Pts',(85.851107925251,-1.46789149284502,42.));
#43099=CARTESIAN_POINT('Ctrl Pts',(85.8787722019253,-1.30220546987841,42.));
#43100=CARTESIAN_POINT('Ctrl Pts',(85.8995434395036,-1.13542121242627,42.));
#43101=CARTESIAN_POINT('Ctrl Pts',(85.9133341464194,-0.967978688103236,
42.));
#43102=CARTESIAN_POINT('Ctrl Pts',(85.926960703886,-0.80252921593562,42.));
#43103=CARTESIAN_POINT('Ctrl Pts',(85.9337718247844,-0.636436380822634,
42.));
#43104=CARTESIAN_POINT('Ctrl Pts',(85.9336345128749,-0.470136750206304,
42.));
#43105=CARTESIAN_POINT('Ctrl Pts',(85.9335702448832,-0.392301234639418,
42.));
#43106=CARTESIAN_POINT('Ctrl Pts',(85.9319831293793,-0.314420653493014,
42.));
#43107=CARTESIAN_POINT('Ctrl Pts',(85.9288558891231,-0.236541327327588,
42.));
#43108=CARTESIAN_POINT('Ctrl Pts',(85.9277529940179,-0.209075344356874,
42.));
#43109=CARTESIAN_POINT('Ctrl Pts',(85.9264585191432,-0.181609528300492,
42.));
#43110=CARTESIAN_POINT('Ctrl Pts',(85.9249716376403,-0.154145948317355,
42.));
#43111=CARTESIAN_POINT('Ctrl Pts',(85.9237407875316,-0.131411419477627,
42.));
#43112=CARTESIAN_POINT('Ctrl Pts',(85.922378510943,-0.108686724224631,42.));
#43113=CARTESIAN_POINT('Ctrl Pts',(85.9208851246716,-0.0859796899287691,
42.));
#43114=CARTESIAN_POINT('Ctrl Pts',(85.9100466443096,0.0788201009962529,
42.));
#43115=CARTESIAN_POINT('Ctrl Pts',(85.892300375058,0.242802290608795,42.));
#43116=CARTESIAN_POINT('Ctrl Pts',(85.8675999298121,0.405551851065137,42.));
#43117=CARTESIAN_POINT('Ctrl Pts',(85.8648424370719,0.423720783931401,42.));
#43118=CARTESIAN_POINT('Ctrl Pts',(85.8619982222532,0.441874346367681,42.));
#43119=CARTESIAN_POINT('Ctrl Pts',(85.8590671810102,0.46001195351897,42.));
#43120=CARTESIAN_POINT('Ctrl Pts',(85.8327238923556,0.623027135182727,42.));
#43121=CARTESIAN_POINT('Ctrl Pts',(85.7993709501763,0.784754959977138,42.));
#43122=CARTESIAN_POINT('Ctrl Pts',(85.7591902245475,0.944778915634052,42.));
#43123=CARTESIAN_POINT('Ctrl Pts',(85.7190590371889,1.10460557993238,42.));
#43124=CARTESIAN_POINT('Ctrl Pts',(85.6721165102442,1.26273325668429,42.));
#43125=CARTESIAN_POINT('Ctrl Pts',(85.6184980647307,1.4187228208717,42.));
#43126=CARTESIAN_POINT('Ctrl Pts',(85.5685831655387,1.56393783590737,42.));
#43127=CARTESIAN_POINT('Ctrl Pts',(85.5128820688434,1.70730010798767,42.));
#43128=CARTESIAN_POINT('Ctrl Pts',(85.451472575904,1.84842874304492,42.));
#43129=CARTESIAN_POINT('Ctrl Pts',(85.4364074129714,1.88305084754089,42.));
#43130=CARTESIAN_POINT('Ctrl Pts',(85.4209985669166,1.91753838332473,42.));
#43131=CARTESIAN_POINT('Ctrl Pts',(85.4052469350423,1.95188543849552,42.));
#43132=CARTESIAN_POINT('Ctrl Pts',(85.3941405753051,1.97610329437745,42.));
#43133=CARTESIAN_POINT('Ctrl Pts',(85.3828637956616,2.00025130705317,42.));
#43134=CARTESIAN_POINT('Ctrl Pts',(85.3714168828596,2.02432736674011,42.));
#43135=CARTESIAN_POINT('Ctrl Pts',(85.3626888510097,2.04268485922774,42.));
#43136=CARTESIAN_POINT('Ctrl Pts',(85.3538640990633,2.06099584588555,42.));
#43137=CARTESIAN_POINT('Ctrl Pts',(85.3449464057949,2.07925244694918,42.));
#43138=CARTESIAN_POINT('Ctrl Pts',(85.2740289091692,2.2244371270408,42.));
#43139=CARTESIAN_POINT('Ctrl Pts',(85.1971721039349,2.3663221572068,42.));
#43140=CARTESIAN_POINT('Ctrl Pts',(85.1145485353578,2.50451868546955,42.));
#43141=CARTESIAN_POINT('Ctrl Pts',(85.0325534073232,2.64166408143795,42.));
#43142=CARTESIAN_POINT('Ctrl Pts',(84.9448784824779,2.77517746393529,42.));
#43143=CARTESIAN_POINT('Ctrl Pts',(84.8516514430892,2.90464835133629,42.));
#43144=CARTESIAN_POINT('Ctrl Pts',(84.8193995921606,2.94943874463242,42.));
#43145=CARTESIAN_POINT('Ctrl Pts',(84.7864829254346,2.99374501823486,42.));
#43146=CARTESIAN_POINT('Ctrl Pts',(84.752905714703,3.03754912324718,42.));
#43147=CARTESIAN_POINT('Ctrl Pts',(84.65510697225,3.16513525357588,42.));
#43148=CARTESIAN_POINT('Ctrl Pts',(84.5517063684955,3.28846448836943,42.));
#43149=CARTESIAN_POINT('Ctrl Pts',(84.4430292319423,3.40721711979787,42.));
#43150=CARTESIAN_POINT('Ctrl Pts',(84.3801478011414,3.47592830977242,42.));
#43151=CARTESIAN_POINT('Ctrl Pts',(84.3154993362663,3.54310650462682,42.));
#43152=CARTESIAN_POINT('Ctrl Pts',(84.2491434596823,3.60868251821583,42.));
#43153=CARTESIAN_POINT('Ctrl Pts',(84.2089699962351,3.64838383361632,42.));
#43154=CARTESIAN_POINT('Ctrl Pts',(84.1681706577425,3.68749778106476,42.));
#43155=CARTESIAN_POINT('Ctrl Pts',(84.1267583557391,3.726007975968,42.));
#43156=CARTESIAN_POINT('Ctrl Pts',(84.1075910362983,3.74383208068396,42.));
#43157=CARTESIAN_POINT('Ctrl Pts',(84.088292403684,3.76152683711411,42.));
#43158=CARTESIAN_POINT('Ctrl Pts',(84.0688637244686,3.77909056167488,42.));
#43159=CARTESIAN_POINT('Ctrl Pts',(84.0541228012848,3.79241650687679,42.));
#43160=CARTESIAN_POINT('Ctrl Pts',(84.0393144271957,3.80566031870826,42.));
#43161=CARTESIAN_POINT('Ctrl Pts',(84.0244399044793,3.81882101986992,42.));
#43162=CARTESIAN_POINT('Ctrl Pts',(83.9064001150324,3.92326043105106,42.));
#43163=CARTESIAN_POINT('Ctrl Pts',(83.7841852346065,4.02248016159722,42.));
#43164=CARTESIAN_POINT('Ctrl Pts',(83.6581398297667,4.1162287172709,42.));
#43165=CARTESIAN_POINT('Ctrl Pts',(83.5324837634402,4.20968769536464,42.));
#43166=CARTESIAN_POINT('Ctrl Pts',(83.4030201308865,4.2977096203736,42.));
#43167=CARTESIAN_POINT('Ctrl Pts',(83.2700643854091,4.38000074382011,42.));
#43168=CARTESIAN_POINT('Ctrl Pts',(83.1392403663464,4.46097246462693,42.));
#43169=CARTESIAN_POINT('Ctrl Pts',(83.0050346764522,4.53639592031169,42.));
#43170=CARTESIAN_POINT('Ctrl Pts',(82.8677324475143,4.60594364255217,42.));
#43171=CARTESIAN_POINT('Ctrl Pts',(82.7949213954891,4.64282463757642,42.));
#43172=CARTESIAN_POINT('Ctrl Pts',(82.721239345296,4.67805245546147,42.));
#43173=CARTESIAN_POINT('Ctrl Pts',(82.6467279335914,4.71157233605123,42.));
#43174=CARTESIAN_POINT('Ctrl Pts',(82.5480059693877,4.75598363327391,42.));
#43175=CARTESIAN_POINT('Ctrl Pts',(82.4478279782409,4.79739714128736,42.));
#43176=CARTESIAN_POINT('Ctrl Pts',(82.3463374882128,4.83575688226234,42.));
#43177=CARTESIAN_POINT('Ctrl Pts',(82.3210480836265,4.84531536413657,42.));
#43178=CARTESIAN_POINT('Ctrl Pts',(82.2956771925386,4.85468417743707,42.));
#43179=CARTESIAN_POINT('Ctrl Pts',(82.2702270542163,4.86386234007145,42.));
#43180=CARTESIAN_POINT('Ctrl Pts',(82.2479671578636,4.87188999581004,42.));
#43181=CARTESIAN_POINT('Ctrl Pts',(82.2256545985108,4.87976890597722,42.));
#43182=CARTESIAN_POINT('Ctrl Pts',(82.2032959008903,4.88749708030084,42.));
#43183=CARTESIAN_POINT('Ctrl Pts',(82.0573143762485,4.93795487930184,42.));
#43184=CARTESIAN_POINT('Ctrl Pts',(81.9092993450614,4.98201550564599,42.));
#43185=CARTESIAN_POINT('Ctrl Pts',(81.7596854975444,5.01959244081141,42.));
#43186=CARTESIAN_POINT('Ctrl Pts',(81.6253698886421,5.05332707842144,42.));
#43187=CARTESIAN_POINT('Ctrl Pts',(81.4897651591011,5.08183552641375,42.));
#43188=CARTESIAN_POINT('Ctrl Pts',(81.3531856950333,5.10501933912427,42.));
#43189=CARTESIAN_POINT('Ctrl Pts',(81.2870765067884,5.11624110697331,42.));
#43190=CARTESIAN_POINT('Ctrl Pts',(81.2207389937343,5.12621485843111,42.));
#43191=CARTESIAN_POINT('Ctrl Pts',(81.154209309988,5.13492653924264,42.));
#43192=CARTESIAN_POINT('Ctrl Pts',(81.1165245578612,5.13986114156606,42.));
#43193=CARTESIAN_POINT('Ctrl Pts',(81.0787781560059,5.14439077566049,42.));
#43194=CARTESIAN_POINT('Ctrl Pts',(81.0409767524365,5.14851261661839,42.));
#43195=CARTESIAN_POINT('Ctrl Pts',(81.0182097045005,5.15099512101801,42.));
#43196=CARTESIAN_POINT('Ctrl Pts',(80.995425948708,5.15332930886033,42.));
#43197=CARTESIAN_POINT('Ctrl Pts',(80.9726350572463,5.15551398645696,42.));
#43198=CARTESIAN_POINT('Ctrl Pts',(80.8229478859385,5.16986262263071,42.));
#43199=CARTESIAN_POINT('Ctrl Pts',(80.6728487059268,5.17777748899213,42.));
#43200=CARTESIAN_POINT('Ctrl Pts',(80.5227445915659,5.17914634612362,42.));
#43201=CARTESIAN_POINT('Ctrl Pts',(80.385433598572,5.18039853786262,42.));
#43202=CARTESIAN_POINT('Ctrl Pts',(80.2481180770058,5.17617242893916,42.));
#43203=CARTESIAN_POINT('Ctrl Pts',(80.111118248695,5.16634484417903,42.));
#43204=CARTESIAN_POINT('Ctrl Pts',(80.0029202747275,5.15858333985344,42.));
#43205=CARTESIAN_POINT('Ctrl Pts',(79.894919291723,5.14732714412843,42.));
#43206=CARTESIAN_POINT('Ctrl Pts',(79.7872818445162,5.13260507264869,42.));
#43207=CARTESIAN_POINT('Ctrl Pts',(83.8799476118145,3.36633437021264,54.));
#43208=CARTESIAN_POINT('Ctrl Pts',(83.9867208778113,3.26433819512922,54.));
#43209=CARTESIAN_POINT('Ctrl Pts',(84.0887720625524,3.15785064545971,54.));
#43210=CARTESIAN_POINT('Ctrl Pts',(84.1859774524887,3.04731119162579,54.));
#43211=CARTESIAN_POINT('Ctrl Pts',(84.2849060809427,2.93481211554574,54.));
#43212=CARTESIAN_POINT('Ctrl Pts',(84.3788160767822,2.81811580143815,54.));
#43213=CARTESIAN_POINT('Ctrl Pts',(84.4675539561856,2.69763654749194,54.));
#43214=CARTESIAN_POINT('Ctrl Pts',(84.5575854668602,2.57540093277315,54.));
#43215=CARTESIAN_POINT('Ctrl Pts',(84.6422935095527,2.44927079503114,54.));
#43216=CARTESIAN_POINT('Ctrl Pts',(84.7214863046654,2.31963561596069,54.));
#43217=CARTESIAN_POINT('Ctrl Pts',(84.8005661343855,2.19018535635012,54.));
#43218=CARTESIAN_POINT('Ctrl Pts',(84.8741469255614,2.0572394347727,54.));
#43219=CARTESIAN_POINT('Ctrl Pts',(84.9419988953608,1.92115133237301,54.));
#43220=CARTESIAN_POINT('Ctrl Pts',(84.9589203834966,1.88721255038936,54.));
#43221=CARTESIAN_POINT('Ctrl Pts',(84.9754853611401,1.85307820023649,54.));
#43222=CARTESIAN_POINT('Ctrl Pts',(84.991689831896,1.81875350067991,54.));
#43223=CARTESIAN_POINT('Ctrl Pts',(85.0049215662956,1.79072572274637,54.));
#43224=CARTESIAN_POINT('Ctrl Pts',(85.0179129290737,1.76257102716215,54.));
#43225=CARTESIAN_POINT('Ctrl Pts',(85.0306616523005,1.73429221126858,54.));
#43226=CARTESIAN_POINT('Ctrl Pts',(85.0386661539721,1.71653687804293,54.));
#43227=CARTESIAN_POINT('Ctrl Pts',(85.0465747847197,1.69873297209936,54.));
#43228=CARTESIAN_POINT('Ctrl Pts',(85.0543816393726,1.68089376031065,54.));
#43229=CARTESIAN_POINT('Ctrl Pts',(85.116794780348,1.53827534485887,54.));
#43230=CARTESIAN_POINT('Ctrl Pts',(85.1727981491917,1.39320033760763,54.));
#43231=CARTESIAN_POINT('Ctrl Pts',(85.2222276344322,1.24609759053344,54.));
#43232=CARTESIAN_POINT('Ctrl Pts',(85.2279053057752,1.22920077181355,54.));
#43233=CARTESIAN_POINT('Ctrl Pts',(85.2334962056225,1.21227715721916,54.));
#43234=CARTESIAN_POINT('Ctrl Pts',(85.239000055387,1.19532736479374,54.));
#43235=CARTESIAN_POINT('Ctrl Pts',(85.2863939183891,1.04937204724304,54.));
#43236=CARTESIAN_POINT('Ctrl Pts',(85.3273366473861,0.901478132634383,54.));
#43237=CARTESIAN_POINT('Ctrl Pts',(85.361892379472,0.75208834072346,54.));
#43238=CARTESIAN_POINT('Ctrl Pts',(85.3968699097081,0.600875049958123,54.));
#43239=CARTESIAN_POINT('Ctrl Pts',(85.4253037941124,0.448128478050284,54.));
#43240=CARTESIAN_POINT('Ctrl Pts',(85.4472134338793,0.294282568467623,54.));
#43241=CARTESIAN_POINT('Ctrl Pts',(85.4680624160397,0.147884423247048,54.));
#43242=CARTESIAN_POINT('Ctrl Pts',(85.4830033161768,0.000490076344759782,
54.));
#43243=CARTESIAN_POINT('Ctrl Pts',(85.4920112832216,-0.147538780000658,
54.));
#43244=CARTESIAN_POINT('Ctrl Pts',(85.494164608261,-0.182924593618131,54.));
#43245=CARTESIAN_POINT('Ctrl Pts',(85.4959787192161,-0.218346695891146,
54.));
#43246=CARTESIAN_POINT('Ctrl Pts',(85.4974529220841,-0.25380018882677,54.));
#43247=CARTESIAN_POINT('Ctrl Pts',(85.4983096377735,-0.27440357001597,54.));
#43248=CARTESIAN_POINT('Ctrl Pts',(85.4990515565517,-0.29501755266055,54.));
#43249=CARTESIAN_POINT('Ctrl Pts',(85.4996785205849,-0.315641176049658,
54.));
#43250=CARTESIAN_POINT('Ctrl Pts',(85.5002766428774,-0.335316066873864,
54.));
#43251=CARTESIAN_POINT('Ctrl Pts',(85.5007698615858,-0.354990703538879,
54.));
#43252=CARTESIAN_POINT('Ctrl Pts',(85.5011582956561,-0.374662168734253,
54.));
#43253=CARTESIAN_POINT('Ctrl Pts',(85.5042977154338,-0.533651792992443,
54.));
#43254=CARTESIAN_POINT('Ctrl Pts',(85.5005974827858,-0.692475378903122,
54.));
#43255=CARTESIAN_POINT('Ctrl Pts',(85.4901267378284,-0.850671112988953,
54.));
#43256=CARTESIAN_POINT('Ctrl Pts',(85.4795441308475,-1.01055689825874,54.));
#43257=CARTESIAN_POINT('Ctrl Pts',(85.4620457764301,-1.1698020853449,54.));
#43258=CARTESIAN_POINT('Ctrl Pts',(85.4376534301819,-1.32794813514256,54.));
#43259=CARTESIAN_POINT('Ctrl Pts',(85.4300871316483,-1.37700369595264,54.));
#43260=CARTESIAN_POINT('Ctrl Pts',(85.4218571333759,-1.42595358576316,54.));
#43261=CARTESIAN_POINT('Ctrl Pts',(85.4129630820678,-1.4747842949477,54.));
#43262=CARTESIAN_POINT('Ctrl Pts',(85.3844600874515,-1.63127332258914,54.));
#43263=CARTESIAN_POINT('Ctrl Pts',(85.3491410875078,-1.78653855181248,54.));
#43264=CARTESIAN_POINT('Ctrl Pts',(85.3072293605156,-1.9402107254356,54.));
#43265=CARTESIAN_POINT('Ctrl Pts',(85.2815881273281,-2.03422603621094,54.));
#43266=CARTESIAN_POINT('Ctrl Pts',(85.2534782669258,-2.12764507941347,54.));
#43267=CARTESIAN_POINT('Ctrl Pts',(85.2229414321389,-2.2203819677405,54.));
#43268=CARTESIAN_POINT('Ctrl Pts',(85.2062836803499,-2.27096966218257,54.));
#43269=CARTESIAN_POINT('Ctrl Pts',(85.1889036183782,-2.32135434404811,54.));
#43270=CARTESIAN_POINT('Ctrl Pts',(85.1708071415319,-2.37152182596523,54.));
#43271=CARTESIAN_POINT('Ctrl Pts',(85.1621804631312,-2.3954369082408,54.));
#43272=CARTESIAN_POINT('Ctrl Pts',(85.1533909724132,-2.41930262938926,54.));
#43273=CARTESIAN_POINT('Ctrl Pts',(85.144439260286,-2.44311743472982,54.));
#43274=CARTESIAN_POINT('Ctrl Pts',(85.1369936391982,-2.46292549092338,54.));
#43275=CARTESIAN_POINT('Ctrl Pts',(85.1294387812218,-2.48269031816802,54.));
#43276=CARTESIAN_POINT('Ctrl Pts',(85.121776982974,-2.50240686339091,54.));
#43277=CARTESIAN_POINT('Ctrl Pts',(85.0627970435496,-2.65418332699488,54.));
#43278=CARTESIAN_POINT('Ctrl Pts',(84.9974542852625,-2.80317877950254,54.));
#43279=CARTESIAN_POINT('Ctrl Pts',(84.9260417665538,-2.94901892145395,54.));
#43280=CARTESIAN_POINT('Ctrl Pts',(84.8539555738348,-3.09623485458405,54.));
#43281=CARTESIAN_POINT('Ctrl Pts',(84.7756843890024,-3.24023637487642,54.));
#43282=CARTESIAN_POINT('Ctrl Pts',(84.6914762047118,-3.38063566136618,54.));
#43283=CARTESIAN_POINT('Ctrl Pts',(84.6071559667504,-3.52122177358501,54.));
#43284=CARTESIAN_POINT('Ctrl Pts',(84.5168826728383,-3.65819679106705,54.));
#43285=CARTESIAN_POINT('Ctrl Pts',(84.4208552373469,-3.79115765968197,54.));
#43286=CARTESIAN_POINT('Ctrl Pts',(84.3666732455324,-3.86617876857727,54.));
#43287=CARTESIAN_POINT('Ctrl Pts',(84.3106584773921,-3.93992162294824,54.));
#43288=CARTESIAN_POINT('Ctrl Pts',(84.2528400935798,-4.01231054808743,54.));
#43289=CARTESIAN_POINT('Ctrl Pts',(84.1767127434739,-4.10762239675047,54.));
#43290=CARTESIAN_POINT('Ctrl Pts',(84.0974590287316,-4.2005874878607,54.));
#43291=CARTESIAN_POINT('Ctrl Pts',(84.0152183541386,-4.29110409180728,54.));
#43292=CARTESIAN_POINT('Ctrl Pts',(83.9998522812934,-4.30801646195529,54.));
#43293=CARTESIAN_POINT('Ctrl Pts',(83.9843818987029,-4.32484332582238,54.));
#43294=CARTESIAN_POINT('Ctrl Pts',(83.9688080694945,-4.34158397855754,54.));
#43295=CARTESIAN_POINT('Ctrl Pts',(83.9526295296066,-4.35897464814822,54.));
#43296=CARTESIAN_POINT('Ctrl Pts',(83.9363458803576,-4.37626524708654,54.));
#43297=CARTESIAN_POINT('Ctrl Pts',(83.9199606112101,-4.39345287359883,54.));
#43298=CARTESIAN_POINT('Ctrl Pts',(83.8056108457966,-4.51340214278705,54.));
#43299=CARTESIAN_POINT('Ctrl Pts',(83.686281282956,-4.62837513484254,54.));
#43300=CARTESIAN_POINT('Ctrl Pts',(83.5623913145015,-4.73816763663545,54.));
#43301=CARTESIAN_POINT('Ctrl Pts',(83.4420179244782,-4.8448437122275,54.));
#43302=CARTESIAN_POINT('Ctrl Pts',(83.3173386901459,-4.94662952648338,54.));
#43303=CARTESIAN_POINT('Ctrl Pts',(83.1886992789893,-5.0433133030905,54.));
#43304=CARTESIAN_POINT('Ctrl Pts',(83.1301826943935,-5.08729363805938,54.));
#43305=CARTESIAN_POINT('Ctrl Pts',(83.0708461719817,-5.13021787326625,54.));
#43306=CARTESIAN_POINT('Ctrl Pts',(83.0107200033352,-5.17206406404072,54.));
#43307=CARTESIAN_POINT('Ctrl Pts',(82.9801270201334,-5.19335595474724,54.));
#43308=CARTESIAN_POINT('Ctrl Pts',(82.9493295839171,-5.2143687281097,54.));
#43309=CARTESIAN_POINT('Ctrl Pts',(82.9183315612049,-5.23509935358629,54.));
#43310=CARTESIAN_POINT('Ctrl Pts',(82.889668794743,-5.25426822387709,54.));
#43311=CARTESIAN_POINT('Ctrl Pts',(82.8608313052831,-5.27319782388591,54.));
#43312=CARTESIAN_POINT('Ctrl Pts',(82.8318448455755,-5.29187134074881,54.));
#43313=CARTESIAN_POINT('Ctrl Pts',(82.6883558129876,-5.38430915125419,54.));
#43314=CARTESIAN_POINT('Ctrl Pts',(82.5411173174573,-5.47054475376944,54.));
#43315=CARTESIAN_POINT('Ctrl Pts',(82.39054444323,-5.55034300499343,54.));
#43316=CARTESIAN_POINT('Ctrl Pts',(82.242702024046,-5.62869421246123,54.));
#43317=CARTESIAN_POINT('Ctrl Pts',(82.0916444097254,-5.70083979834345,54.));
#43318=CARTESIAN_POINT('Ctrl Pts',(81.9377302789933,-5.76652227351167,54.));
#43319=CARTESIAN_POINT('Ctrl Pts',(81.8197903384035,-5.81685285188211,54.));
#43320=CARTESIAN_POINT('Ctrl Pts',(81.700172382812,-5.86338783920109,54.));
#43321=CARTESIAN_POINT('Ctrl Pts',(81.5790669755173,-5.90611323035059,54.));
#43322=CARTESIAN_POINT('Ctrl Pts',(74.8634535980369,0.000107814451578703,
51.1759584946969));
#43323=CARTESIAN_POINT('Ctrl Pts',(74.8639092161186,-0.570355406205201,
51.2068866386484));
#43324=CARTESIAN_POINT('Ctrl Pts',(74.9587810459553,-1.14096646897359,51.2378147825999));
#43325=CARTESIAN_POINT('Ctrl Pts',(75.1452601228757,-1.67987880496399,51.2687429265514));
#43326=CARTESIAN_POINT('Ctrl Pts',(75.4197255087757,-2.47306581932794,51.3142638777755));
#43327=CARTESIAN_POINT('Ctrl Pts',(75.89263800231,-3.19758446033676,51.3597848289997));
#43328=CARTESIAN_POINT('Ctrl Pts',(76.5082814088742,-3.76807555044598,51.4053057802238));
#43329=CARTESIAN_POINT('Ctrl Pts',(77.1239248154383,-4.33856664055521,51.450826731448));
#43330=CARTESIAN_POINT('Ctrl Pts',(77.8822991350322,-4.75503017976483,51.4963476826721));
#43331=CARTESIAN_POINT('Ctrl Pts',(78.6940564823907,-4.96840050758325,51.5418686338963));
#43332=CARTESIAN_POINT('Ctrl Pts',(79.5058138297492,-5.18177083540168,51.5873895851204));
#43333=CARTESIAN_POINT('Ctrl Pts',(80.3709542048723,-5.19204795182889,51.6329105363446));
#43334=CARTESIAN_POINT('Ctrl Pts',(81.1875510777335,-4.99802105929599,51.6784314875687));
#43335=CARTESIAN_POINT('Ctrl Pts',(82.0041479505947,-4.80399416676308,51.7239524387928));
#43336=CARTESIAN_POINT('Ctrl Pts',(82.7722013211941,-4.40566326527006,51.769473390017));
#43337=CARTESIAN_POINT('Ctrl Pts',(83.4012229665159,-3.84995771537295,51.8149943412411));
#43338=CARTESIAN_POINT('Ctrl Pts',(84.0302446118377,-3.29425216547584,51.8605152924653));
#43339=CARTESIAN_POINT('Ctrl Pts',(84.520234531882,-2.58117196717465,51.9060362436894));
#43340=CARTESIAN_POINT('Ctrl Pts',(84.8134645551446,-1.79472868292726,51.9515571949135));
#43341=CARTESIAN_POINT('Ctrl Pts',(85.1066945784073,-1.00828539867987,51.9970781461377));
#43342=CARTESIAN_POINT('Ctrl Pts',(85.2031647048884,-0.148479028486275,
52.0425990973618));
#43343=CARTESIAN_POINT('Ctrl Pts',(85.0915093037797,0.683392334134824,52.088120048586));
#43344=CARTESIAN_POINT('Ctrl Pts',(84.9798539026711,1.51526369675592,52.1336409998101));
#43345=CARTESIAN_POINT('Ctrl Pts',(84.6600729739728,2.31920005180453,52.1791619510343));
#43346=CARTESIAN_POINT('Ctrl Pts',(84.1698415161116,3.00048559910823,52.2246829022584));
#43347=CARTESIAN_POINT('Ctrl Pts',(83.6796100582504,3.68177114641193,52.2702038534825));
#43348=CARTESIAN_POINT('Ctrl Pts',(83.0189280712263,4.24040588597073,52.3157248047067));
#43349=CARTESIAN_POINT('Ctrl Pts',(82.265633811734,4.6105743038535,52.3612457559308));
#43350=CARTESIAN_POINT('Ctrl Pts',(81.5123395522418,4.98074272173626,52.406766707155));
#43351=CARTESIAN_POINT('Ctrl Pts',(80.6664330202815,5.16244481794298,52.4522876583791));
#43352=CARTESIAN_POINT('Ctrl Pts',(79.8275747198911,5.13427325239268,52.4978086096033));
#43353=CARTESIAN_POINT('Ctrl Pts',(78.9887164195008,5.10610168684238,52.5433295608274));
#43354=CARTESIAN_POINT('Ctrl Pts',(78.1569063506806,4.86805645953507,52.5888505120516));
#43355=CARTESIAN_POINT('Ctrl Pts',(77.4301442125608,4.44818309563375,52.6343714632757));
#43356=CARTESIAN_POINT('Ctrl Pts',(76.7033820744409,4.02830973173244,52.6798924144998));
#43357=CARTESIAN_POINT('Ctrl Pts',(76.0816678670215,3.42660823123714,52.725413365724));
#43358=CARTESIAN_POINT('Ctrl Pts',(75.6382489050602,2.71396759426174,52.7709343169481));
#43359=CARTESIAN_POINT('Ctrl Pts',(75.1948299430989,2.00132695728634,52.8164552681723));
#43360=CARTESIAN_POINT('Ctrl Pts',(74.9297062265958,1.17774718383084,52.8619762193964));
#43361=CARTESIAN_POINT('Ctrl Pts',(74.8741132188043,0.340259351903744,52.9074971706205));
#43362=CARTESIAN_POINT('Ctrl Pts',(74.8665978476355,0.227043101222055,52.9136509453126));
#43363=CARTESIAN_POINT('Ctrl Pts',(74.8629116778522,0.113572678934222,52.9198047200048));
#43364=CARTESIAN_POINT('Ctrl Pts',(74.8630099039127,9.58920879684522E-5,
52.9259584946969));
#43365=CARTESIAN_POINT('Ctrl Pts',(78.4211181181246,-5.90584097022479,54.));
#43366=CARTESIAN_POINT('Ctrl Pts',(77.455879038986,-5.647791608345,53.9544790487759));
#43367=CARTESIAN_POINT('Ctrl Pts',(75.6552430725963,-4.64961437394933,53.8634371463276));
#43368=CARTESIAN_POINT('Ctrl Pts',(73.9774513743918,-2.05559122386841,53.7268742926551));
#43369=CARTESIAN_POINT('Ctrl Pts',(73.7190590194211,1.02247359936586,53.5903114389827));
#43370=CARTESIAN_POINT('Ctrl Pts',(74.9405084533092,3.85979119586914,53.4537485853103));
#43371=CARTESIAN_POINT('Ctrl Pts',(77.3541911747203,5.78754789219838,53.3171857316378));
#43372=CARTESIAN_POINT('Ctrl Pts',(80.391275596298,6.35162199178929,53.1806228779654));
#43373=CARTESIAN_POINT('Ctrl Pts',(83.3361779879638,5.41904570738785,53.044060024293));
#43374=CARTESIAN_POINT('Ctrl Pts',(85.4949699527806,3.20958767782661,52.9074971706206));
#43375=CARTESIAN_POINT('Ctrl Pts',(86.3589850655242,0.243850535977484,52.7709343169481));
#43376=CARTESIAN_POINT('Ctrl Pts',(85.7246308116887,-2.7793433146957,52.6343714632757));
#43377=CARTESIAN_POINT('Ctrl Pts',(83.7413822653001,-5.14764123692896,52.4978086096033));
#43378=CARTESIAN_POINT('Ctrl Pts',(80.8765513474216,-6.30299985802483,52.3612457559308));
#43379=CARTESIAN_POINT('Ctrl Pts',(77.8051787527545,-5.9731825630531,52.2246829022584));
#43380=CARTESIAN_POINT('Ctrl Pts',(75.2509719030383,-4.23590394123515,52.0881200485859));
#43381=CARTESIAN_POINT('Ctrl Pts',(73.8157787618652,-1.5005191497456,51.9515571949136));
#43382=CARTESIAN_POINT('Ctrl Pts',(73.8377738960802,1.58843304652964,51.8149943412411));
#43383=CARTESIAN_POINT('Ctrl Pts',(75.3117746142583,4.30310269326682,51.6784314875687));
#43384=CARTESIAN_POINT('Ctrl Pts',(77.8904620590793,6.00383208915477,51.5418686338962));
#43385=CARTESIAN_POINT('Ctrl Pts',(80.9662200126132,6.28987829428071,51.4053057802239));
#43386=CARTESIAN_POINT('Ctrl Pts',(83.8143075062239,5.09384023309799,51.2687429265514));
#43387=CARTESIAN_POINT('Ctrl Pts',(85.7636295740737,2.6975403991448,51.132180072879));
#43388=CARTESIAN_POINT('Ctrl Pts',(86.354867380944,-0.334380983822473,50.9956172192065));
#43389=CARTESIAN_POINT('Ctrl Pts',(85.4487075396391,-3.28751216265552,50.8590543655341));
#43390=CARTESIAN_POINT('Ctrl Pts',(83.258668528712,-5.46600672263342,50.7224915118617));
#43391=CARTESIAN_POINT('Ctrl Pts',(80.3007893255799,-6.35654590588445,50.5859286581892));
#43392=CARTESIAN_POINT('Ctrl Pts',(77.2720351219492,-5.74929192997566,50.4493658045168));
#43393=CARTESIAN_POINT('Ctrl Pts',(74.8860713886881,-3.78733207289439,50.3128029508444));
#43394=CARTESIAN_POINT('Ctrl Pts',(73.7051028531023,-0.932963012101885,
50.1762400971719));
#43395=CARTESIAN_POINT('Ctrl Pts',(74.0074011771884,2.14124015953471,50.0396772434995));
#43396=CARTESIAN_POINT('Ctrl Pts',(75.7217357950776,4.71090282906051,49.9031143898271));
#43397=CARTESIAN_POINT('Ctrl Pts',(78.4441579740491,6.17053528166351,49.7665515361547));
#43398=CARTESIAN_POINT('Ctrl Pts',(81.5331832701364,6.17620426573987,49.6299886824822));
#43399=CARTESIAN_POINT('Ctrl Pts',(84.2609445326221,4.72657399835094,49.4934258288098));
#43400=CARTESIAN_POINT('Ctrl Pts',(85.9846992690839,2.16322091580975,49.3568629751373));
#43401=CARTESIAN_POINT('Ctrl Pts',(86.2982790838942,-0.909851995299122,
49.2203001214649));
#43402=CARTESIAN_POINT('Ctrl Pts',(85.1277951530875,-3.76853644535141,49.0837372677925));
#43403=CARTESIAN_POINT('Ctrl Pts',(82.7490486508255,-5.73924050614397,48.94717441412));
#43404=CARTESIAN_POINT('Ctrl Pts',(79.7225437079984,-6.35760710314802,48.8106115604476));
#43405=CARTESIAN_POINT('Ctrl Pts',(76.7614158020519,-5.47793049104956,48.6740487067752));
#43406=CARTESIAN_POINT('Ctrl Pts',(74.563395616688,-3.3074889041874,48.5374858531028));
#43407=CARTESIAN_POINT('Ctrl Pts',(73.6464027337136,-0.357703578130303,
48.4009229994303));
#43408=CARTESIAN_POINT('Ctrl Pts',(74.2265082218259,2.67636745596063,48.2643601457579));
#43409=CARTESIAN_POINT('Ctrl Pts',(76.1670218022879,5.07980592226054,48.1277972920855));
#43410=CARTESIAN_POINT('Ctrl Pts',(79.0107001846261,6.28628952143238,47.991234438413));
#43411=CARTESIAN_POINT('Ctrl Pts',(82.0874873209564,6.01153447605647,47.8546715847406));
#43412=CARTESIAN_POINT('Ctrl Pts',(84.6723997386214,4.32028132816605,47.7181087310682));
#43413=CARTESIAN_POINT('Ctrl Pts',(86.1563544240622,1.61104012280873,47.5815458773957));
#43414=CARTESIAN_POINT('Ctrl Pts',(86.1896870770046,-1.47781052937492,47.4449830237233));
#43415=CARTESIAN_POINT('Ctrl Pts',(84.7645435231389,-4.21844462901729,47.3084201700509));
#43416=CARTESIAN_POINT('Ctrl Pts',(82.2167303935176,-5.96508645657586,47.1718573163784));
#43417=CARTESIAN_POINT('Ctrl Pts',(79.1465889950142,-6.30617473025753,47.035294462706));
#43418=CARTESIAN_POINT('Ctrl Pts',(76.2775368648236,-5.1613388068622,46.8987316090336));
#43419=CARTESIAN_POINT('Ctrl Pts',(74.2856088680233,-2.80033641956749,46.7621687553612));
#43420=CARTESIAN_POINT('Ctrl Pts',(73.6401630760097,0.220509347236804,46.6256059016887));
#43421=CARTESIAN_POINT('Ctrl Pts',(74.4932859058703,3.18939648797121,46.4890430480163));
#43422=CARTESIAN_POINT('Ctrl Pts',(76.6439559920085,5.40676601013892,46.3524801943438));
#43423=CARTESIAN_POINT('Ctrl Pts',(79.5854108583403,6.35013904694908,46.2159173406715));
#43424=CARTESIAN_POINT('Ctrl Pts',(82.624555380254,5.79722857302948,46.079354486999));
#43425=CARTESIAN_POINT('Ctrl Pts',(85.0452758157915,3.87831690486471,45.9427916333266));
#43426=CARTESIAN_POINT('Ctrl Pts',(86.2771777145318,1.04555727349326,45.8062287796541));
#43427=CARTESIAN_POINT('Ctrl Pts',(86.0299879841389,-2.03356705891616,45.6696659259817));
#43428=CARTESIAN_POINT('Ctrl Pts',(84.3619519504042,-4.63352190610293,45.5331030723093));
#43429=CARTESIAN_POINT('Ctrl Pts',(81.6661090088627,-6.14167980625449,45.3965402186368));
#43430=CARTESIAN_POINT('Ctrl Pts',(78.5776807367317,-6.20267345467319,45.2599773649644));
#43431=CARTESIAN_POINT('Ctrl Pts',(75.8243936079491,-4.80213091560737,45.123414511292));
#43432=CARTESIAN_POINT('Ctrl Pts',(74.0550047758089,-2.27006208203801,44.9868516576196));
#43433=CARTESIAN_POINT('Ctrl Pts',(73.6864353996727,0.7969015682589,44.8502888039471));
#43434=CARTESIAN_POINT('Ctrl Pts',(74.8055314959948,3.67609127100912,44.7137259502747));
#43435=CARTESIAN_POINT('Ctrl Pts',(77.1486004080237,5.68908344454576,44.5771630966022));
#43436=CARTESIAN_POINT('Ctrl Pts',(80.1635447169054,6.36155666463022,44.4406002429298));
#43437=CARTESIAN_POINT('Ctrl Pts',(83.1399529776901,5.53505604037131,44.3040373892574));
#43438=CARTESIAN_POINT('Ctrl Pts',(85.3764939963492,3.4043299457581,44.167474535585));
#43439=CARTESIAN_POINT('Ctrl Pts',(86.3461715250332,0.471441453942473,44.0309116819125));
#43440=CARTESIAN_POINT('Ctrl Pts',(85.8205004111942,-2.57253280683391,43.8943488282401));
#43441=CARTESIAN_POINT('Ctrl Pts',(83.9233445571365,-5.0103410604769,43.7577859745677));
#43442=CARTESIAN_POINT('Ctrl Pts',(81.1017308763422,-6.26756245882339,43.6212231208953));
#43443=CARTESIAN_POINT('Ctrl Pts',(78.020516297909,-6.04795786312262,43.4846602672228));
#43444=CARTESIAN_POINT('Ctrl Pts',(75.40572755909,-4.40327273783911,43.3480974135504));
#43445=CARTESIAN_POINT('Ctrl Pts',(73.8734873761917,-1.72104424964613,43.211534559878));
#43446=CARTESIAN_POINT('Ctrl Pts',(73.784837682508,1.36671388452568,43.0749717062055));
#43447=CARTESIAN_POINT('Ctrl Pts',(75.1606667541984,4.13243333827823,42.9384088525331));
#43448=CARTESIAN_POINT('Ctrl Pts',(77.6767884766317,5.92442701100857,42.8018459988606));
#43449=CARTESIAN_POINT('Ctrl Pts',(80.7403278321772,6.32044846892683,42.6652831451882));
#43450=CARTESIAN_POINT('Ctrl Pts',(83.6294253939595,5.22718080357853,42.5287202915158));
#43451=CARTESIAN_POINT('Ctrl Pts',(85.6633177227071,2.90223574469819,42.3921574378434));
#43452=CARTESIAN_POINT('Ctrl Pts',(86.3627699345494,-0.106570534545254,
42.2555945841709));
#43453=CARTESIAN_POINT('Ctrl Pts',(85.5629461401894,-3.09025001994495,42.1190317304985));
#43454=CARTESIAN_POINT('Ctrl Pts',(83.45236018166,-5.34580695151189,41.9824688768261));
#43455=CARTESIAN_POINT('Ctrl Pts',(80.5282216380884,-6.34166017411614,41.8459060231536));
#43456=CARTESIAN_POINT('Ctrl Pts',(77.4797852514363,-5.84337786289595,41.7093431694812));
#43457=CARTESIAN_POINT('Ctrl Pts',(75.0248946938219,-3.96789034338118,41.5727803158088));
#43458=CARTESIAN_POINT('Ctrl Pts',(74.1705695184084,-2.09471758856737,41.4817384133605));
#43459=CARTESIAN_POINT('Ctrl Pts',(73.988784526404,-1.1122563070174,41.4362174621363));
#43460=CARTESIAN_POINT('Ctrl Pts',(78.5051856848936,-5.59138446414239,54.1879275126212));
#43461=CARTESIAN_POINT('Ctrl Pts',(77.5913407611158,-5.34707494069419,54.1424065613971));
#43462=CARTESIAN_POINT('Ctrl Pts',(75.8865796578611,-4.40204565375622,54.0513646589488));
#43463=CARTESIAN_POINT('Ctrl Pts',(74.2981219796566,-1.94614126789259,53.9148018052764));
#43464=CARTESIAN_POINT('Ctrl Pts',(74.0534877257849,0.968031991940416,53.7782389516039));
#43465=CARTESIAN_POINT('Ctrl Pts',(75.2099010838163,3.6542766112774,53.6416760979315));
#43466=CARTESIAN_POINT('Ctrl Pts',(77.4950672672453,5.47938990112807,53.5051132442591));
#43467=CARTESIAN_POINT('Ctrl Pts',(80.3704421269332,6.01342987494025,53.3685503905866));
#43468=CARTESIAN_POINT('Ctrl Pts',(83.1585431889481,5.13050861537382,53.2319875369142));
#43469=CARTESIAN_POINT('Ctrl Pts',(85.202390274274,3.0386931799519,53.0954246832418));
#43470=CARTESIAN_POINT('Ctrl Pts',(86.0204009018096,0.23086671403978,52.9588618295694));
#43471=CARTESIAN_POINT('Ctrl Pts',(85.4198228406087,-2.63135717819982,52.8222989758969));
#43472=CARTESIAN_POINT('Ctrl Pts',(83.5421723642892,-4.873555076111,52.6857361222245));
#43473=CARTESIAN_POINT('Ctrl Pts',(80.8298793703903,-5.9673966267179,52.549173268552));
#43474=CARTESIAN_POINT('Ctrl Pts',(77.9220420114104,-5.65514045381926,52.4126104148797));
#43475=CARTESIAN_POINT('Ctrl Pts',(75.5038339069743,-4.01036323328569,52.2760475612072));
#43476=CARTESIAN_POINT('Ctrl Pts',(74.1450576254833,-1.42062400669694,52.1394847075348));
#43477=CARTESIAN_POINT('Ctrl Pts',(74.1658816287634,1.50385692799279,52.0029218538623));
#43478=CARTESIAN_POINT('Ctrl Pts',(75.561399177798,4.07398398772421,51.8663590001899));
#43479=CARTESIAN_POINT('Ctrl Pts',(78.0027844080377,5.68415804588484,51.7297961465174));
#43480=CARTESIAN_POINT('Ctrl Pts',(80.9147736274489,5.95497372064338,51.593233292845));
#43481=CARTESIAN_POINT('Ctrl Pts',(83.6112147007152,4.82261870676202,51.4566704391726));
#43482=CARTESIAN_POINT('Ctrl Pts',(85.4567451138666,2.5539098589376,51.3201075855002));
#43483=CARTESIAN_POINT('Ctrl Pts',(86.0165024633475,-0.316576868133725,
51.1835447318278));
#43484=CARTESIAN_POINT('Ctrl Pts',(85.1585911033486,-3.1124685755383,51.0469818781553));
#43485=CARTESIAN_POINT('Ctrl Pts',(83.0851607209018,-5.17496919133383,50.9104190244829));
#43486=CARTESIAN_POINT('Ctrl Pts',(80.284773797755,-6.01809161522638,50.7738561708104));
#43487=CARTESIAN_POINT('Ctrl Pts',(77.4172856135544,-5.44317087763737,50.6372933171381));
#43488=CARTESIAN_POINT('Ctrl Pts',(75.1583625207344,-3.5856755743499,50.5007304634656));
#43489=CARTESIAN_POINT('Ctrl Pts',(74.0402746555502,-0.883287395950221,
50.3641676097932));
#43490=CARTESIAN_POINT('Ctrl Pts',(74.326477105185,2.02722982592681,50.2276047561207));
#43491=CARTESIAN_POINT('Ctrl Pts',(75.9495319752931,4.46007080503741,50.0910419024483));
#43492=CARTESIAN_POINT('Ctrl Pts',(78.5269987836753,5.84198512680619,49.9544790487759));
#43493=CARTESIAN_POINT('Ctrl Pts',(81.4515489259775,5.84735226582193,49.8179161951034));
#43494=CARTESIAN_POINT('Ctrl Pts',(84.0340705383689,4.47490756290936,49.681353341431));
#43495=CARTESIAN_POINT('Ctrl Pts',(85.6660439528304,2.04804021682049,49.5447904877586));
#43496=CARTESIAN_POINT('Ctrl Pts',(85.9629272102087,-0.861406925251295,
49.4082276340861));
#43497=CARTESIAN_POINT('Ctrl Pts',(84.8547656970158,-3.56788072000698,49.2716647804137));
#43498=CARTESIAN_POINT('Ctrl Pts',(82.602675553726,-5.43365464187376,49.1351019267412));
#43499=CARTESIAN_POINT('Ctrl Pts',(79.7373168684362,-6.01909630904101,48.9985390730689));
#43500=CARTESIAN_POINT('Ctrl Pts',(76.9338542196583,-5.18625807869333,48.8619762193964));
#43501=CARTESIAN_POINT('Ctrl Pts',(74.8528676204124,-3.13138165545505,48.725413365724));
#43502=CARTESIAN_POINT('Ctrl Pts',(73.9847000240544,-0.338657650893332,
48.5888505120515));
#43503=CARTESIAN_POINT('Ctrl Pts',(74.5339177950964,2.53386426912626,48.4522876583791));
#43504=CARTESIAN_POINT('Ctrl Pts',(76.3711087287763,4.80933165281371,48.3157248047067));
#43505=CARTESIAN_POINT('Ctrl Pts',(79.0633754539025,5.95157603200757,48.1791619510343));
#43506=CARTESIAN_POINT('Ctrl Pts',(81.9763390572716,5.69145031919123,48.0425990973618));
#43507=CARTESIAN_POINT('Ctrl Pts',(84.4236178116724,4.09024794619769,47.9060362436894));
#43508=CARTESIAN_POINT('Ctrl Pts',(85.8285593289765,1.52526029048154,47.7694733900169));
#43509=CARTESIAN_POINT('Ctrl Pts',(85.8601171847926,-1.39912450683183,47.6329105363445));
#43510=CARTESIAN_POINT('Ctrl Pts',(84.5108554003267,-3.99383354215757,47.4963476826721));
#43511=CARTESIAN_POINT('Ctrl Pts',(82.0987005823549,-5.64747542453636,47.3597848289997));
#43512=CARTESIAN_POINT('Ctrl Pts',(79.1920288644982,-5.97040245287662,47.2232219753272));
#43513=CARTESIAN_POINT('Ctrl Pts',(76.4757394167395,-4.88652331892474,47.0866591216548));
#43514=CARTESIAN_POINT('Ctrl Pts',(74.5898716273508,-2.65123250518983,46.9500962679824));
#43515=CARTESIAN_POINT('Ctrl Pts',(73.9787925969288,0.208768326907914,46.8135334143099));
#43516=CARTESIAN_POINT('Ctrl Pts',(74.7864909011902,3.01957707001274,46.6769705606375));
#43517=CARTESIAN_POINT('Ctrl Pts',(76.8226485572726,5.11888275061244,46.5404077069651));
#43518=CARTESIAN_POINT('Ctrl Pts',(79.6074856574423,6.01202588949896,46.4038448532926));
#43519=CARTESIAN_POINT('Ctrl Pts',(82.4848109274224,5.48855513410238,46.2672819996202));
#43520=CARTESIAN_POINT('Ctrl Pts',(84.7766401018847,3.67181591888614,46.1307191459478));
#43521=CARTESIAN_POINT('Ctrl Pts',(85.942949383271,0.989886575824742,45.9941562922754));
#43522=CARTESIAN_POINT('Ctrl Pts',(85.7089212702245,-1.92528977961673,45.8575934386029));
#43523=CARTESIAN_POINT('Ctrl Pts',(84.1296998161292,-4.38681002937017,45.7210305849305));
#43524=CARTESIAN_POINT('Ctrl Pts',(81.5773970336638,-5.81466606120303,45.5844677312581));
#43525=CARTESIAN_POINT('Ctrl Pts',(78.6534121267769,-5.87241210277425,45.4479048775856));
#43526=CARTESIAN_POINT('Ctrl Pts',(76.0467237728552,-4.54644145206012,45.3113420239132));
#43527=CARTESIAN_POINT('Ctrl Pts',(74.3715460501678,-2.14919262508739,45.1747791702408));
#43528=CARTESIAN_POINT('Ctrl Pts',(74.02260115069,0.754470543768118,45.0382163165683));
#43529=CARTESIAN_POINT('Ctrl Pts',(75.082110974677,3.48035778902924,44.9016534628959));
#43530=CARTESIAN_POINT('Ctrl Pts',(77.3004231810475,5.38616819305111,44.7650906092235));
#43531=CARTESIAN_POINT('Ctrl Pts',(80.1548367783535,6.02283557611966,44.6285277555511));
#43532=CARTESIAN_POINT('Ctrl Pts',(82.9727661794669,5.24034197810641,44.4919649018786));
#43533=CARTESIAN_POINT('Ctrl Pts',(85.0902225702155,3.22306639570792,44.3554020482062));
#43534=CARTESIAN_POINT('Ctrl Pts',(86.0082696182899,0.446339553438113,44.2188391945338));
#43535=CARTESIAN_POINT('Ctrl Pts',(85.5105878632297,-2.43555829595599,44.0822763408613));
#43536=CARTESIAN_POINT('Ctrl Pts',(83.7144460737851,-4.74356544763836,43.9457134871889));
#43537=CARTESIAN_POINT('Ctrl Pts',(81.0430692151556,-5.93384609185868,43.8091506335164));
#43538=CARTESIAN_POINT('Ctrl Pts',(78.1259139088411,-5.72593434299071,43.672587779844));
#43539=CARTESIAN_POINT('Ctrl Pts',(75.6503495980245,-4.1688204782118,43.5360249261716));
#43540=CARTESIAN_POINT('Ctrl Pts',(74.1996935446045,-1.629407247518,43.3994620724992));
#43541=CARTESIAN_POINT('Ctrl Pts',(74.1157640039154,1.29394320290574,43.2628992188267));
#43542=CARTESIAN_POINT('Ctrl Pts',(75.4183370558397,3.91240192264668,43.1263363651543));
#43543=CARTESIAN_POINT('Ctrl Pts',(77.8004878756186,5.60898089117325,42.9897735114819));
#43544=CARTESIAN_POINT('Ctrl Pts',(80.7009090762987,5.98391618632172,42.8532106578094));
#43545=CARTESIAN_POINT('Ctrl Pts',(83.4361766366318,4.94885955848552,42.716647804137));
#43546=CARTESIAN_POINT('Ctrl Pts',(85.3617743670875,2.74770620069144,42.5800849504646));
#43547=CARTESIAN_POINT('Ctrl Pts',(86.0239842454813,-0.100896186368019,
42.4435220967921));
#43548=CARTESIAN_POINT('Ctrl Pts',(85.2667470695425,-2.92570965573735,42.3069592431197));
#43549=CARTESIAN_POINT('Ctrl Pts',(83.2685392616698,-5.06116945709941,42.1703963894473));
#43550=CARTESIAN_POINT('Ctrl Pts',(80.5000964766443,-6.0039984742552,42.0338335357748));
#43551=CARTESIAN_POINT('Ctrl Pts',(77.6139740872696,-5.5322472050016,41.8972706821024));
#43552=CARTESIAN_POINT('Ctrl Pts',(75.2897941789012,-3.75662001961385,41.76070782843));
#43553=CARTESIAN_POINT('Ctrl Pts',(74.4809575479766,-1.98318434927916,41.6696659259817));
#43554=CARTESIAN_POINT('Ctrl Pts',(74.308851697983,-1.05303421926797,41.6241449747576));
#43555=CARTESIAN_POINT('Ctrl Pts',(78.5892532516625,-5.27692795806,54.3758550252424));
#43556=CARTESIAN_POINT('Ctrl Pts',(77.7268024832456,-5.04635827304338,54.3303340740183));
#43557=CARTESIAN_POINT('Ctrl Pts',(76.1179162431258,-4.15447693356311,54.23929217157));
#43558=CARTESIAN_POINT('Ctrl Pts',(74.6187925849215,-1.83669131191678,54.1027293178976));
#43559=CARTESIAN_POINT('Ctrl Pts',(74.3879164321487,0.913590384514973,53.9661664642252));
#43560=CARTESIAN_POINT('Ctrl Pts',(75.4792937143235,3.44876202668567,53.8296036105527));
#43561=CARTESIAN_POINT('Ctrl Pts',(77.6359433597704,5.17123191005776,53.6930407568803));
#43562=CARTESIAN_POINT('Ctrl Pts',(80.3496086575683,5.6752377580912,53.5564779032078));
#43563=CARTESIAN_POINT('Ctrl Pts',(82.9809083899325,4.84197152335979,53.4199150495354));
#43564=CARTESIAN_POINT('Ctrl Pts',(84.9098105957675,2.86779868207719,53.283352195863));
#43565=CARTESIAN_POINT('Ctrl Pts',(85.681816738095,0.217882892102075,53.1467893421906));
#43566=CARTESIAN_POINT('Ctrl Pts',(85.1150148695287,-2.48337104170394,53.0102264885181));
#43567=CARTESIAN_POINT('Ctrl Pts',(83.3429624632783,-4.59946891529305,52.8736636348457));
#43568=CARTESIAN_POINT('Ctrl Pts',(80.7832073933592,-5.63179339541097,52.7371007811733));
#43569=CARTESIAN_POINT('Ctrl Pts',(78.0389052700664,-5.33709834458541,52.6005379275009));
#43570=CARTESIAN_POINT('Ctrl Pts',(75.7566959109101,-3.78482252533623,52.4639750738284));
#43571=CARTESIAN_POINT('Ctrl Pts',(74.4743364891013,-1.34072886364829,52.327412220156));
#43572=CARTESIAN_POINT('Ctrl Pts',(74.4939893614466,1.41928080945594,52.1908493664835));
#43573=CARTESIAN_POINT('Ctrl Pts',(75.8110237413377,3.8448652821816,52.0542865128111));
#43574=CARTESIAN_POINT('Ctrl Pts',(78.115106756996,5.36448400261491,51.9177236591387));
#43575=CARTESIAN_POINT('Ctrl Pts',(80.8633272422847,5.62006914700605,51.7811608054663));
#43576=CARTESIAN_POINT('Ctrl Pts',(83.4081218952066,4.55139718042604,51.6445979517938));
#43577=CARTESIAN_POINT('Ctrl Pts',(85.1498606536595,2.41027931873041,51.5080350981214));
#43578=CARTESIAN_POINT('Ctrl Pts',(85.6781375457509,-0.298772752444985,
51.371472244449));
#43579=CARTESIAN_POINT('Ctrl Pts',(84.8684746670582,-2.93742498842107,51.2349093907766));
#43580=CARTESIAN_POINT('Ctrl Pts',(82.9116529130915,-4.88393166003425,51.0983465371041));
#43581=CARTESIAN_POINT('Ctrl Pts',(80.2687582699299,-5.67963732456832,50.9617836834317));
#43582=CARTESIAN_POINT('Ctrl Pts',(77.5625361051596,-5.13704982529907,50.8252208297592));
#43583=CARTESIAN_POINT('Ctrl Pts',(75.4306536527807,-3.3840190758054,50.6886579760868));
#43584=CARTESIAN_POINT('Ctrl Pts',(74.3754464579983,-0.833611779798555,
50.5520951224143));
#43585=CARTESIAN_POINT('Ctrl Pts',(74.6455530331815,1.91321949231889,50.4155322687419));
#43586=CARTESIAN_POINT('Ctrl Pts',(76.1773281555086,4.20923878101431,50.2789694150695));
#43587=CARTESIAN_POINT('Ctrl Pts',(78.6098395933014,5.51343497194888,50.1424065613971));
#43588=CARTESIAN_POINT('Ctrl Pts',(81.3699145818185,5.51850026590399,50.0058437077246));
#43589=CARTESIAN_POINT('Ctrl Pts',(83.8071965441157,4.22324112746778,49.8692808540522));
#43590=CARTESIAN_POINT('Ctrl Pts',(85.3473886365768,1.93285951783123,49.7327180003798));
#43591=CARTESIAN_POINT('Ctrl Pts',(85.6275753365233,-0.812961855203473,
49.5961551467073));
#43592=CARTESIAN_POINT('Ctrl Pts',(84.5817362409442,-3.36722499466254,49.4595922930349));
#43593=CARTESIAN_POINT('Ctrl Pts',(82.4563024566265,-5.12806877760354,49.3230294393625));
#43594=CARTESIAN_POINT('Ctrl Pts',(79.752090028874,-5.680585514934,49.1864665856901));
#43595=CARTESIAN_POINT('Ctrl Pts',(77.1062926372646,-4.89458566633712,49.0499037320176));
#43596=CARTESIAN_POINT('Ctrl Pts',(75.1423396241368,-2.95527440672271,48.9133408783452));
#43597=CARTESIAN_POINT('Ctrl Pts',(74.3229973143953,-0.319611723656359,
48.7767780246728));
#43598=CARTESIAN_POINT('Ctrl Pts',(74.8413273683668,2.39136108229189,48.6402151710003));
#43599=CARTESIAN_POINT('Ctrl Pts',(76.5751956552648,4.53885738336689,48.5036523173279));
#43600=CARTESIAN_POINT('Ctrl Pts',(79.1160507231789,5.61686254258275,48.3670894636555));
#43601=CARTESIAN_POINT('Ctrl Pts',(81.8651907935868,5.37136616232601,48.2305266099831));
#43602=CARTESIAN_POINT('Ctrl Pts',(84.1748358847232,3.86021456422933,48.0939637563106));
#43603=CARTESIAN_POINT('Ctrl Pts',(85.5007642338909,1.43948045815434,47.9574009026382));
#43604=CARTESIAN_POINT('Ctrl Pts',(85.5305472925806,-1.32043848428875,47.8208380489658));
#43605=CARTESIAN_POINT('Ctrl Pts',(84.2571672775145,-3.76922245529786,47.6842751952933));
#43606=CARTESIAN_POINT('Ctrl Pts',(81.9806707711923,-5.32986439249687,47.5477123416209));
#43607=CARTESIAN_POINT('Ctrl Pts',(79.2374687339821,-5.63463017549571,47.4111494879484));
#43608=CARTESIAN_POINT('Ctrl Pts',(76.6739419686554,-4.61170783098729,47.274586634276));
#43609=CARTESIAN_POINT('Ctrl Pts',(74.8941343866782,-2.50212859081217,47.1380237806036));
#43610=CARTESIAN_POINT('Ctrl Pts',(74.3174221178479,0.197027306579024,47.0014609269311));
#43611=CARTESIAN_POINT('Ctrl Pts',(75.0796958965101,2.84975765205427,46.8648980732588));
#43612=CARTESIAN_POINT('Ctrl Pts',(77.0013411225368,4.83099949108596,46.7283352195863));
#43613=CARTESIAN_POINT('Ctrl Pts',(79.6295604565443,5.67391273204884,46.5917723659139));
#43614=CARTESIAN_POINT('Ctrl Pts',(82.3450664745908,5.17988169517528,46.4552095122414));
#43615=CARTESIAN_POINT('Ctrl Pts',(84.5080043879781,3.46531493290757,46.318646658569));
#43616=CARTESIAN_POINT('Ctrl Pts',(85.6087210520102,0.934215878156226,46.1820838048966));
#43617=CARTESIAN_POINT('Ctrl Pts',(85.3878545563101,-1.8170125003173,46.0455209512241));
#43618=CARTESIAN_POINT('Ctrl Pts',(83.8974476818542,-4.14009815263742,45.9089580975517));
#43619=CARTESIAN_POINT('Ctrl Pts',(81.4886850584649,-5.48765231615157,45.7723952438793));
#43620=CARTESIAN_POINT('Ctrl Pts',(78.7291435168221,-5.54215075087533,45.6358323902069));
#43621=CARTESIAN_POINT('Ctrl Pts',(76.2690539377614,-4.29075198851288,45.4992695365344));
#43622=CARTESIAN_POINT('Ctrl Pts',(74.6880873245266,-2.02832316813677,45.362706682862));
#43623=CARTESIAN_POINT('Ctrl Pts',(74.3587669017073,0.712039519277336,45.2261438291895));
#43624=CARTESIAN_POINT('Ctrl Pts',(75.3586904533591,3.28462430704937,45.0895809755172));
#43625=CARTESIAN_POINT('Ctrl Pts',(77.4522459540714,5.08325294155646,44.9530181218447));
#43626=CARTESIAN_POINT('Ctrl Pts',(80.1461288398016,5.68411448760911,44.8164552681723));
#43627=CARTESIAN_POINT('Ctrl Pts',(82.8055793812436,4.94562791584151,44.6798924144999));
#43628=CARTESIAN_POINT('Ctrl Pts',(84.8039511440818,3.04180284565774,44.5433295608274));
#43629=CARTESIAN_POINT('Ctrl Pts',(85.6703677115467,0.421237652933754,44.406766707155));
#43630=CARTESIAN_POINT('Ctrl Pts',(85.2006753152652,-2.29858378507807,44.2702038534825));
#43631=CARTESIAN_POINT('Ctrl Pts',(83.5055475904337,-4.47678983479981,44.1336409998101));
#43632=CARTESIAN_POINT('Ctrl Pts',(80.9844075539689,-5.60012972489397,43.9970781461377));
#43633=CARTESIAN_POINT('Ctrl Pts',(78.2313115197731,-5.40391082285879,43.8605152924653));
#43634=CARTESIAN_POINT('Ctrl Pts',(75.894971636959,-3.93436821858449,43.7239524387928));
#43635=CARTESIAN_POINT('Ctrl Pts',(74.5258997130174,-1.53777024538986,43.5873895851204));
#43636=CARTESIAN_POINT('Ctrl Pts',(74.4466903253228,1.22117252128579,43.4508267314479));
#43637=CARTESIAN_POINT('Ctrl Pts',(75.6760073574809,3.69237050701514,43.3142638777755));
#43638=CARTESIAN_POINT('Ctrl Pts',(77.9241872746054,5.29353477133792,43.1777010241031));
#43639=CARTESIAN_POINT('Ctrl Pts',(80.6614903204203,5.6473839037166,43.0411381704306));
#43640=CARTESIAN_POINT('Ctrl Pts',(83.2429278793041,4.67053831339252,42.9045753167582));
#43641=CARTESIAN_POINT('Ctrl Pts',(85.060231011468,2.59317665668469,42.7680124630858));
#43642=CARTESIAN_POINT('Ctrl Pts',(85.6851985564131,-0.0952218381907853,
42.6314496094134));
#43643=CARTESIAN_POINT('Ctrl Pts',(84.9705479988958,-2.76116929152976,42.4948867557409));
#43644=CARTESIAN_POINT('Ctrl Pts',(83.0847183416795,-4.77653196268692,42.3583239020685));
#43645=CARTESIAN_POINT('Ctrl Pts',(80.4719713152003,-5.66633677439428,42.2217610483961));
#43646=CARTESIAN_POINT('Ctrl Pts',(77.7481629231028,-5.22111654710725,42.0851981947237));
#43647=CARTESIAN_POINT('Ctrl Pts',(75.5546936639805,-3.54534969584653,41.9486353410512));
#43648=CARTESIAN_POINT('Ctrl Pts',(74.7913455775449,-1.87165110999094,41.8575934386029));
#43649=CARTESIAN_POINT('Ctrl Pts',(74.6289188695621,-0.993812131518549,
41.8120724873788));
#43650=CARTESIAN_POINT('Ctrl Pts',(78.6733208184315,-4.96247145197761,54.5637825378637));
#43651=CARTESIAN_POINT('Ctrl Pts',(77.8622642053754,-4.74564160539257,54.5182615866395));
#43652=CARTESIAN_POINT('Ctrl Pts',(76.3492528283906,-3.90690821337,54.4272196841912));
#43653=CARTESIAN_POINT('Ctrl Pts',(74.9394631901864,-1.72724135594096,54.2906568305188));
#43654=CARTESIAN_POINT('Ctrl Pts',(74.7223451385125,0.85914877708953,54.1540939768464));
#43655=CARTESIAN_POINT('Ctrl Pts',(75.7486863448307,3.24324744209394,54.017531123174));
#43656=CARTESIAN_POINT('Ctrl Pts',(77.7768194522954,4.86307391898745,53.8809682695015));
#43657=CARTESIAN_POINT('Ctrl Pts',(80.3287751882034,5.33704564124216,53.7444054158291));
#43658=CARTESIAN_POINT('Ctrl Pts',(82.8032735909169,4.55343443134576,53.6078425621567));
#43659=CARTESIAN_POINT('Ctrl Pts',(84.617230917261,2.69690418420248,53.4712797084842));
#43660=CARTESIAN_POINT('Ctrl Pts',(85.3432325743804,0.204899070164371,53.3347168548118));
#43661=CARTESIAN_POINT('Ctrl Pts',(84.8102068984487,-2.33538490520805,53.1981540011394));
#43662=CARTESIAN_POINT('Ctrl Pts',(83.1437525622673,-4.32538275447508,53.0615911474669));
#43663=CARTESIAN_POINT('Ctrl Pts',(80.7365354163281,-5.29619016410404,52.9250282937945));
#43664=CARTESIAN_POINT('Ctrl Pts',(78.1557685287222,-5.01905623535157,52.7884654401221));
#43665=CARTESIAN_POINT('Ctrl Pts',(76.0095579148461,-3.55928181738677,52.6519025864496));
#43666=CARTESIAN_POINT('Ctrl Pts',(74.8036153527193,-1.26083372059963,52.5153397327772));
#43667=CARTESIAN_POINT('Ctrl Pts',(74.8220970941299,1.33470469091909,52.3787768791048));
#43668=CARTESIAN_POINT('Ctrl Pts',(76.0606483048774,3.61574657663899,52.2422140254324));
#43669=CARTESIAN_POINT('Ctrl Pts',(78.2274291059544,5.04480995934498,52.1056511717599));
#43670=CARTESIAN_POINT('Ctrl Pts',(80.8118808571204,5.28516457336873,51.9690883180875));
#43671=CARTESIAN_POINT('Ctrl Pts',(83.2050290896979,4.28017565409007,51.832525464415));
#43672=CARTESIAN_POINT('Ctrl Pts',(84.8429761934525,2.26664877852321,51.6959626107426));
#43673=CARTESIAN_POINT('Ctrl Pts',(85.3397726281543,-0.280968636756239,
51.5593997570702));
#43674=CARTESIAN_POINT('Ctrl Pts',(84.5783582307678,-2.76238140130385,51.4228369033978));
#43675=CARTESIAN_POINT('Ctrl Pts',(82.7381451052813,-4.59289412873466,51.2862740497253));
#43676=CARTESIAN_POINT('Ctrl Pts',(80.2527427421049,-5.34118303391026,51.1497111960529));
#43677=CARTESIAN_POINT('Ctrl Pts',(77.7077865967648,-4.83092877296077,51.0131483423805));
#43678=CARTESIAN_POINT('Ctrl Pts',(75.702944784827,-3.18236257726091,50.876585488708));
#43679=CARTESIAN_POINT('Ctrl Pts',(74.7106182604463,-0.783936163646889,
50.7400226350356));
#43680=CARTESIAN_POINT('Ctrl Pts',(74.9646289611781,1.79920915871098,50.6034597813632));
#43681=CARTESIAN_POINT('Ctrl Pts',(76.405124335724,3.95840675699122,50.4668969276907));
#43682=CARTESIAN_POINT('Ctrl Pts',(78.6926804029276,5.18488481709156,50.3303340740183));
#43683=CARTESIAN_POINT('Ctrl Pts',(81.2882802376596,5.18964826598606,50.1937712203459));
#43684=CARTESIAN_POINT('Ctrl Pts',(83.5803225498624,3.97157469202619,50.0572083666735));
#43685=CARTESIAN_POINT('Ctrl Pts',(85.0287333203233,1.81767881884198,49.920645513001));
#43686=CARTESIAN_POINT('Ctrl Pts',(85.2922234628379,-0.764516785155648,
49.7840826593286));
#43687=CARTESIAN_POINT('Ctrl Pts',(84.3087067848726,-3.1665692693181,49.6475198056562));
#43688=CARTESIAN_POINT('Ctrl Pts',(82.3099293595269,-4.82248291333333,49.5109569519837));
#43689=CARTESIAN_POINT('Ctrl Pts',(79.7668631893118,-5.34207472082699,49.3743940983113));
#43690=CARTESIAN_POINT('Ctrl Pts',(77.278731054871,-4.6029132539809,49.2378312446389));
#43691=CARTESIAN_POINT('Ctrl Pts',(75.4318116278612,-2.77916715799037,49.1012683909664));
#43692=CARTESIAN_POINT('Ctrl Pts',(74.6612946047361,-0.300565796419388,
48.964705537294));
#43693=CARTESIAN_POINT('Ctrl Pts',(75.1487369416373,2.24885789545753,48.8281426836216));
#43694=CARTESIAN_POINT('Ctrl Pts',(76.7792825817531,4.26838311392006,48.6915798299491));
#43695=CARTESIAN_POINT('Ctrl Pts',(79.1687259924554,5.28214905315793,48.5550169762767));
#43696=CARTESIAN_POINT('Ctrl Pts',(81.7540425299019,5.05128200546077,48.4184541226042));
#43697=CARTESIAN_POINT('Ctrl Pts',(83.9260539577742,3.63018118226098,48.2818912689319));
#43698=CARTESIAN_POINT('Ctrl Pts',(85.1729691388052,1.35370062582714,48.1453284152594));
#43699=CARTESIAN_POINT('Ctrl Pts',(85.2009774003686,-1.24175246174566,48.008765561587));
#43700=CARTESIAN_POINT('Ctrl Pts',(84.0034791547023,-3.54461136843815,47.8722027079146));
#43701=CARTESIAN_POINT('Ctrl Pts',(81.8626409600297,-5.01225336045737,47.7356398542421));
#43702=CARTESIAN_POINT('Ctrl Pts',(79.282908603466,-5.2988578981148,47.5990770005697));
#43703=CARTESIAN_POINT('Ctrl Pts',(76.8721445205713,-4.33689234304983,47.4625141468972));
#43704=CARTESIAN_POINT('Ctrl Pts',(75.1983971460056,-2.35302467643452,47.3259512932248));
#43705=CARTESIAN_POINT('Ctrl Pts',(74.6560516387671,0.185286286250136,47.1893884395524));
#43706=CARTESIAN_POINT('Ctrl Pts',(75.37290089183,2.6799382340958,47.05282558588));
#43707=CARTESIAN_POINT('Ctrl Pts',(77.180033687801,4.54311623155949,46.9162627322075));
#43708=CARTESIAN_POINT('Ctrl Pts',(79.6516352556463,5.33579957459872,46.7796998785351));
#43709=CARTESIAN_POINT('Ctrl Pts',(82.2053220217592,4.87120825624818,46.6431370248627));
#43710=CARTESIAN_POINT('Ctrl Pts',(84.2393686740714,3.25881394692901,46.5065741711902));
#43711=CARTESIAN_POINT('Ctrl Pts',(85.2744927207494,0.87854518048771,46.3700113175178));
#43712=CARTESIAN_POINT('Ctrl Pts',(85.0667878423957,-1.70873522101788,46.2334484638454));
#43713=CARTESIAN_POINT('Ctrl Pts',(83.6651955475792,-3.89338627590466,46.0968856101729));
#43714=CARTESIAN_POINT('Ctrl Pts',(81.399973083266,-5.16063857110011,45.9603227565005));
#43715=CARTESIAN_POINT('Ctrl Pts',(78.8048749068673,-5.21188939897639,45.8237599028281));
#43716=CARTESIAN_POINT('Ctrl Pts',(76.4913841026675,-4.03506252496563,45.6871970491556));
#43717=CARTESIAN_POINT('Ctrl Pts',(75.0046285988854,-1.90745371118615,45.5506341954832));
#43718=CARTESIAN_POINT('Ctrl Pts',(74.6949326527246,0.669608494786554,45.4140713418108));
#43719=CARTESIAN_POINT('Ctrl Pts',(75.6352699320413,3.08889082506949,45.2775084881384));
#43720=CARTESIAN_POINT('Ctrl Pts',(77.6040687270953,4.78033769006181,45.1409456344659));
#43721=CARTESIAN_POINT('Ctrl Pts',(80.1374209012496,5.34539339909855,45.0043827807935));
#43722=CARTESIAN_POINT('Ctrl Pts',(82.6383925830204,4.65091385357662,44.8678199271211));
#43723=CARTESIAN_POINT('Ctrl Pts',(84.5176797179481,2.86053929560756,44.7312570734486));
#43724=CARTESIAN_POINT('Ctrl Pts',(85.3324658048034,0.396135752429396,44.5946942197762));
#43725=CARTESIAN_POINT('Ctrl Pts',(84.8907627673008,-2.16160927420015,44.4581313661037));
#43726=CARTESIAN_POINT('Ctrl Pts',(83.2966491070823,-4.21001422196126,44.3215685124314));
#43727=CARTESIAN_POINT('Ctrl Pts',(80.9257458927823,-5.26641335792926,44.1850056587589));
#43728=CARTESIAN_POINT('Ctrl Pts',(78.3367091307052,-5.08188730272688,44.0484428050865));
#43729=CARTESIAN_POINT('Ctrl Pts',(76.1395936758935,-3.69991595895718,43.9118799514141));
#43730=CARTESIAN_POINT('Ctrl Pts',(74.8521058814301,-1.44613324326173,43.7753170977416));
#43731=CARTESIAN_POINT('Ctrl Pts',(74.7776166467301,1.14840183966585,43.6387542440692));
#43732=CARTESIAN_POINT('Ctrl Pts',(75.9336776591222,3.47233909138358,43.5021913903967));
#43733=CARTESIAN_POINT('Ctrl Pts',(78.0478866735923,4.97808865150259,43.3656285367243));
#43734=CARTESIAN_POINT('Ctrl Pts',(80.622071564542,5.31085162111149,43.2290656830519));
#43735=CARTESIAN_POINT('Ctrl Pts',(83.0496791219762,4.39221706829951,43.0925028293795));
#43736=CARTESIAN_POINT('Ctrl Pts',(84.7586876558485,2.43864711267794,42.955939975707));
#43737=CARTESIAN_POINT('Ctrl Pts',(85.3464128673449,-0.0895474900135507,
42.8193771220346));
#43738=CARTESIAN_POINT('Ctrl Pts',(84.674348928249,-2.59662892732216,42.6828142683622));
#43739=CARTESIAN_POINT('Ctrl Pts',(82.9008974216893,-4.49189446827444,42.5462514146897));
#43740=CARTESIAN_POINT('Ctrl Pts',(80.4438461537563,-5.32867507453335,42.4096885610173));
#43741=CARTESIAN_POINT('Ctrl Pts',(77.882351758936,-4.9099858892129,42.2731257073449));
#43742=CARTESIAN_POINT('Ctrl Pts',(75.8195931490597,-3.33407937207921,42.1365628536724));
#43743=CARTESIAN_POINT('Ctrl Pts',(75.1017336071131,-1.76011787070273,42.0455209512241));
#43744=CARTESIAN_POINT('Ctrl Pts',(74.9489860411411,-0.934590043769125,
42.));
#43745=CARTESIAN_POINT('Ctrl Pts',(74.9489860411411,-0.934590043769125,
42.));
#43746=CARTESIAN_POINT('Ctrl Pts',(74.9621578377196,-1.08166252357025,42.));
#43747=CARTESIAN_POINT('Ctrl Pts',(74.9817852992141,-1.22784345789557,42.));
#43748=CARTESIAN_POINT('Ctrl Pts',(75.0076019736251,-1.37276211585687,42.));
#43749=CARTESIAN_POINT('Ctrl Pts',(75.0338763132224,-1.52024981983637,42.));
#43750=CARTESIAN_POINT('Ctrl Pts',(75.0665612512022,-1.66643073229691,42.));
#43751=CARTESIAN_POINT('Ctrl Pts',(75.1054285779647,-1.81092654194609,42.));
#43752=CARTESIAN_POINT('Ctrl Pts',(75.1448624859236,-1.95752871227154,42.));
#43753=CARTESIAN_POINT('Ctrl Pts',(75.1906603781215,-2.10239702200426,42.));
#43754=CARTESIAN_POINT('Ctrl Pts',(75.2426373250352,-2.24513869268825,42.));
#43755=CARTESIAN_POINT('Ctrl Pts',(75.29454010169,-2.38767667332699,42.));
#43756=CARTESIAN_POINT('Ctrl Pts',(75.3526044873427,-2.5280948419444,42.));
#43757=CARTESIAN_POINT('Ctrl Pts',(75.4166973936328,-2.66599315453721,42.));
#43758=CARTESIAN_POINT('Ctrl Pts',(75.4326815052143,-2.70038357530239,42.));
#43759=CARTESIAN_POINT('Ctrl Pts',(75.449040803215,-2.7346171978847,42.));
#43760=CARTESIAN_POINT('Ctrl Pts',(75.4657736992349,-2.76868764381097,42.));
#43761=CARTESIAN_POINT('Ctrl Pts',(75.4794370599443,-2.79650809949688,42.));
#43762=CARTESIAN_POINT('Ctrl Pts',(75.4933495262802,-2.82421975339959,42.));
#43763=CARTESIAN_POINT('Ctrl Pts',(75.5075103252484,-2.85181908809118,42.));
#43764=CARTESIAN_POINT('Ctrl Pts',(75.5164010622901,-2.86914709534701,42.));
#43765=CARTESIAN_POINT('Ctrl Pts',(75.5253895443675,-2.88643043349627,42.));
#43766=CARTESIAN_POINT('Ctrl Pts',(75.5344690816879,-2.90365621558174,42.));
#43767=CARTESIAN_POINT('Ctrl Pts',(75.6070587324555,-3.04137397163715,42.));
#43768=CARTESIAN_POINT('Ctrl Pts',(75.6855654691879,-3.17561201831191,42.));
#43769=CARTESIAN_POINT('Ctrl Pts',(75.7697563305504,-3.30597466154241,42.));
#43770=CARTESIAN_POINT('Ctrl Pts',(75.7794264538999,-3.32094805437625,42.));
#43771=CARTESIAN_POINT('Ctrl Pts',(75.7891716226622,-3.33587031738042,42.));
#43772=CARTESIAN_POINT('Ctrl Pts',(75.7989915273745,-3.35074084747145,42.));
#43773=CARTESIAN_POINT('Ctrl Pts',(75.8835543044775,-3.47879639977254,42.));
#43774=CARTESIAN_POINT('Ctrl Pts',(75.973654962357,-3.60301695222072,42.));
#43775=CARTESIAN_POINT('Ctrl Pts',(76.0689073761605,-3.7231766192315,42.));
#43776=CARTESIAN_POINT('Ctrl Pts',(76.1653225040828,-3.84480303480804,42.));
#43777=CARTESIAN_POINT('Ctrl Pts',(76.2670163041758,-3.96226941007647,42.));
#43778=CARTESIAN_POINT('Ctrl Pts',(76.373637405052,-4.07532035528121,42.));
#43779=CARTESIAN_POINT('Ctrl Pts',(76.4750970144414,-4.18289854240666,42.));
#43780=CARTESIAN_POINT('Ctrl Pts',(76.5810191264453,-4.28647872276781,42.));
#43781=CARTESIAN_POINT('Ctrl Pts',(76.6911364486616,-4.38581595590781,42.));
#43782=CARTESIAN_POINT('Ctrl Pts',(76.7174590185628,-4.40956164105969,42.));
#43783=CARTESIAN_POINT('Ctrl Pts',(76.7440214458089,-4.43306475471181,42.));
#43784=CARTESIAN_POINT('Ctrl Pts',(76.7708203338762,-4.45632170068001,42.));
#43785=CARTESIAN_POINT('Ctrl Pts',(76.7863924722136,-4.46983570838862,42.));
#43786=CARTESIAN_POINT('Ctrl Pts',(76.8020444525746,-4.4832665963797,42.));
#43787=CARTESIAN_POINT('Ctrl Pts',(76.8177756225022,-4.49661364255217,42.));
#43788=CARTESIAN_POINT('Ctrl Pts',(76.8327874920505,-4.50935040128779,42.));
#43789=CARTESIAN_POINT('Ctrl Pts',(76.8478645955037,-4.52200496353173,42.));
#43790=CARTESIAN_POINT('Ctrl Pts',(76.8630045687877,-4.53457559580324,42.));
#43791=CARTESIAN_POINT('Ctrl Pts',(76.9853501941721,-4.63615846110177,42.));
#43792=CARTESIAN_POINT('Ctrl Pts',(77.1118304566725,-4.73229035624535,42.));
#43793=CARTESIAN_POINT('Ctrl Pts',(77.2420411835477,-4.82273740245613,42.));
#43794=CARTESIAN_POINT('Ctrl Pts',(77.3736430569181,-4.91415076760505,42.));
#43795=CARTESIAN_POINT('Ctrl Pts',(77.5090559855352,-4.9997577814759,42.));
#43796=CARTESIAN_POINT('Ctrl Pts',(77.647907899746,-5.07928955985309,42.));
#43797=CARTESIAN_POINT('Ctrl Pts',(77.6909792789766,-5.10396003996012,42.));
#43798=CARTESIAN_POINT('Ctrl Pts',(77.7343818612472,-5.12804571555085,42.));
#43799=CARTESIAN_POINT('Ctrl Pts',(77.7781053039389,-5.15153788690001,42.));
#43800=CARTESIAN_POINT('Ctrl Pts',(77.9182247422167,-5.22682266894667,42.));
#43801=CARTESIAN_POINT('Ctrl Pts',(78.06163707807,-5.29601545637256,42.));
#43802=CARTESIAN_POINT('Ctrl Pts',(78.2079144047746,-5.35906058683497,42.));
#43803=CARTESIAN_POINT('Ctrl Pts',(78.2974055901389,-5.39763104463341,42.));
#43804=CARTESIAN_POINT('Ctrl Pts',(78.3879697557877,-5.43389968577381,42.));
#43805=CARTESIAN_POINT('Ctrl Pts',(78.4795137827033,-5.46784552584796,42.));
#43806=CARTESIAN_POINT('Ctrl Pts',(78.5294507402801,-5.48636286698762,42.));
#43807=CARTESIAN_POINT('Ctrl Pts',(78.579679328162,-5.50418890812706,42.));
#43808=CARTESIAN_POINT('Ctrl Pts',(78.6301847786606,-5.52131941272422,42.));
#43809=CARTESIAN_POINT('Ctrl Pts',(78.6542608776631,-5.5294855753972,42.));
#43810=CARTESIAN_POINT('Ctrl Pts',(78.6783998956819,-5.53749367161001,42.));
#43811=CARTESIAN_POINT('Ctrl Pts',(78.7026002488239,-5.54534319403179,42.));
#43812=CARTESIAN_POINT('Ctrl Pts',(78.7227291790244,-5.55187212722577,42.));
#43813=CARTESIAN_POINT('Ctrl Pts',(78.7428924200437,-5.55828870175179,42.));
#43814=CARTESIAN_POINT('Ctrl Pts',(78.7630845889307,-5.56459156251722,42.));
#43815=CARTESIAN_POINT('Ctrl Pts',(78.9185216410264,-5.61311027799698,42.));
#43816=CARTESIAN_POINT('Ctrl Pts',(79.0757515599109,-5.65492040660673,42.));
#43817=CARTESIAN_POINT('Ctrl Pts',(79.2342989894222,-5.69001769854474,42.));
#43818=CARTESIAN_POINT('Ctrl Pts',(79.3943420666046,-5.72544607868212,42.));
#43819=CARTESIAN_POINT('Ctrl Pts',(79.5557282918266,-5.75403468223215,42.));
#43820=CARTESIAN_POINT('Ctrl Pts',(79.7179998356104,-5.77573559499886,42.));
#43821=CARTESIAN_POINT('Ctrl Pts',(79.8804872888693,-5.79746538179104,42.));
#43822=CARTESIAN_POINT('Ctrl Pts',(80.0438631437588,-5.81228940141547,42.));
#43823=CARTESIAN_POINT('Ctrl Pts',(80.2076882609928,-5.82011187102181,42.));
#43824=CARTESIAN_POINT('Ctrl Pts',(80.3001239970504,-5.82452557600221,42.));
#43825=CARTESIAN_POINT('Ctrl Pts',(80.3927030712261,-5.8267093823107,42.));
#43826=CARTESIAN_POINT('Ctrl Pts',(80.4853481377936,-5.82663890625317,42.));
#43827=CARTESIAN_POINT('Ctrl Pts',(80.6073305659698,-5.82654611296212,42.));
#43828=CARTESIAN_POINT('Ctrl Pts',(80.7294274833697,-5.82254585001131,42.));
#43829=CARTESIAN_POINT('Ctrl Pts',(80.8514724367705,-5.81468368107405,42.));
#43830=CARTESIAN_POINT('Ctrl Pts',(80.8742756500897,-5.8132146918989,42.));
#43831=CARTESIAN_POINT('Ctrl Pts',(80.8970770480159,-5.81161083778777,42.));
#43832=CARTESIAN_POINT('Ctrl Pts',(80.919875541321,-5.80987235409354,42.));
#43833=CARTESIAN_POINT('Ctrl Pts',(80.9435592690711,-5.80806636744516,42.));
#43834=CARTESIAN_POINT('Ctrl Pts',(80.9672302930977,-5.80611580996086,42.));
#43835=CARTESIAN_POINT('Ctrl Pts',(80.9908841690558,-5.80402160058609,42.));
#43836=CARTESIAN_POINT('Ctrl Pts',(81.155960195153,-5.78940650063313,42.));
#43837=CARTESIAN_POINT('Ctrl Pts',(81.3202504662812,-5.76779538062928,42.));
#43838=CARTESIAN_POINT('Ctrl Pts',(81.4833338348112,-5.73938880947425,42.));
#43839=CARTESIAN_POINT('Ctrl Pts',(81.6417881370958,-5.71178854923165,42.));
#43840=CARTESIAN_POINT('Ctrl Pts',(81.7991037303719,-5.67777281625275,42.));
#43841=CARTESIAN_POINT('Ctrl Pts',(81.9548995203013,-5.63747982388683,42.));
#43842=CARTESIAN_POINT('Ctrl Pts',(82.0257692259441,-5.61915100698019,42.));
#43843=CARTESIAN_POINT('Ctrl Pts',(82.0963244625258,-5.59952266952908,42.));
#43844=CARTESIAN_POINT('Ctrl Pts',(82.1665291864494,-5.57860481216614,42.));
#43845=CARTESIAN_POINT('Ctrl Pts',(82.2022502415219,-5.56796154070089,42.));
#43846=CARTESIAN_POINT('Ctrl Pts',(82.237880548397,-5.55698439518312,42.));
#43847=CARTESIAN_POINT('Ctrl Pts',(82.2734153269695,-5.54567450906375,42.));
#43848=CARTESIAN_POINT('Ctrl Pts',(82.3062731292964,-5.53521664166231,42.));
#43849=CARTESIAN_POINT('Ctrl Pts',(82.3390528004547,-5.52447298718656,42.));
#43850=CARTESIAN_POINT('Ctrl Pts',(82.3717251389673,-5.51345319731889,42.));
#43851=CARTESIAN_POINT('Ctrl Pts',(82.5334598871624,-5.45890298694057,42.));
#43852=CARTESIAN_POINT('Ctrl Pts',(82.6926833054789,-5.39755431492727,42.));
#43853=CARTESIAN_POINT('Ctrl Pts',(82.8489527497613,-5.32958509775792,42.));
#43854=CARTESIAN_POINT('Ctrl Pts',(83.0023884399965,-5.26284841869041,42.));
#43855=CARTESIAN_POINT('Ctrl Pts',(83.1529770200388,-5.18972885692545,42.));
#43856=CARTESIAN_POINT('Ctrl Pts',(83.300293543373,-5.11034629693712,42.));
#43857=CARTESIAN_POINT('Ctrl Pts',(83.4131779268302,-5.04951774126171,42.));
#43858=CARTESIAN_POINT('Ctrl Pts',(83.5241410217568,-4.98501074834143,42.));
#43859=CARTESIAN_POINT('Ctrl Pts',(83.6330530644636,-4.91696557452329,42.));
#43860=CARTESIAN_POINT('Ctrl Pts',(74.8636515713633,-1.05953972605244E-5,
52.4490415053031));
#43861=CARTESIAN_POINT('Ctrl Pts',(74.8636836703329,0.432042645208333,52.425619963237));
#43862=CARTESIAN_POINT('Ctrl Pts',(74.9176467693691,0.864103762023963,52.4021984211709));
#43863=CARTESIAN_POINT('Ctrl Pts',(75.025442005686,1.28228860328595,52.3787768791048));
#43864=CARTESIAN_POINT('Ctrl Pts',(75.2349474977124,2.09505198615906,52.3332559278806));
#43865=CARTESIAN_POINT('Ctrl Pts',(75.6477979012949,2.85539928139903,52.2877349766565));
#43866=CARTESIAN_POINT('Ctrl Pts',(76.215353236599,3.47375015947001,52.2422140254324));
#43867=CARTESIAN_POINT('Ctrl Pts',(76.7829085719031,4.09210103754099,52.1966930742082));
#43868=CARTESIAN_POINT('Ctrl Pts',(77.5051688389287,4.56845549844299,52.1511721229841));
#43869=CARTESIAN_POINT('Ctrl Pts',(78.2970409309692,4.84669183123127,52.1056511717599));
#43870=CARTESIAN_POINT('Ctrl Pts',(79.0889130230097,5.12492816401956,52.0601302205358));
#43871=CARTESIAN_POINT('Ctrl Pts',(79.950396940065,5.20504636869414,52.0146092693116));
#43872=CARTESIAN_POINT('Ctrl Pts',(80.7799969373556,5.07760731781833,51.9690883180875));
#43873=CARTESIAN_POINT('Ctrl Pts',(81.6095969346462,4.95016826694251,51.9235673668633));
#43874=CARTESIAN_POINT('Ctrl Pts',(82.407313012172,4.61517196051629,51.8780464156392));
#43875=CARTESIAN_POINT('Ctrl Pts',(83.0791622348941,4.11208599470871,51.832525464415));
#43876=CARTESIAN_POINT('Ctrl Pts',(83.7510114576161,3.60900002890112,51.7870045131909));
#43877=CARTESIAN_POINT('Ctrl Pts',(84.2969938255343,2.93782440371217,51.7414835619668));
#43878=CARTESIAN_POINT('Ctrl Pts',(84.652784415277,2.17763368857111,51.6959626107426));
#43879=CARTESIAN_POINT('Ctrl Pts',(85.0085750050198,1.41744297343006,51.6504416595185));
#43880=CARTESIAN_POINT('Ctrl Pts',(85.174173816587,0.568237168336915,51.6049207082943));
#43881=CARTESIAN_POINT('Ctrl Pts',(85.1300708228062,-0.269934528300925,
51.5593997570702));
#43882=CARTESIAN_POINT('Ctrl Pts',(85.0859678290255,-1.10810622493877,51.513878805846));
#43883=CARTESIAN_POINT('Ctrl Pts',(84.8321630298966,-1.93524381312131,51.4683578546219));
#43884=CARTESIAN_POINT('Ctrl Pts',(84.3985584427511,-2.65389806178438,51.4228369033978));
#43885=CARTESIAN_POINT('Ctrl Pts',(83.9649538556056,-3.37255231044745,51.3773159521736));
#43886=CARTESIAN_POINT('Ctrl Pts',(83.3515494804435,-3.98272321959106,51.3317950009495));
#43887=CARTESIAN_POINT('Ctrl Pts',(82.6306135656663,-4.41252349169213,51.2862740497253));
#43888=CARTESIAN_POINT('Ctrl Pts',(81.9096776508892,-4.84232376379319,51.2407530985012));
#43889=CARTESIAN_POINT('Ctrl Pts',(81.0812101964971,-5.09175339885173,51.1952321472771));
#43890=CARTESIAN_POINT('Ctrl Pts',(80.2428171117443,-5.13142583955608,51.1497111960529));
#43891=CARTESIAN_POINT('Ctrl Pts',(79.4044240269915,-5.17109828026043,51.1041902448287));
#43892=CARTESIAN_POINT('Ctrl Pts',(78.5561053118782,-5.0010135266106,51.0586692936046));
#43893=CARTESIAN_POINT('Ctrl Pts',(77.7978056523318,-4.64121011716904,51.0131483423805));
#43894=CARTESIAN_POINT('Ctrl Pts',(77.0395059927855,-4.28140670772748,50.9676273911563));
#43895=CARTESIAN_POINT('Ctrl Pts',(76.3712253888062,-3.73188464249419,50.9221064399322));
#43896=CARTESIAN_POINT('Ctrl Pts',(75.8716973327532,-3.0573858742752,50.876585488708));
#43897=CARTESIAN_POINT('Ctrl Pts',(75.3721692767001,-2.38288710605622,50.8310645374839));
#43898=CARTESIAN_POINT('Ctrl Pts',(75.0413937685732,-1.58341163485156,50.7855435862597));
#43899=CARTESIAN_POINT('Ctrl Pts',(74.9183411312984,-0.753149678856254,
50.7400226350356));
#43900=CARTESIAN_POINT('Ctrl Pts',(74.8814142807203,-0.503996471995245,
50.7263622584581));
#43901=CARTESIAN_POINT('Ctrl Pts',(74.863193691693,-0.252070821087219,50.7127018818806));
#43902=CARTESIAN_POINT('Ctrl Pts',(74.863409785596,-0.000114188402419197,
50.6990415053031));
#43903=CARTESIAN_POINT('Ctrl Pts',(78.4211181181246,-5.90584097022479,54.));
#43904=CARTESIAN_POINT('Ctrl Pts',(78.262197315854,-5.84962792448672,54.));
#43905=CARTESIAN_POINT('Ctrl Pts',(78.1060006691959,-5.78682362442592,54.));
#43906=CARTESIAN_POINT('Ctrl Pts',(77.9528680303037,-5.71771729056826,54.));
#43907=CARTESIAN_POINT('Ctrl Pts',(77.7985213424485,-5.64806307564769,54.));
#43908=CARTESIAN_POINT('Ctrl Pts',(77.6472868104496,-5.57200607329776,54.));
#43909=CARTESIAN_POINT('Ctrl Pts',(77.4995371906765,-5.48979573308941,54.));
#43910=CARTESIAN_POINT('Ctrl Pts',(77.3527503170532,-5.40812108081466,54.));
#43911=CARTESIAN_POINT('Ctrl Pts',(77.2094025440176,-5.32037251008645,54.));
#43912=CARTESIAN_POINT('Ctrl Pts',(77.0698924031099,-5.2267559251608,54.));
#43913=CARTESIAN_POINT('Ctrl Pts',(76.9320428668315,-5.13425366879426,54.));
#43914=CARTESIAN_POINT('Ctrl Pts',(76.7979396790733,-5.03602176868112,54.));
#43915=CARTESIAN_POINT('Ctrl Pts',(76.6680070843611,-4.9322284322092,54.));
#43916=CARTESIAN_POINT('Ctrl Pts',(76.6071928831282,-4.88364855996996,54.));
#43917=CARTESIAN_POINT('Ctrl Pts',(76.5472929286395,-4.83384997802402,54.));
#43918=CARTESIAN_POINT('Ctrl Pts',(76.4883542081234,-4.78284805815547,54.));
#43919=CARTESIAN_POINT('Ctrl Pts',(76.4675681505831,-4.76486109081434,54.));
#43920=CARTESIAN_POINT('Ctrl Pts',(76.4469016708152,-4.74672444521351,54.));
#43921=CARTESIAN_POINT('Ctrl Pts',(76.4263569020757,-4.72843876494938,54.));
#43922=CARTESIAN_POINT('Ctrl Pts',(76.4093496763995,-4.71330164197465,54.));
#43923=CARTESIAN_POINT('Ctrl Pts',(76.3924320826677,-4.69806789557155,54.));
#43924=CARTESIAN_POINT('Ctrl Pts',(76.3756100433455,-4.68274265394818,54.));
#43925=CARTESIAN_POINT('Ctrl Pts',(76.253522088766,-4.57151788699861,54.));
#43926=CARTESIAN_POINT('Ctrl Pts',(76.1363802959433,-4.45540215091792,54.));
#43927=CARTESIAN_POINT('Ctrl Pts',(76.0245380696913,-4.33461793741634,54.));
#43928=CARTESIAN_POINT('Ctrl Pts',(76.0120522412589,-4.32113384453241,54.));
#43929=CARTESIAN_POINT('Ctrl Pts',(75.9996325008476,-4.30759153218521,54.));
#43930=CARTESIAN_POINT('Ctrl Pts',(75.9872793707827,-4.29399128343888,54.));
#43931=CARTESIAN_POINT('Ctrl Pts',(75.8762537634941,-4.17175701014861,54.));
#43932=CARTESIAN_POINT('Ctrl Pts',(75.7706051017538,-4.04484500574663,54.));
#43933=CARTESIAN_POINT('Ctrl Pts',(75.6705456325977,-3.91365715790437,54.));
#43934=CARTESIAN_POINT('Ctrl Pts',(75.5706095000858,-3.78263101658568,54.));
#43935=CARTESIAN_POINT('Ctrl Pts',(75.4762484938177,-3.64733884239891,54.));
#43936=CARTESIAN_POINT('Ctrl Pts',(75.3877215008782,-3.50816030674374,54.));
#43937=CARTESIAN_POINT('Ctrl Pts',(75.3053092655013,-3.3785951440857,54.));
#43938=CARTESIAN_POINT('Ctrl Pts',(75.2279532002239,-3.24566130808865,54.));
#43939=CARTESIAN_POINT('Ctrl Pts',(75.1559025908774,-3.10965711388346,54.));
#43940=CARTESIAN_POINT('Ctrl Pts',(75.1382269322467,-3.07629218149895,54.));
#43941=CARTESIAN_POINT('Ctrl Pts',(75.1208707661237,-3.04274244911447,54.));
#43942=CARTESIAN_POINT('Ctrl Pts',(75.1038381551363,-3.00901230432905,54.));
#43943=CARTESIAN_POINT('Ctrl Pts',(75.0918286612032,-2.98522957545307,54.));
#43944=CARTESIAN_POINT('Ctrl Pts',(75.0799800257135,-2.96135715462957,54.));
#43945=CARTESIAN_POINT('Ctrl Pts',(75.0682937193415,-2.93739658146396,54.));
#43946=CARTESIAN_POINT('Ctrl Pts',(75.0593831488875,-2.91912713271648,54.));
#43947=CARTESIAN_POINT('Ctrl Pts',(75.0505692407358,-2.90081106123106,54.));
#43948=CARTESIAN_POINT('Ctrl Pts',(75.0418557997086,-2.88245623475075,54.));
#43949=CARTESIAN_POINT('Ctrl Pts',(74.9725621697134,-2.73648949775383,54.));
#43950=CARTESIAN_POINT('Ctrl Pts',(74.9095514078268,-2.58793651812475,54.));
#43951=CARTESIAN_POINT('Ctrl Pts',(74.8530199493793,-2.43717464723368,54.));
#43952=CARTESIAN_POINT('Ctrl Pts',(74.7969184627566,-2.28755945393634,54.));
#43953=CARTESIAN_POINT('Ctrl Pts',(74.7471978947673,-2.13576814174227,54.));
#43954=CARTESIAN_POINT('Ctrl Pts',(74.7040995632473,-1.98215647267268,54.));
#43955=CARTESIAN_POINT('Ctrl Pts',(74.689189623633,-1.92901425975836,54.));
#43956=CARTESIAN_POINT('Ctrl Pts',(74.6750726996462,-1.8756541147206,54.));
#43957=CARTESIAN_POINT('Ctrl Pts',(74.6617602392352,-1.82209063115797,54.));
#43958=CARTESIAN_POINT('Ctrl Pts',(74.6229859141292,-1.66607980661111,54.));
#43959=CARTESIAN_POINT('Ctrl Pts',(74.5910324654638,-1.50834341117627,54.));
#43960=CARTESIAN_POINT('Ctrl Pts',(74.5659470122711,-1.34933512929417,54.));
#43961=CARTESIAN_POINT('Ctrl Pts',(74.5514323754776,-1.25733171038229,54.));
#43962=CARTESIAN_POINT('Ctrl Pts',(74.53921800968,-1.16490257794463,54.));
#43963=CARTESIAN_POINT('Ctrl Pts',(74.5293208329226,-1.07213748305002,54.));
#43964=CARTESIAN_POINT('Ctrl Pts',(74.5233288405017,-1.01597522999915,54.));
#43965=CARTESIAN_POINT('Ctrl Pts',(74.5181862975362,-0.959689866802773,
54.));
#43966=CARTESIAN_POINT('Ctrl Pts',(74.5138979638249,-0.903301703642221,
54.));
#43967=CARTESIAN_POINT('Ctrl Pts',(74.5119131404968,-0.877202862178623,
54.));
#43968=CARTESIAN_POINT('Ctrl Pts',(74.5101113192301,-0.851082003289393,
54.));
#43969=CARTESIAN_POINT('Ctrl Pts',(74.5084930266152,-0.82494116692696,54.));
#43970=CARTESIAN_POINT('Ctrl Pts',(74.5072652037706,-0.805107722861111,
54.));
#43971=CARTESIAN_POINT('Ctrl Pts',(74.5061436496233,-0.785272753142196,
54.));
#43972=CARTESIAN_POINT('Ctrl Pts',(74.5051283162844,-0.765437884984759,
54.));
#43973=CARTESIAN_POINT('Ctrl Pts',(74.4970709060958,-0.608033747192235,
54.));
#43974=CARTESIAN_POINT('Ctrl Pts',(74.4956975322905,-0.450619814120949,
54.));
#43975=CARTESIAN_POINT('Ctrl Pts',(74.5009899876326,-0.293622280698601,
54.));
#43976=CARTESIAN_POINT('Ctrl Pts',(74.5062660952276,-0.13710969345059,54.));
#43977=CARTESIAN_POINT('Ctrl Pts',(74.5181670402557,0.018989819316881,54.));
#43978=CARTESIAN_POINT('Ctrl Pts',(74.5367258029922,0.174246479217172,54.));
#43979=CARTESIAN_POINT('Ctrl Pts',(74.554987007931,0.327013865966896,54.));
#43980=CARTESIAN_POINT('Ctrl Pts',(74.5796944593158,0.478965862238273,54.));
#43981=CARTESIAN_POINT('Ctrl Pts',(74.6109264058199,0.629675371802867,54.));
#43982=CARTESIAN_POINT('Ctrl Pts',(74.6274886243206,0.709596225510156,54.));
#43983=CARTESIAN_POINT('Ctrl Pts',(74.6458864053681,0.789167314751061,54.));
#43984=CARTESIAN_POINT('Ctrl Pts',(74.6661366021754,0.868321944692978,54.));
#43985=CARTESIAN_POINT('Ctrl Pts',(74.6929665893138,0.973195873746105,54.));
#43986=CARTESIAN_POINT('Ctrl Pts',(74.7230481604637,1.07733908095142,54.));
#43987=CARTESIAN_POINT('Ctrl Pts',(74.756335592551,1.18060444965825,54.));
#43988=CARTESIAN_POINT('Ctrl Pts',(74.764630155877,1.2063361173301,54.));
#43989=CARTESIAN_POINT('Ctrl Pts',(74.7731238140521,1.23201323737033,54.));
#43990=CARTESIAN_POINT('Ctrl Pts',(74.7818159387465,1.25763344672042,54.));
#43991=CARTESIAN_POINT('Ctrl Pts',(74.7894184833493,1.28004209721328,54.));
#43992=CARTESIAN_POINT('Ctrl Pts',(74.797170156781,1.30239918000046,54.));
#43993=CARTESIAN_POINT('Ctrl Pts',(74.8050684469936,1.3246983529196,54.));
#43994=CARTESIAN_POINT('Ctrl Pts',(74.8566369434172,1.47029123289496,54.));
#43995=CARTESIAN_POINT('Ctrl Pts',(74.9144748216866,1.61348540239222,54.));
#43996=CARTESIAN_POINT('Ctrl Pts',(74.9783786997189,1.7538870626109,54.));
#43997=CARTESIAN_POINT('Ctrl Pts',(75.035748310145,1.87993244198298,54.));
#43998=CARTESIAN_POINT('Ctrl Pts',(75.0980076737178,2.00372722149472,54.));
#43999=CARTESIAN_POINT('Ctrl Pts',(75.1650377417778,2.12496422368888,54.));
#44000=CARTESIAN_POINT('Ctrl Pts',(75.1974826154779,2.18364713029786,54.));
#44001=CARTESIAN_POINT('Ctrl Pts',(75.2310455858999,2.24173042299757,54.));
#44002=CARTESIAN_POINT('Ctrl Pts',(75.2657150993742,2.2991770726025,54.));
#44003=CARTESIAN_POINT('Ctrl Pts',(75.2853531085793,2.3317168379668,54.));
#44004=CARTESIAN_POINT('Ctrl Pts',(75.3053461718748,2.36405230992688,54.));
#44005=CARTESIAN_POINT('Ctrl Pts',(75.3256923528984,2.39617652956482,54.));
#44006=CARTESIAN_POINT('Ctrl Pts',(75.3379464504319,2.41552430397864,54.));
#44007=CARTESIAN_POINT('Ctrl Pts',(75.3503269232296,2.43479266761671,54.));
#44008=CARTESIAN_POINT('Ctrl Pts',(75.3628287363761,2.45397339235937,54.));
#44009=CARTESIAN_POINT('Ctrl Pts',(75.4449389344336,2.57994976787039,54.));
#44010=CARTESIAN_POINT('Ctrl Pts',(75.5323361389007,2.70223687521552,54.));
#44011=CARTESIAN_POINT('Ctrl Pts',(75.6248542953279,2.82044646998141,54.));
#44012=CARTESIAN_POINT('Ctrl Pts',(75.7094873480668,2.92858134052372,54.));
#44013=CARTESIAN_POINT('Ctrl Pts',(75.7984063381093,3.03330408161034,54.));
#44014=CARTESIAN_POINT('Ctrl Pts',(75.8915079123733,3.13428753395923,54.));
#44015=CARTESIAN_POINT('Ctrl Pts',(75.9650364336347,3.21404089991225,54.));
#44016=CARTESIAN_POINT('Ctrl Pts',(76.0411743927007,3.29146134666981,54.));
#44017=CARTESIAN_POINT('Ctrl Pts',(76.1197954215943,3.36643663068922,54.));
#44018=CARTESIAN_POINT('Origin',(70.,0.,54.));
#44019=CARTESIAN_POINT('',(48.9897948556636,-10.,54.));
#44020=CARTESIAN_POINT('',(48.9897948556636,10.,54.));
#44021=CARTESIAN_POINT('Origin',(0.,0.,54.));
#44022=CARTESIAN_POINT('',(100.,-10.,54.));
#44023=CARTESIAN_POINT('',(40.,-10.,54.));
#44024=CARTESIAN_POINT('',(100.,10.,54.));
#44025=CARTESIAN_POINT('',(100.,-10.,54.));
#44026=CARTESIAN_POINT('',(100.,10.,54.));
#44027=CARTESIAN_POINT('Origin',(80.,0.,48.));
#44028=CARTESIAN_POINT('Origin',(40.,-10.,42.));
#44029=CARTESIAN_POINT('',(48.9897948556636,-10.,42.));
#44030=CARTESIAN_POINT('',(48.9897948556636,-10.,41.));
#44031=CARTESIAN_POINT('',(100.,-10.,42.));
#44032=CARTESIAN_POINT('',(40.,-10.,42.));
#44033=CARTESIAN_POINT('',(100.,-10.,42.));
#44034=CARTESIAN_POINT('Origin',(100.,10.,42.));
#44035=CARTESIAN_POINT('',(48.9897948556636,10.,42.));
#44036=CARTESIAN_POINT('',(48.9897948556636,10.,41.));
#44037=CARTESIAN_POINT('',(100.,10.,42.));
#44038=CARTESIAN_POINT('',(100.,10.,42.));
#44039=CARTESIAN_POINT('',(100.,10.,42.));
#44040=CARTESIAN_POINT('Origin',(100.,-10.,42.));
#44041=CARTESIAN_POINT('',(100.,-10.,42.));
#44042=CARTESIAN_POINT('Origin',(70.,0.,42.));
#44043=CARTESIAN_POINT('Origin',(0.,0.,42.));
#44044=CARTESIAN_POINT('Origin',(0.,0.,161.));
#44045=CARTESIAN_POINT('',(-40.,4.89858719658941E-15,161.));
#44046=CARTESIAN_POINT('Origin',(0.,0.,161.));
#44047=CARTESIAN_POINT('',(-35.,-4.28626379701574E-15,161.));
#44048=CARTESIAN_POINT('Origin',(0.,0.,161.));
#44049=CARTESIAN_POINT('Origin',(0.,0.,155.));
#44050=CARTESIAN_POINT('',(-40.,-4.89858719658941E-15,155.));
#44051=CARTESIAN_POINT('Origin',(0.,0.,155.));
#44052=CARTESIAN_POINT('',(-35.,-4.28626379701574E-15,155.));
#44053=CARTESIAN_POINT('Origin',(0.,0.,155.));
#44054=CARTESIAN_POINT('Origin',(0.,0.,155.));
#44055=CARTESIAN_POINT('',(-35.,-4.28626379701574E-15,155.));
#44056=CARTESIAN_POINT('Origin',(0.,0.,41.));
#44057=CARTESIAN_POINT('',(-40.,4.89858719658941E-15,65.));
#44058=CARTESIAN_POINT('',(-40.,-4.89858719658941E-15,41.));
#44059=CARTESIAN_POINT('Origin',(0.,0.,65.));
#44060=CARTESIAN_POINT('Origin',(0.,0.,65.));
#44061=CARTESIAN_POINT('',(-35.,-4.28626379701574E-15,65.));
#44062=CARTESIAN_POINT('Origin',(0.,0.,65.));
#44063=CARTESIAN_POINT('Origin',(0.,0.,59.));
#44064=CARTESIAN_POINT('',(-40.,-4.89858719658941E-15,59.));
#44065=CARTESIAN_POINT('Origin',(0.,0.,59.));
#44066=CARTESIAN_POINT('',(-35.,-4.28626379701574E-15,59.));
#44067=CARTESIAN_POINT('Origin',(0.,0.,59.));
#44068=CARTESIAN_POINT('Origin',(0.,0.,59.));
#44069=CARTESIAN_POINT('',(-35.,-4.28626379701574E-15,59.));
#44070=CARTESIAN_POINT('Origin',(0.,0.,41.));
#44071=CARTESIAN_POINT('',(-40.,-4.89858719658941E-15,41.));
#44072=CARTESIAN_POINT('Origin',(0.,0.,41.));
#44073=CARTESIAN_POINT('',(-40.,-4.89858719658941E-15,179.));
#44074=CARTESIAN_POINT('Origin',(0.,0.,179.));
#44075=CARTESIAN_POINT('',(-40.,-4.89858719658941E-15,41.));
#44076=CARTESIAN_POINT('Origin',(0.,0.,41.));
#44077=CARTESIAN_POINT('Origin',(0.,0.,179.));
#44078=CARTESIAN_POINT('Origin',(0.,0.,179.));
#44079=CARTESIAN_POINT('',(0.,0.,0.));
#44080=CARTESIAN_POINT('Origin',(17.,0.,10.));
#44081=CARTESIAN_POINT('',(8.38741669750802,-2.51341528648493,10.0004125898919));
#44082=CARTESIAN_POINT('',(8.11258330249198,-2.51593117465217,9.99678855536978));
#44083=CARTESIAN_POINT('',(17.,-2.5175,10.));
#44084=CARTESIAN_POINT('',(8.,-1.91346599666512,11.6359872033749));
#44085=CARTESIAN_POINT('Ctrl Pts',(8.11258330249198,-2.51593117465217,9.99678855536978));
#44086=CARTESIAN_POINT('Ctrl Pts',(8.07505553499465,-2.5106778598197,10.5892880216948));
#44087=CARTESIAN_POINT('Ctrl Pts',(8.03752776749733,-2.29922182808408,11.1848035603043));
#44088=CARTESIAN_POINT('Ctrl Pts',(8.,-1.91346599666512,11.6359872033749));
#44089=CARTESIAN_POINT('',(8.,0.,12.5175));
#44090=CARTESIAN_POINT('Origin',(8.,0.,10.));
#44091=CARTESIAN_POINT('',(8.,1.91705370942339,11.63867864773));
#44092=CARTESIAN_POINT('Origin',(8.,0.,10.));
#44093=CARTESIAN_POINT('Ctrl Pts',(8.,1.91705735205381,11.6386813803727));
#44094=CARTESIAN_POINT('Ctrl Pts',(8.05125205967898,1.39129213527502,12.2512665672672));
#44095=CARTESIAN_POINT('Ctrl Pts',(8.10250411935795,0.544371212086402,12.59099264795));
#44096=CARTESIAN_POINT('Ctrl Pts',(8.15375617903693,-0.258560825221013,
12.5080805624475));
#44097=CARTESIAN_POINT('Ctrl Pts',(8.20650761555986,-1.08498260540997,12.4227428873811));
#44098=CARTESIAN_POINT('Ctrl Pts',(8.25925905208279,-1.86480406571553,11.8896768067268));
#44099=CARTESIAN_POINT('Ctrl Pts',(8.31201048860571,-2.2437397594872,11.1506185698235));
#44100=CARTESIAN_POINT('Ctrl Pts',(8.33714589157315,-2.4242979013978,10.7984665181368));
#44101=CARTESIAN_POINT('Ctrl Pts',(8.36228129454058,-2.51383878282056,10.3995459271082));
#44102=CARTESIAN_POINT('Ctrl Pts',(8.38741669750802,-2.51341528648493,10.0004125898919));
#44103=CARTESIAN_POINT('Origin',(17.,0.,10.));
#44104=CARTESIAN_POINT('',(9.38741669750802,-2.51821640390817,9.99779587498902));
#44105=CARTESIAN_POINT('',(9.11258330249198,-2.52124832125375,10.0007652502423));
#44106=CARTESIAN_POINT('',(17.,-2.5175,10.));
#44107=CARTESIAN_POINT('Ctrl Pts',(9.11258330249198,-2.52124832125375,10.0007652502423));
#44108=CARTESIAN_POINT('Ctrl Pts',(9.10992719234634,-2.52141294296029,10.0426045038361));
#44109=CARTESIAN_POINT('Ctrl Pts',(9.1072710822007,-2.5204604246002,10.0844359799301));
#44110=CARTESIAN_POINT('Ctrl Pts',(9.10461497205506,-2.51836711132594,10.1262101550091));
#44111=CARTESIAN_POINT('Ctrl Pts',(9.05201425910005,-2.47691183852974,10.953491883468));
#44112=CARTESIAN_POINT('Ctrl Pts',(8.99941354614505,-1.98805378788741,11.7583010071421));
#44113=CARTESIAN_POINT('Ctrl Pts',(8.94681283319005,-1.27303790376294,12.1765352372871));
#44114=CARTESIAN_POINT('Ctrl Pts',(8.89421212023505,-0.558022019638478,
12.5947694674322));
#44115=CARTESIAN_POINT('Ctrl Pts',(8.84161140728004,0.383151697968126,12.6264288040482));
#44116=CARTESIAN_POINT('Ctrl Pts',(8.78901069432504,1.12455068265491,12.2569425195909));
#44117=CARTESIAN_POINT('Ctrl Pts',(8.73640998137004,1.8659496673417,11.8874562351336));
#44118=CARTESIAN_POINT('Ctrl Pts',(8.68380926841503,2.40757391910867,11.116824329603));
#44119=CARTESIAN_POINT('Ctrl Pts',(8.63120855546003,2.50428468514339,10.2942760189482));
#44120=CARTESIAN_POINT('Ctrl Pts',(8.57860784250503,2.60099545117811,9.47172770829336));
#44121=CARTESIAN_POINT('Ctrl Pts',(8.52600712955003,2.25279273148057,8.59726299251438));
#44122=CARTESIAN_POINT('Ctrl Pts',(8.47340641659503,1.61729847184723,8.06572620427011));
#44123=CARTESIAN_POINT('Ctrl Pts',(8.42080570364003,0.981804212213907,7.53418941602586));
#44124=CARTESIAN_POINT('Ctrl Pts',(8.36820499068502,0.0590184126448082,
7.34558055531628));
#44125=CARTESIAN_POINT('Ctrl Pts',(8.31560427773002,-0.733527071137423,
7.58705948364037));
#44126=CARTESIAN_POINT('Ctrl Pts',(8.26300356477502,-1.52607255491969,7.82853841196447));
#44127=CARTESIAN_POINT('Ctrl Pts',(8.21040285182001,-2.18837772291507,8.50010512932227));
#44128=CARTESIAN_POINT('Ctrl Pts',(8.15780213886501,-2.42039953698568,9.29386718638688));
#44129=CARTESIAN_POINT('Ctrl Pts',(8.14272919340733,-2.48688631923651,9.52132289031894));
#44130=CARTESIAN_POINT('Ctrl Pts',(8.12765624794966,-2.51804115702582,9.75881244500678));
#44131=CARTESIAN_POINT('Ctrl Pts',(8.11258330249198,-2.51593117465217,9.99678855536978));
#44132=CARTESIAN_POINT('Ctrl Pts',(8.38741669750802,-2.51341528648493,10.0004125898919));
#44133=CARTESIAN_POINT('Ctrl Pts',(8.41503273106351,-2.51294999499824,9.56188850305078));
#44134=CARTESIAN_POINT('Ctrl Pts',(8.442648764619,-2.40388679040722,9.12310760576339));
#44135=CARTESIAN_POINT('Ctrl Pts',(8.4702647981745,-2.1876220614921,8.74581465401795));
#44136=CARTESIAN_POINT('Ctrl Pts',(8.52301623469742,-1.77451874248758,8.0251193682683));
#44137=CARTESIAN_POINT('Ctrl Pts',(8.57576767122035,-0.970262177240812,
7.5287791899215));
#44138=CARTESIAN_POINT('Ctrl Pts',(8.62851910774328,-0.1408761191083,7.48239314407354));
#44139=CARTESIAN_POINT('Ctrl Pts',(8.68127054426621,0.688509939024223,7.43600709822558));
#44140=CARTESIAN_POINT('Ctrl Pts',(8.73402198078914,1.54302549004246,7.8395751848765));
#44141=CARTESIAN_POINT('Ctrl Pts',(8.78677341731206,2.03398159212986,8.50960439185275));
#44142=CARTESIAN_POINT('Ctrl Pts',(8.83952485383499,2.52493769421725,9.179633598829));
#44143=CARTESIAN_POINT('Ctrl Pts',(8.89227629035792,2.65233434737381,10.1161239261306));
#44144=CARTESIAN_POINT('Ctrl Pts',(8.94502772688085,2.35817766113461,10.8929680036272));
#44145=CARTESIAN_POINT('Ctrl Pts',(8.99777916340378,2.0640209748954,11.6698120811238));
#44146=CARTESIAN_POINT('Ctrl Pts',(9.05053059992671,1.34831094926045,12.2870099088155));
#44147=CARTESIAN_POINT('Ctrl Pts',(9.10328203644964,0.536674424493379,12.4637998105904));
#44148=CARTESIAN_POINT('Ctrl Pts',(9.15603347297256,-0.274962100273664,
12.6405897123653));
#44149=CARTESIAN_POINT('Ctrl Pts',(9.20878490949549,-1.18252512417281,12.3769716882235));
#44150=CARTESIAN_POINT('Ctrl Pts',(9.26153634601842,-1.77313330145451,11.7928622005606));
#44151=CARTESIAN_POINT('Ctrl Pts',(9.30349646318162,-2.24292123425351,11.3282435256204));
#44152=CARTESIAN_POINT('Ctrl Pts',(9.34545658034482,-2.51216861793005,10.6608466481397));
#44153=CARTESIAN_POINT('Ctrl Pts',(9.38741669750802,-2.51821640390817,9.99779587498902));
#44154=CARTESIAN_POINT('Origin',(17.,0.,10.));
#44155=CARTESIAN_POINT('',(10.387416697508,-2.52029863869409,10.0015637155967));
#44156=CARTESIAN_POINT('',(10.112583302492,-2.51430853248195,10.001394303415));
#44157=CARTESIAN_POINT('',(17.,-2.5175,10.));
#44158=CARTESIAN_POINT('Ctrl Pts',(10.112583302492,-2.51430853248195,10.001394303415));
#44159=CARTESIAN_POINT('Ctrl Pts',(10.092198136743,-2.51595777248054,10.3247931866629));
#44160=CARTESIAN_POINT('Ctrl Pts',(10.0718129709941,-2.45799321307868,10.6476234550357));
#44161=CARTESIAN_POINT('Ctrl Pts',(10.0514278052451,-2.33765469185702,10.9452326133532));
#44162=CARTESIAN_POINT('Ctrl Pts',(9.9988270922901,-2.02714007107045,11.7131662226365));
#44163=CARTESIAN_POINT('Ctrl Pts',(9.9462263793351,-1.30132911626528,12.3131734369901));
#44164=CARTESIAN_POINT('Ctrl Pts',(9.8936256663801,-0.488698459628603,12.4737145429049));
#44165=CARTESIAN_POINT('Ctrl Pts',(9.84102495342509,0.323932197008068,12.6342556488198));
#44166=CARTESIAN_POINT('Ctrl Pts',(9.78842424047009,1.22338255547628,12.3553306462958));
#44167=CARTESIAN_POINT('Ctrl Pts',(9.73582352751509,1.80259317536673,11.7631664355228));
#44168=CARTESIAN_POINT('Ctrl Pts',(9.68322281456008,2.38180379525719,11.1710022247498));
#44169=CARTESIAN_POINT('Ctrl Pts',(9.63062210160508,2.64077467656993,10.2655988057278));
#44170=CARTESIAN_POINT('Ctrl Pts',(9.57802138865008,2.46230433720098,9.4567191109119));
#44171=CARTESIAN_POINT('Ctrl Pts',(9.52542067569508,2.28383399783203,8.64783941609604));
#44172=CARTESIAN_POINT('Ctrl Pts',(9.47281996274007,1.66792243778143,7.93548344548637));
#44173=CARTESIAN_POINT('Ctrl Pts',(9.42021924978507,0.893310282463933,7.64202084104588));
#44174=CARTESIAN_POINT('Ctrl Pts',(9.36761853683007,0.118698127146456,7.3485582366054));
#44175=CARTESIAN_POINT('Ctrl Pts',(9.31501782387507,-0.814614623437939,
7.47398899833411));
#44176=CARTESIAN_POINT('Ctrl Pts',(9.26241711092007,-1.48424475125507,7.96158154582029));
#44177=CARTESIAN_POINT('Ctrl Pts',(9.2124725081107,-2.12006143289624,8.42455276329856));
#44178=CARTESIAN_POINT('Ctrl Pts',(9.16252790530134,-2.51815282999178,9.2140339823356));
#44179=CARTESIAN_POINT('Ctrl Pts',(9.11258330249198,-2.52124832125375,10.0007652502423));
#44180=CARTESIAN_POINT('Ctrl Pts',(9.38741669750802,-2.51821640390817,9.99779587498902));
#44181=CARTESIAN_POINT('Ctrl Pts',(9.39820801686775,-2.51977177587378,9.82727221756083));
#44182=CARTESIAN_POINT('Ctrl Pts',(9.40899933622747,-2.5039186648545,9.65703601909512));
#44183=CARTESIAN_POINT('Ctrl Pts',(9.4197906555872,-2.46959121774327,9.4906105390579));
#44184=CARTESIAN_POINT('Ctrl Pts',(9.47254209211013,-2.30178762608609,8.67706931640221));
#44185=CARTESIAN_POINT('Ctrl Pts',(9.52529352863306,-1.69252711210748,7.95458782227486));
#44186=CARTESIAN_POINT('Ctrl Pts',(9.57804496515599,-0.918992044645595,
7.65185103954266));
#44187=CARTESIAN_POINT('Ctrl Pts',(9.63079640167891,-0.145456977183702,
7.34911425681047));
#44188=CARTESIAN_POINT('Ctrl Pts',(9.68354783820185,0.792352643761475,7.46612218547344));
#44189=CARTESIAN_POINT('Ctrl Pts',(9.73629927472478,1.46778672088276,7.94964481826351));
#44190=CARTESIAN_POINT('Ctrl Pts',(9.7890507112477,2.14322079800404,8.43316745105357));
#44191=CARTESIAN_POINT('Ctrl Pts',(9.84180214777063,2.55627933130144,9.2832047879707));
#44192=CARTESIAN_POINT('Ctrl Pts',(9.89455358429355,2.51904287005632,10.1130358196035));
#44193=CARTESIAN_POINT('Ctrl Pts',(9.94730502081648,2.4818064088112,10.9428668512363));
#44194=CARTESIAN_POINT('Ctrl Pts',(10.0000564573394,1.9942749530235,11.7524915775848));
#44195=CARTESIAN_POINT('Ctrl Pts',(10.0528078938623,1.27824867411093,12.1735761611315));
#44196=CARTESIAN_POINT('Ctrl Pts',(10.1055593303853,0.562222395198357,12.5946607446782));
#44197=CARTESIAN_POINT('Ctrl Pts',(10.1583107669082,-0.382298706839069,
12.6272051854231));
#44198=CARTESIAN_POINT('Ctrl Pts',(10.2110622034311,-1.12561003076715,12.2564032684892));
#44199=CARTESIAN_POINT('Ctrl Pts',(10.2638136399541,-1.86892135469524,11.8856013515554));
#44200=CARTESIAN_POINT('Ctrl Pts',(10.316565076477,-2.41102290051395,11.1114530769427));
#44201=CARTESIAN_POINT('Ctrl Pts',(10.3693165129999,-2.50528839198755,10.2861531872439));
#44202=CARTESIAN_POINT('Ctrl Pts',(10.3753499078359,-2.51606991694613,10.1917603058192));
#44203=CARTESIAN_POINT('Ctrl Pts',(10.381383302672,-2.52099311007268,10.0966982885981));
#44204=CARTESIAN_POINT('Ctrl Pts',(10.387416697508,-2.52029863869409,10.0015637155967));
#44205=CARTESIAN_POINT('Origin',(17.,0.,10.));
#44206=CARTESIAN_POINT('',(11.387416697508,-2.51373500251495,10.0008811020012));
#44207=CARTESIAN_POINT('',(11.112583302492,-2.51647995600113,9.99782029265504));
#44208=CARTESIAN_POINT('',(17.,-2.5175,10.));
#44209=CARTESIAN_POINT('Ctrl Pts',(11.112583302492,-2.51647995600113,9.99782029265504));
#44210=CARTESIAN_POINT('Ctrl Pts',(11.0744690811397,-2.51135536271962,10.601162700555));
#44211=CARTESIAN_POINT('Ctrl Pts',(11.0363548597874,-2.29335787087922,11.2078301743458));
#44212=CARTESIAN_POINT('Ctrl Pts',(10.9982406384351,-1.89829552552759,11.6596889786441));
#44213=CARTESIAN_POINT('Ctrl Pts',(10.9456399254801,-1.35307748643653,12.2832907319479));
#44214=CARTESIAN_POINT('Ctrl Pts',(10.8930392125251,-0.470617551500217,
12.612040242372));
#44215=CARTESIAN_POINT('Ctrl Pts',(10.8404384995701,0.349713918313006,12.4971570813192));
#44216=CARTESIAN_POINT('Ctrl Pts',(10.7878377866151,1.17004538812622,12.3822739202663));
#44217=CARTESIAN_POINT('Ctrl Pts',(10.7352370736601,1.92824839281636,11.8237580877364));
#44218=CARTESIAN_POINT('Ctrl Pts',(10.6826363607051,2.28118689753448,11.0743741314967));
#44219=CARTESIAN_POINT('Ctrl Pts',(10.6300356477501,2.63412540225261,10.3249901752571));
#44220=CARTESIAN_POINT('Ctrl Pts',(10.5774349347951,2.58179940699873,9.38473809530771));
#44221=CARTESIAN_POINT('Ctrl Pts',(10.5248342218401,2.14788981154851,8.67914312428277));
#44222=CARTESIAN_POINT('Ctrl Pts',(10.4722335088851,1.7139802160983,7.97354815325784));
#44223=CARTESIAN_POINT('Ctrl Pts',(10.4196327959301,0.89848702045178,7.50261029115733));
#44224=CARTESIAN_POINT('Ctrl Pts',(10.3670320829751,0.0704738041310564,
7.47945912120493));
#44225=CARTESIAN_POINT('Ctrl Pts',(10.3144313700201,-0.75753941218968,7.45630795125253));
#44226=CARTESIAN_POINT('Ctrl Pts',(10.2618306570651,-1.59807264918463,7.88094347344825));
#44227=CARTESIAN_POINT('Ctrl Pts',(10.2092299441101,-2.07073012429811,8.5611912366526));
#44228=CARTESIAN_POINT('Ctrl Pts',(10.1770143969041,-2.36021135651701,8.97781209017717));
#44229=CARTESIAN_POINT('Ctrl Pts',(10.144798849698,-2.51170216814413,9.49031324977247));
#44230=CARTESIAN_POINT('Ctrl Pts',(10.112583302492,-2.51430853248195,10.001394303415));
#44231=CARTESIAN_POINT('Ctrl Pts',(10.387416697508,-2.52029863869409,10.0015637155967));
#44232=CARTESIAN_POINT('Ctrl Pts',(10.4341347391949,-2.51492117812715,9.26491360929207));
#44233=CARTESIAN_POINT('Ctrl Pts',(10.4808527808818,-2.17272085367765,8.52391321726476));
#44234=CARTESIAN_POINT('Ctrl Pts',(10.5275708225687,-1.60543177741221,8.05553548493098));
#44235=CARTESIAN_POINT('Ctrl Pts',(10.5803222590916,-0.964880234234785,
7.52666917710177));
#44236=CARTESIAN_POINT('Ctrl Pts',(10.6330736956146,-0.0373477107514415,
7.34538806622821));
#44237=CARTESIAN_POINT('Ctrl Pts',(10.6858251321375,0.755189892849743,7.59416505899928));
#44238=CARTESIAN_POINT('Ctrl Pts',(10.7385765686604,1.54772749645094,7.84294205177034));
#44239=CARTESIAN_POINT('Ctrl Pts',(10.7913280051833,2.20527018016997,8.52177714818604));
#44240=CARTESIAN_POINT('Ctrl Pts',(10.8440794417063,2.42867242752584,9.32183795532995));
#44241=CARTESIAN_POINT('Ctrl Pts',(10.8968308782292,2.6520746748817,10.1218987624739));
#44242=CARTESIAN_POINT('Ctrl Pts',(10.9495823147521,2.44133648587441,11.043185280346));
#44243=CARTESIAN_POINT('Ctrl Pts',(11.0023337512751,1.89233207177004,11.6665631803213));
#44244=CARTESIAN_POINT('Ctrl Pts',(11.055085187798,1.34332765766567,12.2899410802967));
#44245=CARTESIAN_POINT('Ctrl Pts',(11.1078366243209,0.456057018464226,12.6154103623752));
#44246=CARTESIAN_POINT('Ctrl Pts',(11.1605880608438,-0.36582085049157,12.4949005236292));
#44247=CARTESIAN_POINT('Ctrl Pts',(11.2133394973668,-1.18769871944735,12.3743906848832));
#44248=CARTESIAN_POINT('Ctrl Pts',(11.2660909338897,-1.94418381815748,11.8079017253127));
#44249=CARTESIAN_POINT('Ctrl Pts',(11.3188423704126,-2.2911173230099,11.0531547493414));
#44250=CARTESIAN_POINT('Ctrl Pts',(11.3417004794444,-2.44144960594696,10.7261098420302));
#44251=CARTESIAN_POINT('Ctrl Pts',(11.3645585884762,-2.5148828983645,10.363716881786));
#44252=CARTESIAN_POINT('Ctrl Pts',(11.387416697508,-2.51373500251495,10.0008811020012));
#44253=CARTESIAN_POINT('Origin',(17.,0.,10.));
#44254=CARTESIAN_POINT('',(12.387416697508,-2.51713767377043,9.99773848900567));
#44255=CARTESIAN_POINT('',(12.112583302492,-2.52111941107521,10.0008984969629));
#44256=CARTESIAN_POINT('',(17.,-2.5175,10.));
#44257=CARTESIAN_POINT('Ctrl Pts',(12.112583302492,-2.52111941107521,10.0008984969629));
#44258=CARTESIAN_POINT('Ctrl Pts',(12.1093407384914,-2.52135655101894,10.0519832687507));
#44259=CARTESIAN_POINT('Ctrl Pts',(12.1060981744908,-2.51993661233261,10.1030546133874));
#44260=CARTESIAN_POINT('Ctrl Pts',(12.1028556104902,-2.51681755665027,10.1540219769643));
#44261=CARTESIAN_POINT('Ctrl Pts',(12.0502548975352,-2.46622038952963,10.9808120298638));
#44262=CARTESIAN_POINT('Ctrl Pts',(11.9976541845802,-1.96849772959592,11.7802392921331));
#44263=CARTESIAN_POINT('Ctrl Pts',(11.9450534716252,-1.24890136395571,12.1905110743009));
#44264=CARTESIAN_POINT('Ctrl Pts',(11.8924527586702,-0.52930499831549,12.6007828564687));
#44265=CARTESIAN_POINT('Ctrl Pts',(11.8398520457152,0.412165073031232,12.621899158535));
#44266=CARTESIAN_POINT('Ctrl Pts',(11.7872513327602,1.14943257671712,12.2443034851074));
#44267=CARTESIAN_POINT('Ctrl Pts',(11.7346506198052,1.886700080403,11.8667078116798));
#44268=CARTESIAN_POINT('Ctrl Pts',(11.6820499068502,2.41976501642805,11.0904001627582));
#44269=CARTESIAN_POINT('Ctrl Pts',(11.6294491938952,2.50738092542064,10.2667101008629));
#44270=CARTESIAN_POINT('Ctrl Pts',(11.5768484809402,2.59499683441322,9.44302003896762));
#44271=CARTESIAN_POINT('Ctrl Pts',(11.5242477679852,2.23716371637332,8.57194756409857));
#44272=CARTESIAN_POINT('Ctrl Pts',(11.4716470550302,1.59582426700453,8.04770947453438));
#44273=CARTESIAN_POINT('Ctrl Pts',(11.4190463420752,0.954484817635741,7.5234713849702));
#44274=CARTESIAN_POINT('Ctrl Pts',(11.3664456291202,0.0296390369380665,
7.34606768071088));
#44275=CARTESIAN_POINT('Ctrl Pts',(11.3138449161652,-0.760160371302549,
7.59578503800158));
#44276=CARTESIAN_POINT('Ctrl Pts',(11.2612442032102,-1.54995977954318,7.84550239529228));
#44277=CARTESIAN_POINT('Ctrl Pts',(11.2086434902552,-2.20471281532674,8.52234081413302));
#44278=CARTESIAN_POINT('Ctrl Pts',(11.1560427773002,-2.42810126159561,9.31998702164505));
#44279=CARTESIAN_POINT('Ctrl Pts',(11.1415562856974,-2.48962352373278,9.53966265792308));
#44280=CARTESIAN_POINT('Ctrl Pts',(11.1270697940947,-2.51842771657201,9.76850130316745));
#44281=CARTESIAN_POINT('Ctrl Pts',(11.112583302492,-2.51647995600113,9.99782029265504));
#44282=CARTESIAN_POINT('Ctrl Pts',(11.387416697508,-2.51373500251495,10.0008811020012));
#44283=CARTESIAN_POINT('Ctrl Pts',(11.4173100249991,-2.51223380980875,9.52637252495675));
#44284=CARTESIAN_POINT('Ctrl Pts',(11.4472033524903,-2.38317769596416,9.05110660128233));
#44285=CARTESIAN_POINT('Ctrl Pts',(11.4770966799814,-2.13175081935672,8.65315481349981));
#44286=CARTESIAN_POINT('Ctrl Pts',(11.5298481165043,-1.68806889985638,7.95090684600186));
#44287=CARTESIAN_POINT('Ctrl Pts',(11.5825995530273,-0.863323149861005,
7.48941590337823));
#44288=CARTESIAN_POINT('Ctrl Pts',(11.6353509895502,-0.0327272062512589,
7.47863480548892));
#44289=CARTESIAN_POINT('Ctrl Pts',(11.6881024260731,0.797868737358476,7.46785370759962));
#44290=CARTESIAN_POINT('Ctrl Pts',(11.740853862596,1.63431487458258,7.90778245444463));
#44291=CARTESIAN_POINT('Ctrl Pts',(11.793605299119,2.09607453959934,8.5982778314047));
#44292=CARTESIAN_POINT('Ctrl Pts',(11.8463567356419,2.5578342046161,9.28877320836478));
#44293=CARTESIAN_POINT('Ctrl Pts',(11.8991081721648,2.64490739742552,10.2298352154399));
#44294=CARTESIAN_POINT('Ctrl Pts',(11.9518596086878,2.31768063801954,10.9933327607025));
#44295=CARTESIAN_POINT('Ctrl Pts',(12.0046110452107,1.99045387861357,11.7568303059651));
#44296=CARTESIAN_POINT('Ctrl Pts',(12.0573624817336,1.24892716699225,12.3427633894151));
#44297=CARTESIAN_POINT('Ctrl Pts',(12.1101139182565,0.430454087136451,12.4845649100919));
#44298=CARTESIAN_POINT('Ctrl Pts',(12.1628653547795,-0.388018992719343,
12.6263664307688));
#44299=CARTESIAN_POINT('Ctrl Pts',(12.2156167913024,-1.28343844080961,12.3240363886725));
#44300=CARTESIAN_POINT('Ctrl Pts',(12.2683682278253,-1.84843800135739,11.7151182083536));
#44301=CARTESIAN_POINT('Ctrl Pts',(12.3080510510529,-2.27346486626798,11.2570530995647));
#44302=CARTESIAN_POINT('Ctrl Pts',(12.3477338742805,-2.51150847337059,10.6254910220656));
#44303=CARTESIAN_POINT('Ctrl Pts',(12.387416697508,-2.51713767377043,9.99773848900567));
#44304=CARTESIAN_POINT('Origin',(17.,0.,10.));
#44305=CARTESIAN_POINT('',(13.387416697508,-2.52103810132661,10.001041928985));
#44306=CARTESIAN_POINT('',(13.112583302492,-2.51415776047792,10.0012738589896));
#44307=CARTESIAN_POINT('',(17.,-2.5175,10.));
#44308=CARTESIAN_POINT('Ctrl Pts',(13.112583302492,-2.51415776047792,10.0012738589896));
#44309=CARTESIAN_POINT('Ctrl Pts',(13.0916116828881,-2.51570257838621,10.3340264679862));
#44310=CARTESIAN_POINT('Ctrl Pts',(13.0706400632842,-2.45424048782787,10.6662314315614));
#44311=CARTESIAN_POINT('Ctrl Pts',(13.0496684436802,-2.32706309090986,10.9710153210997));
#44312=CARTESIAN_POINT('Ctrl Pts',(12.9970677307252,-2.00807858346622,11.735469864416));
#44313=CARTESIAN_POINT('Ctrl Pts',(12.9444670177702,-1.27567943315398,12.3274185767768));
#44314=CARTESIAN_POINT('Ctrl Pts',(12.8918663048152,-0.461323760684686,
12.4789662705914));
#44315=CARTESIAN_POINT('Ctrl Pts',(12.8392655918602,0.353031911784589,12.6305139644061));
#44316=CARTESIAN_POINT('Ctrl Pts',(12.7866648789052,1.24934410641091,12.3416606396747));
#44317=CARTESIAN_POINT('Ctrl Pts',(12.7340641659502,1.82197341812958,11.7431311615882));
#44318=CARTESIAN_POINT('Ctrl Pts',(12.6814634529952,2.39460272984827,11.1446016835016));
#44319=CARTESIAN_POINT('Ctrl Pts',(12.6288627400402,2.64354915865928,10.2363960520598));
#44320=CARTESIAN_POINT('Ctrl Pts',(12.5762620270852,2.45614829825437,9.42953622388729));
#44321=CARTESIAN_POINT('Ctrl Pts',(12.5236613141302,2.26874743784946,8.62267639571484));
#44322=CARTESIAN_POINT('Ctrl Pts',(12.4710606011752,1.64499928822862,7.91716237081174));
#44323=CARTESIAN_POINT('Ctrl Pts',(12.4184598882202,0.867190344919238,7.63228500687628));
#44324=CARTESIAN_POINT('Ctrl Pts',(12.3658591752652,0.0893814016098554,
7.34740764294083));
#44325=CARTESIAN_POINT('Ctrl Pts',(12.3132584623102,-0.842488335388107,
7.48316693997303));
#44326=CARTESIAN_POINT('Ctrl Pts',(12.2606577493552,-1.50668736673329,7.97812301025402));
#44327=CARTESIAN_POINT('Ctrl Pts',(12.2112996004008,-2.12994193654405,8.4425675789753));
#44328=CARTESIAN_POINT('Ctrl Pts',(12.1619414514464,-2.51750967857237,9.22328862565574));
#44329=CARTESIAN_POINT('Ctrl Pts',(12.112583302492,-2.52111941107521,10.0008984969629));
#44330=CARTESIAN_POINT('Ctrl Pts',(12.387416697508,-2.51713767377043,9.99773848900567));
#44331=CARTESIAN_POINT('Ctrl Pts',(12.4004853108034,-2.5189915197724,9.79100281768763));
#44332=CARTESIAN_POINT('Ctrl Pts',(12.4135539240987,-2.49563861108269,9.58468031461302));
#44333=CARTESIAN_POINT('Ctrl Pts',(12.4266225373941,-2.44545626145838,9.38510392197382));
#44334=CARTESIAN_POINT('Ctrl Pts',(12.479373973917,-2.24289528800626,8.57951413445476));
#44335=CARTESIAN_POINT('Ctrl Pts',(12.53212541044,-1.60319366809675,7.88384087795828));
#44336=CARTESIAN_POINT('Ctrl Pts',(12.5848768469629,-0.817380208664749,
7.61457695408235));
#44337=CARTESIAN_POINT('Ctrl Pts',(12.6376282834858,-0.0315667492327322,
7.34531303020641));
#44338=CARTESIAN_POINT('Ctrl Pts',(12.6903797200088,0.900358549721807,7.50245843895104));
#44339=CARTESIAN_POINT('Ctrl Pts',(12.7431311565317,1.55442129220108,8.01452072288645));
#44340=CARTESIAN_POINT('Ctrl Pts',(12.7958825930546,2.20848403468036,8.52658300682186));
#44341=CARTESIAN_POINT('Ctrl Pts',(12.8486340295775,2.58468422068438,9.39356216594807));
#44342=CARTESIAN_POINT('Ctrl Pts',(12.9013854661005,2.51187160157225,10.2210307008325));
#44343=CARTESIAN_POINT('Ctrl Pts',(12.9541369026234,2.43905898246011,11.0484992357168));
#44344=CARTESIAN_POINT('Ctrl Pts',(13.0068883391463,1.91723355823185,11.8364571463594));
#44345=CARTESIAN_POINT('Ctrl Pts',(13.0596397756693,1.18379699541328,12.2264272247595));
#44346=CARTESIAN_POINT('Ctrl Pts',(13.1123912121922,0.450360432594741,12.6163973031597));
#44347=CARTESIAN_POINT('Ctrl Pts',(13.1651426487151,-0.494687268814085,
12.6083795493175));
#44348=CARTESIAN_POINT('Ctrl Pts',(13.217894085238,-1.2214017464924,12.206021597166));
#44349=CARTESIAN_POINT('Ctrl Pts',(13.270645521761,-1.94811622417074,11.8036636450145));
#44350=CARTESIAN_POINT('Ctrl Pts',(13.3233969582839,-2.45649747811857,11.0069654945536));
#44351=CARTESIAN_POINT('Ctrl Pts',(13.3761483948068,-2.51526019467618,10.1783806788171));
#44352=CARTESIAN_POINT('Ctrl Pts',(13.3799044957072,-2.51944432134875,10.119382320145));
#44353=CARTESIAN_POINT('Ctrl Pts',(13.3836605966076,-2.52134889274696,10.0602222968396));
#44354=CARTESIAN_POINT('Ctrl Pts',(13.387416697508,-2.52103810132661,10.001041928985));
#44355=CARTESIAN_POINT('Origin',(17.,0.,10.));
#44356=CARTESIAN_POINT('',(14.387416697508,-2.5142305845587,10.0013871638039));
#44357=CARTESIAN_POINT('',(14.112583302492,-2.51674334939835,9.9977931730102));
#44358=CARTESIAN_POINT('',(17.,-2.5175,10.));
#44359=CARTESIAN_POINT('Ctrl Pts',(14.112583302492,-2.51674334939835,9.9977931730102));
#44360=CARTESIAN_POINT('Ctrl Pts',(14.0738826272847,-2.51142956124591,10.6102558210133));
#44361=CARTESIAN_POINT('Ctrl Pts',(14.0351819520775,-2.28602139692528,11.2262225148951));
#44362=CARTESIAN_POINT('Ctrl Pts',(13.9964812768703,-1.87983305754009,11.6805716463953));
#44363=CARTESIAN_POINT('Ctrl Pts',(13.9438805639153,-1.32775493147994,12.2981083720319));
#44364=CARTESIAN_POINT('Ctrl Pts',(13.8912798509603,-0.441714862070872,
12.6170829616767));
#44365=CARTESIAN_POINT('Ctrl Pts',(13.8386791380053,0.377296548559049,12.4931387240453));
#44366=CARTESIAN_POINT('Ctrl Pts',(13.7860784250503,1.19630795918896,12.3691944864138));
#44367=CARTESIAN_POINT('Ctrl Pts',(13.7334777120953,1.94829071103973,11.8023314215061));
#44368=CARTESIAN_POINT('Ctrl Pts',(13.6808769991403,2.29292383346307,11.0490918343144));
#44369=CARTESIAN_POINT('Ctrl Pts',(13.6282762861853,2.63755695588642,10.2958522471228));
#44370=CARTESIAN_POINT('Ctrl Pts',(13.5756755732303,2.57484044888233,9.35623613764727));
#44371=CARTESIAN_POINT('Ctrl Pts',(13.5230748602753,2.13315759981582,8.65548074121795));
#44372=CARTESIAN_POINT('Ctrl Pts',(13.4704741473203,1.69147475074932,7.95472534478866));
#44373=CARTESIAN_POINT('Ctrl Pts',(13.4178734343653,0.870825559620414,7.49283066140558));
#44374=CARTESIAN_POINT('Ctrl Pts',(13.3652727214103,0.0426070147234524,
7.47883399491689));
#44375=CARTESIAN_POINT('Ctrl Pts',(13.3126720084553,-0.785611530173522,
7.46483732842821));
#44376=CARTESIAN_POINT('Ctrl Pts',(13.2600712955003,-1.62139942883856,7.89873867883393));
#44377=CARTESIAN_POINT('Ctrl Pts',(13.2074705825453,-2.08650844588355,8.58416954117274));
#44378=CARTESIAN_POINT('Ctrl Pts',(13.1758414891942,-2.36618101479215,8.99632282793861));
#44379=CARTESIAN_POINT('Ctrl Pts',(13.1442123958431,-2.51182788845302,9.49942118706689));
#44380=CARTESIAN_POINT('Ctrl Pts',(13.112583302492,-2.51415776047792,10.0012738589896));
#44381=CARTESIAN_POINT('Ctrl Pts',(13.387416697508,-2.52103810132661,10.001041928985));
#44382=CARTESIAN_POINT('Ctrl Pts',(13.4364120331305,-2.51698407552909,9.22908130753535));
#44383=CARTESIAN_POINT('Ctrl Pts',(13.4854073687531,-2.13598344491356,8.45365903697655));
#44384=CARTESIAN_POINT('Ctrl Pts',(13.5344027043756,-1.520510482961,7.98843310210574));
#44385=CARTESIAN_POINT('Ctrl Pts',(13.5871541408985,-0.857853875520787,
7.48754182214329));
#44386=CARTESIAN_POINT('Ctrl Pts',(13.6399055774215,0.0766035185270594,
7.34623074323072));
#44387=CARTESIAN_POINT('Ctrl Pts',(13.6926570139444,0.857735340163466,7.62878857970604));
#44388=CARTESIAN_POINT('Ctrl Pts',(13.7454084504673,1.63886716179986,7.91134641618136));
#44389=CARTESIAN_POINT('Ctrl Pts',(13.7981598869902,2.26667341102482,8.61777316804455));
#44390=CARTESIAN_POINT('Ctrl Pts',(13.8509113235132,2.45553701572534,9.42668378890823));
#44391=CARTESIAN_POINT('Ctrl Pts',(13.9036627600361,2.64440062042586,10.2355944097719));
#44392=CARTESIAN_POINT('Ctrl Pts',(13.956414196559,2.39432158060191,11.1469888996361));
#44393=CARTESIAN_POINT('Ctrl Pts',(14.009165633082,1.81907200865208,11.7462332435378));
#44394=CARTESIAN_POINT('Ctrl Pts',(14.0619170696049,1.24382243670226,12.3454775874394));
#44395=CARTESIAN_POINT('Ctrl Pts',(14.1146685061278,0.343402332626565,12.6325717853785));
#44396=CARTESIAN_POINT('Ctrl Pts',(14.1674199426507,-0.472547026325317,
12.4769038781125));
#44397=CARTESIAN_POINT('Ctrl Pts',(14.2201713791737,-1.28849638527722,12.3212359708466));
#44398=CARTESIAN_POINT('Ctrl Pts',(14.2729228156966,-2.01997499910531,11.7228059583755));
#44399=CARTESIAN_POINT('Ctrl Pts',(14.3256742522195,-2.33420061173484,10.9538663521032));
#44400=CARTESIAN_POINT('Ctrl Pts',(14.3462550673157,-2.45679479415481,10.6538668658346));
#44401=CARTESIAN_POINT('Ctrl Pts',(14.3668358824119,-2.51587694143337,10.327913315048));
#44402=CARTESIAN_POINT('Ctrl Pts',(14.387416697508,-2.5142305845587,10.0013871638039));
#44403=CARTESIAN_POINT('Origin',(17.,0.,10.));
#44404=CARTESIAN_POINT('',(15.387416697508,-2.51610609219152,9.99784272973747));
#44405=CARTESIAN_POINT('',(15.112583302492,-2.52097083132827,10.0010472664792));
#44406=CARTESIAN_POINT('',(17.,-2.5175,10.));
#44407=CARTESIAN_POINT('Ctrl Pts',(15.112583302492,-2.52097083132827,10.0010472664792));
#44408=CARTESIAN_POINT('Ctrl Pts',(15.1087542846364,-2.52129013078259,10.0613807422796));
#44409=CARTESIAN_POINT('Ctrl Pts',(15.1049252667809,-2.51930944209528,10.1216929066385));
#44410=CARTESIAN_POINT('Ctrl Pts',(15.1010962489253,-2.51496119606018,10.18183389453));
#44411=CARTESIAN_POINT('Ctrl Pts',(15.0484955359703,-2.45522764291969,11.0080141214861));
#44412=CARTESIAN_POINT('Ctrl Pts',(14.9958948230153,-1.94869838889795,11.8018906284176));
#44413=CARTESIAN_POINT('Ctrl Pts',(14.9432941100603,-1.22461077616291,12.2041828031708));
#44414=CARTESIAN_POINT('Ctrl Pts',(14.8906933971053,-0.500523163427894,
12.6064749779241));
#44415=CARTESIAN_POINT('Ctrl Pts',(14.8380926841503,0.441122808020406,12.6171828204993));
#44416=CARTESIAN_POINT('Ctrl Pts',(14.7854919711953,1.17417125864671,12.2314603375943));
#44417=CARTESIAN_POINT('Ctrl Pts',(14.7328912582403,1.90721970927303,11.8457378546893));
#44418=CARTESIAN_POINT('Ctrl Pts',(14.6802905452853,2.43167063907734,11.0635850463041));
#44419=CARTESIAN_POINT('Ctrl Pts',(14.6276898323303,2.51017598515645,10.2389767905723));
#44420=CARTESIAN_POINT('Ctrl Pts',(14.5750891193753,2.58868133123557,9.41436853484049));
#44421=CARTESIAN_POINT('Ctrl Pts',(14.5224884064203,2.22124109358949,8.5473048317621));
#44422=CARTESIAN_POINT('Ctrl Pts',(14.4698876934653,1.57414581282329,8.03018824684711));
#44423=CARTESIAN_POINT('Ctrl Pts',(14.4172869805103,0.927050532057081,7.51307166193211));
#44424=CARTESIAN_POINT('Ctrl Pts',(14.3646862675553,0.000300208170735533,
7.34590219518052));
#44425=CARTESIAN_POINT('Ctrl Pts',(14.3120855546003,-0.78669052599029,7.6043348733169));
#44426=CARTESIAN_POINT('Ctrl Pts',(14.2594848416453,-1.5736812601513,7.86276755145327));
#44427=CARTESIAN_POINT('Ctrl Pts',(14.2068841286903,-2.220912404587,8.54680237447761));
#44428=CARTESIAN_POINT('Ctrl Pts',(14.1542834157353,-2.43546988544923,9.34686921680396));
#44429=CARTESIAN_POINT('Ctrl Pts',(14.1403833779875,-2.49216792080863,9.55829143305017));
#44430=CARTESIAN_POINT('Ctrl Pts',(14.1264833402398,-2.51865189118754,9.77781628938327));
#44431=CARTESIAN_POINT('Ctrl Pts',(14.112583302492,-2.51674334939835,9.9977931730102));
#44432=CARTESIAN_POINT('Ctrl Pts',(14.387416697508,-2.5142305845587,10.0013871638039));
#44433=CARTESIAN_POINT('Ctrl Pts',(14.4195873189348,-2.51165710418384,9.49098224793788));
#44434=CARTESIAN_POINT('Ctrl Pts',(14.4517579403615,-2.3606998738868,8.97917824272694));
#44435=CARTESIAN_POINT('Ctrl Pts',(14.4839285617883,-2.07199020161617,8.56291610617037));
#44436=CARTESIAN_POINT('Ctrl Pts',(14.5366799983112,-1.598581567437,7.88035466658329));
#44437=CARTESIAN_POINT('Ctrl Pts',(14.5894314348342,-0.754791687647666,
7.45468098748261));
#44438=CARTESIAN_POINT('Ctrl Pts',(14.6421828713571,0.0755017760662482,
7.47955301676295));
#44439=CARTESIAN_POINT('Ctrl Pts',(14.69493430788,0.905795239780163,7.50442504604328));
#44440=CARTESIAN_POINT('Ctrl Pts',(14.747685744403,1.72259228741866,7.97984278370464));
#44441=CARTESIAN_POINT('Ctrl Pts',(14.8004371809259,2.15429550091668,8.68951749030059));
#44442=CARTESIAN_POINT('Ctrl Pts',(14.8531886174488,2.58599871441471,9.39919219689654));
#44443=CARTESIAN_POINT('Ctrl Pts',(14.9059400539717,2.63260809377225,10.3431238724271));
#44444=CARTESIAN_POINT('Ctrl Pts',(14.9586914904947,2.27291895285955,11.0918758845353));
#44445=CARTESIAN_POINT('Ctrl Pts',(15.0114429270176,1.91322981194686,11.8406278966435));
#44446=CARTESIAN_POINT('Ctrl Pts',(15.0641943635405,1.14724215076395,12.3942002453293));
#44447=CARTESIAN_POINT('Ctrl Pts',(15.1169458000635,0.32343793063549,12.5007481717526));
#44448=CARTESIAN_POINT('Ctrl Pts',(15.1696972365864,-0.500366289492972,
12.607296098176));
#44449=CARTESIAN_POINT('Ctrl Pts',(15.2224486731093,-1.38198706856698,12.2668196023368));
#44450=CARTESIAN_POINT('Ctrl Pts',(15.2752001096322,-1.92033578100497,11.6342166324236));
#44451=CARTESIAN_POINT('Ctrl Pts',(15.3126056389242,-2.30207360389097,11.1856440345767));
#44452=CARTESIAN_POINT('Ctrl Pts',(15.3500111682161,-2.51121114836557,10.5901876216538));
#44453=CARTESIAN_POINT('Ctrl Pts',(15.387416697508,-2.51610609219152,9.99784272973747));
#44454=CARTESIAN_POINT('Origin',(17.,0.,10.));
#44455=CARTESIAN_POINT('',(16.387416697508,-2.52148707396491,10.0004260768809));
#44456=CARTESIAN_POINT('',(16.112583302492,-2.51402132015258,10.00114820235));
#44457=CARTESIAN_POINT('',(17.,-2.5175,10.));
#44458=CARTESIAN_POINT('Ctrl Pts',(16.112583302492,-2.51402132015258,10.00114820235));
#44459=CARTESIAN_POINT('Ctrl Pts',(16.0910252290331,-2.51544798192459,10.3432525163187));
#44460=CARTESIAN_POINT('Ctrl Pts',(16.0694671555742,-2.45037630801831,10.6848371225185));
#44461=CARTESIAN_POINT('Ctrl Pts',(16.0479090821154,-2.31618714117941,10.9966797429082));
#44462=CARTESIAN_POINT('Ctrl Pts',(15.9953083691604,-1.9887717132641,11.7575614698192));
#44463=CARTESIAN_POINT('Ctrl Pts',(15.9427076562054,-1.24987381049529,12.3413779501632));
#44464=CARTESIAN_POINT('Ctrl Pts',(15.8901069432504,-0.433892660596432,
12.4839143588234));
#44465=CARTESIAN_POINT('Ctrl Pts',(15.8375062302954,0.38208848930245,12.6264507674836));
#44466=CARTESIAN_POINT('Ctrl Pts',(15.7849055173404,1.27515288633139,12.3277071044599));
#44467=CARTESIAN_POINT('Ctrl Pts',(15.7323048043854,1.8411309644993,11.7228842545134));
#44468=CARTESIAN_POINT('Ctrl Pts',(15.6797040914304,2.40710904266722,11.1180614045669));
#44469=CARTESIAN_POINT('Ctrl Pts',(15.6271033784754,2.6460008019741,10.2071593676976));
#44470=CARTESIAN_POINT('Ctrl Pts',(15.5745026655204,2.44969222623129,9.4024203989171));
#44471=CARTESIAN_POINT('Ctrl Pts',(15.5219019525654,2.25338365048847,8.59768143013662));
#44472=CARTESIAN_POINT('Ctrl Pts',(15.4693012396104,1.62187473969598,7.89910552944501));
#44473=CARTESIAN_POINT('Ctrl Pts',(15.4167005266554,0.840964237195962,7.62284360324235));
#44474=CARTESIAN_POINT('Ctrl Pts',(15.3640998137004,0.0600537346959255,
7.34658167703968));
#44475=CARTESIAN_POINT('Ctrl Pts',(15.3114991007454,-0.870258359511636,
7.492633725326));
#44476=CARTESIAN_POINT('Ctrl Pts',(15.2588983877904,-1.52894548048579,7.99490172295958));
#44477=CARTESIAN_POINT('Ctrl Pts',(15.2101266926909,-2.13968411168212,8.46060760910896));
#44478=CARTESIAN_POINT('Ctrl Pts',(15.1613549975914,-2.51690378953878,9.2325562337822));
#44479=CARTESIAN_POINT('Ctrl Pts',(15.112583302492,-2.52097083132827,10.0010472664792));
#44480=CARTESIAN_POINT('Ctrl Pts',(15.387416697508,-2.51610609219152,9.99784272973747));
#44481=CARTESIAN_POINT('Ctrl Pts',(15.402762604739,-2.51811428069402,9.75482866384464));
#44482=CARTESIAN_POINT('Ctrl Pts',(15.41810851197,-2.48574611148528,9.51233830240333));
#44483=CARTESIAN_POINT('Ctrl Pts',(15.433454419201,-2.41681664896408,9.28072898098979));
#44484=CARTESIAN_POINT('Ctrl Pts',(15.4862058557239,-2.17987215868322,8.48457374345623));
#44485=CARTESIAN_POINT('Ctrl Pts',(15.5389572922469,-1.51090653231955,7.81699271237621));
#44486=CARTESIAN_POINT('Ctrl Pts',(15.5917087287698,-0.714262078956731,
7.58169828266564));
#44487=CARTESIAN_POINT('Ctrl Pts',(15.6444601652927,0.0823823744060931,
7.34640385295507));
#44488=CARTESIAN_POINT('Ctrl Pts',(15.6972116018157,1.00670565476806,7.54339602461395));
#44489=CARTESIAN_POINT('Ctrl Pts',(15.7499630383386,1.63819186355563,8.08305427002273));
#44490=CARTESIAN_POINT('Ctrl Pts',(15.8027144748615,2.26967807234319,8.62271251543151));
#44491=CARTESIAN_POINT('Ctrl Pts',(15.8554659113844,2.60832720955635,9.50503683459018));
#44492=CARTESIAN_POINT('Ctrl Pts',(15.9082173479074,2.50007267397243,10.3286185301445));
#44493=CARTESIAN_POINT('Ctrl Pts',(15.9609687844303,2.3918181383885,11.1522002256988));
#44494=CARTESIAN_POINT('Ctrl Pts',(16.0137202209532,1.8366599300075,11.9170392976487));
#44495=CARTESIAN_POINT('Ctrl Pts',(16.0664716574762,1.08716428599743,12.2751763291555));
#44496=CARTESIAN_POINT('Ctrl Pts',(16.1192230939991,0.337668641987382,12.6333133606624));
#44497=CARTESIAN_POINT('Ctrl Pts',(16.171974530522,-0.606164437651727,12.5847483517261));
#44498=CARTESIAN_POINT('Ctrl Pts',(16.2247259670449,-1.31494317623276,12.1515756916216));
#44499=CARTESIAN_POINT('Ctrl Pts',(16.2774774035679,-2.02372191481378,11.718403031517));
#44500=CARTESIAN_POINT('Ctrl Pts',(16.3302288400908,-2.49744631233675,10.9006227202442));
#44501=CARTESIAN_POINT('Ctrl Pts',(16.3829802766137,-2.52059800533192,10.0702795063633));
#44502=CARTESIAN_POINT('Ctrl Pts',(16.3844590835785,-2.52124702812834,10.0470020866612));
#44503=CARTESIAN_POINT('Ctrl Pts',(16.3859378905433,-2.52154195635077,10.0237147940671));
#44504=CARTESIAN_POINT('Ctrl Pts',(16.387416697508,-2.52148707396491,10.0004260768809));
#44505=CARTESIAN_POINT('Origin',(17.,0.,10.));
#44506=CARTESIAN_POINT('',(17.387416697508,-2.5149367383853,10.0018020624789));
#44507=CARTESIAN_POINT('',(17.112583302492,-2.51701152631831,9.99777648906939));
#44508=CARTESIAN_POINT('',(17.,-2.5175,10.));
#44509=CARTESIAN_POINT('Ctrl Pts',(17.112583302492,-2.51701152631831,9.99777648906939));
#44510=CARTESIAN_POINT('Ctrl Pts',(17.0732961734298,-2.5115265699017,10.6193511875094));
#44511=CARTESIAN_POINT('Ctrl Pts',(17.0340090443676,-2.27855779157825,11.2446011064688));
#44512=CARTESIAN_POINT('Ctrl Pts',(16.9947219153054,-1.86114087724942,11.7012489582421));
#44513=CARTESIAN_POINT('Ctrl Pts',(16.9421212023504,-1.30227012702427,12.3126451876439));
#44514=CARTESIAN_POINT('Ctrl Pts',(16.8895204893954,-0.412758194743455,
12.6218058510013));
#44515=CARTESIAN_POINT('Ctrl Pts',(16.8369197764404,0.404833074321963,12.48881569523));
#44516=CARTESIAN_POINT('Ctrl Pts',(16.7843190634854,1.22242434338735,12.3558255394588));
#44517=CARTESIAN_POINT('Ctrl Pts',(16.7317183505304,1.96809494923736,11.780684564559));
#44518=CARTESIAN_POINT('Ctrl Pts',(16.6791176375754,2.30438057671027,11.0236813667196));
#44519=CARTESIAN_POINT('Ctrl Pts',(16.6265169246204,2.64066620418318,10.2666781688801));
#44520=CARTESIAN_POINT('Ctrl Pts',(16.5739162116654,2.56756685327896,9.32781274810094));
#44521=CARTESIAN_POINT('Ctrl Pts',(16.5213154987104,2.118164721684,8.63198260438628));
#44522=CARTESIAN_POINT('Ctrl Pts',(16.4687147857554,1.66876259008904,7.93615246067163));
#44523=CARTESIAN_POINT('Ctrl Pts',(16.4161140728004,0.843057677803332,7.48335759402149));
#44524=CARTESIAN_POINT('Ctrl Pts',(16.3635133598454,0.014735014871155,7.47851705097473));
#44525=CARTESIAN_POINT('Ctrl Pts',(16.3109126468904,-0.813587648061016,
7.47367650792798));
#44526=CARTESIAN_POINT('Ctrl Pts',(16.2583119339354,-1.64452806163966,7.91679028848459));
#44527=CARTESIAN_POINT('Ctrl Pts',(16.2057112209804,-2.10203179189809,8.60732066550189));
#44528=CARTESIAN_POINT('Ctrl Pts',(16.1746685814843,-2.37203047763264,9.01484148319913));
#44529=CARTESIAN_POINT('Ctrl Pts',(16.1436259419881,-2.51196699247083,9.50853364155139));
#44530=CARTESIAN_POINT('Ctrl Pts',(16.112583302492,-2.51402132015258,10.00114820235));
#44531=CARTESIAN_POINT('Ctrl Pts',(16.387416697508,-2.52148707396491,10.0004260768809));
#44532=CARTESIAN_POINT('Ctrl Pts',(16.4386893270662,-2.51958421287035,9.192968580655));
#44533=CARTESIAN_POINT('Ctrl Pts',(16.4899619566244,-2.09716665055828,8.38379855228885));
#44534=CARTESIAN_POINT('Ctrl Pts',(16.5412345861825,-1.43278785810852,7.925036755228));
#44535=CARTESIAN_POINT('Ctrl Pts',(16.5939860227054,-0.749247029422589,
7.45304333446249));
#44536=CARTESIAN_POINT('Ctrl Pts',(16.6467374592284,0.19041361641662,7.35196260942039));
#44537=CARTESIAN_POINT('Ctrl Pts',(16.6994888957513,0.958700529009151,7.66778071160203));
#44538=CARTESIAN_POINT('Ctrl Pts',(16.7522403322742,1.72698744160169,7.98359881378368));
#44539=CARTESIAN_POINT('Ctrl Pts',(16.8049917687972,2.32390062094753,8.71631574318908));
#44540=CARTESIAN_POINT('Ctrl Pts',(16.8577432053201,2.47787763070436,9.53258587874038));
#44541=CARTESIAN_POINT('Ctrl Pts',(16.910494641843,2.63185464046118,10.3488560142917));
#44542=CARTESIAN_POINT('Ctrl Pts',(16.9632460783659,2.342895480629,11.2486793559889));
#44543=CARTESIAN_POINT('Ctrl Pts',(17.0159975148889,1.74246056482014,11.8226861204126));
#44544=CARTESIAN_POINT('Ctrl Pts',(17.0687489514118,1.14202564901128,12.3966928848363));
#44545=CARTESIAN_POINT('Ctrl Pts',(17.1215003879347,0.230114977225762,12.6448830719865));
#44546=CARTESIAN_POINT('Ctrl Pts',(17.1742518244576,-0.578402601388186,
12.4543438928164));
#44547=CARTESIAN_POINT('Ctrl Pts',(17.2270032609806,-1.38692018000214,12.2638047136463));
#44548=CARTESIAN_POINT('Ctrl Pts',(17.2797546975035,-2.09204466544451,11.6345361681559));
#44549=CARTESIAN_POINT('Ctrl Pts',(17.3325061340264,-2.37298347042277,10.8528205922691));
#44550=CARTESIAN_POINT('Ctrl Pts',(17.350809655187,-2.47046269943862,10.5815834748014));
#44551=CARTESIAN_POINT('Ctrl Pts',(17.3691131763475,-2.51687300377292,10.2919928242661));
#44552=CARTESIAN_POINT('Ctrl Pts',(17.387416697508,-2.5149367383853,10.0018020624789));
#44553=CARTESIAN_POINT('Origin',(17.,0.,10.));
#44554=CARTESIAN_POINT('',(18.387416697508,-2.51518334819126,9.99809619657404));
#44555=CARTESIAN_POINT('',(18.112583302492,-2.5208033701771,10.0011896703713));
#44556=CARTESIAN_POINT('',(17.,-2.5175,10.));
#44557=CARTESIAN_POINT('Ctrl Pts',(18.112583302492,-2.5208033701771,10.0011896703713));
#44558=CARTESIAN_POINT('Ctrl Pts',(18.1081678307815,-2.52121299156672,10.0707760983448));
#44559=CARTESIAN_POINT('Ctrl Pts',(18.103752359071,-2.51857806098439,10.1403310528238));
#44560=CARTESIAN_POINT('Ctrl Pts',(18.0993368873605,-2.5127975112366,10.2096235922112));
#44561=CARTESIAN_POINT('Ctrl Pts',(18.0467361744055,-2.44393487142343,11.03509303539));
#44562=CARTESIAN_POINT('Ctrl Pts',(17.9941354614505,-1.92866092038828,11.8233217768237));
#44563=CARTESIAN_POINT('Ctrl Pts',(17.9415347484955,-1.20017054290006,12.2175851845743));
#44564=CARTESIAN_POINT('Ctrl Pts',(17.8889340355405,-0.47168016541185,12.6118485923249));
#44565=CARTESIAN_POINT('Ctrl Pts',(17.8363333225855,0.470026638529419,12.6121466663925));
#44566=CARTESIAN_POINT('Ctrl Pts',(17.7837326096305,1.19876645873966,12.2183445089276));
#44567=CARTESIAN_POINT('Ctrl Pts',(17.7311318966755,1.92750627894991,11.8245423514627));
#44568=CARTESIAN_POINT('Ctrl Pts',(17.6785311837205,2.44327911542912,11.0366399624654));
#44569=CARTESIAN_POINT('Ctrl Pts',(17.6259304707655,2.51266430538601,10.2112142782281));
#44570=CARTESIAN_POINT('Ctrl Pts',(17.5733297578105,2.58204949534291,9.38578859399074));
#44571=CARTESIAN_POINT('Ctrl Pts',(17.5207290448555,2.20504703877749,8.52283961451336));
#44572=CARTESIAN_POINT('Ctrl Pts',(17.4681283319005,1.55227500058467,8.01290772598547));
#44573=CARTESIAN_POINT('Ctrl Pts',(17.4155276189455,0.899502962391848,7.50297583745757));
#44574=CARTESIAN_POINT('Ctrl Pts',(17.3629269059905,-0.0290386574283893,
7.34606103987917));
#44575=CARTESIAN_POINT('Ctrl Pts',(17.3103261930355,-0.813124548432665,
7.61317745703109));
#44576=CARTESIAN_POINT('Ctrl Pts',(17.2577254800805,-1.59721043943693,7.880293874183));
#44577=CARTESIAN_POINT('Ctrl Pts',(17.2051247671255,-2.23684060162524,8.57144150606521));
#44578=CARTESIAN_POINT('Ctrl Pts',(17.1525240541704,-2.44254089863465,9.3738312197295));
#44579=CARTESIAN_POINT('Ctrl Pts',(17.1392104702776,-2.49460498687914,9.57692129527171));
#44580=CARTESIAN_POINT('Ctrl Pts',(17.1258968863848,-2.51887026298714,9.78713786286086));
#44581=CARTESIAN_POINT('Ctrl Pts',(17.112583302492,-2.51701152631831,9.99777648906939));
#44582=CARTESIAN_POINT('Ctrl Pts',(17.387416697508,-2.5149367383853,10.0018020624789));
#44583=CARTESIAN_POINT('Ctrl Pts',(17.4218646128704,-2.51129261408774,9.45565213245618));
#44584=CARTESIAN_POINT('Ctrl Pts',(17.4563125282328,-2.33640176855005,8.9073765690155));
#44585=CARTESIAN_POINT('Ctrl Pts',(17.4907604435952,-2.00841223852946,8.47532502033285));
#44586=CARTESIAN_POINT('Ctrl Pts',(17.5435118801181,-1.50614907714372,7.81370763056639));
#44587=CARTESIAN_POINT('Ctrl Pts',(17.5962633166411,-0.644869629858092,
7.42463545731654));
#44588=CARTESIAN_POINT('Ctrl Pts',(17.649014753164,0.1835916570973,7.48511479050391));
#44589=CARTESIAN_POINT('Ctrl Pts',(17.7017661896869,1.01205294405269,7.54559412369128));
#44590=CARTESIAN_POINT('Ctrl Pts',(17.7545176262099,1.80769607067784,8.05562496331587));
#44591=CARTESIAN_POINT('Ctrl Pts',(17.8072690627328,2.20854748135092,8.78317152559761));
#44592=CARTESIAN_POINT('Ctrl Pts',(17.8600204992557,2.609398892024,9.51071808787935));
#44593=CARTESIAN_POINT('Ctrl Pts',(17.9127719357786,2.615458586745,10.4557803728183));
#44594=CARTESIAN_POINT('Ctrl Pts',(17.9655233723016,2.22396974003433,11.1884073833958));
#44595=CARTESIAN_POINT('Ctrl Pts',(18.0182748088245,1.83248089332367,11.9210343939733));
#44596=CARTESIAN_POINT('Ctrl Pts',(18.0710262453474,1.04344350518134,12.4412261301894));
#44597=CARTESIAN_POINT('Ctrl Pts',(18.1237776818704,0.215825886080791,12.51232416308));
#44598=CARTESIAN_POINT('Ctrl Pts',(18.1765291183933,-0.611791733019759,
12.5834221959705));
#44599=CARTESIAN_POINT('Ctrl Pts',(18.2292805549162,-1.47798958307853,12.2054265255356));
#44600=CARTESIAN_POINT('Ctrl Pts',(18.2820319914391,-1.98869561701118,11.5503042463912));
#44601=CARTESIAN_POINT('Ctrl Pts',(18.3171602267954,-2.32878496699634,11.1140452338251));
#44602=CARTESIAN_POINT('Ctrl Pts',(18.3522884621517,-2.51123167916713,10.5548945888113));
#44603=CARTESIAN_POINT('Ctrl Pts',(18.387416697508,-2.51518334819126,9.99809619657404));
#44604=CARTESIAN_POINT('Origin',(17.,0.,10.));
#44605=CARTESIAN_POINT('',(19.387416697508,-2.52155059213328,9.99976874863484));
#44606=CARTESIAN_POINT('',(19.112583302492,-2.51389966012859,10.0010175250377));
#44607=CARTESIAN_POINT('',(17.,-2.5175,10.));
#44608=CARTESIAN_POINT('Ctrl Pts',(19.112583302492,-2.51389966012859,10.0010175250377));
#44609=CARTESIAN_POINT('Ctrl Pts',(19.0904387751782,-2.51519458398436,10.3524708738624));
#44610=CARTESIAN_POINT('Ctrl Pts',(19.0682942478644,-2.4464002454655,10.7034398319222));
#44611=CARTESIAN_POINT('Ctrl Pts',(19.0461497205505,-2.30502815708954,11.0222223720467));
#44612=CARTESIAN_POINT('Ctrl Pts',(18.9935490075955,-1.96922181834357,11.7794383040252));
#44613=CARTESIAN_POINT('Ctrl Pts',(18.9409482946405,-1.22391545525877,12.355051210919));
#44614=CARTESIAN_POINT('Ctrl Pts',(18.8883475816855,-0.406408539519951,
12.4885589167013));
#44615=CARTESIAN_POINT('Ctrl Pts',(18.8357468687305,0.411098376218855,12.6220666224836));
#44616=CARTESIAN_POINT('Ctrl Pts',(18.7831461557755,1.30080584461167,12.3134691271544));
#44617=CARTESIAN_POINT('Ctrl Pts',(18.7305454428205,1.86006352761385,11.7024268137365));
#44618=CARTESIAN_POINT('Ctrl Pts',(18.6779447298655,2.41932121061604,11.0913845003187));
#44619=CARTESIAN_POINT('Ctrl Pts',(18.6253440169105,2.64812910822757,10.1778973688121));
#44620=CARTESIAN_POINT('Ctrl Pts',(18.5727433039555,2.44293680574081,9.37537759722749));
#44621=CARTESIAN_POINT('Ctrl Pts',(18.5201425910005,2.23774450325404,8.57285782564289));
#44622=CARTESIAN_POINT('Ctrl Pts',(18.4675418780455,1.59855200066899,7.8813054139802));
#44623=CARTESIAN_POINT('Ctrl Pts',(18.4149411650905,0.814635364990448,7.61369268429331));
#44624=CARTESIAN_POINT('Ctrl Pts',(18.3623404521355,0.0307187293118991,
7.34607995460641));
#44625=CARTESIAN_POINT('Ctrl Pts',(18.3097397391805,-0.897922039460136,
7.50240690689532));
#44626=CARTESIAN_POINT('Ctrl Pts',(18.2571390262255,-1.55101675955056,8.01192545550181));
#44627=CARTESIAN_POINT('Ctrl Pts',(18.208953784981,-2.14928862461043,8.47867339110784));
#44628=CARTESIAN_POINT('Ctrl Pts',(18.1607685437365,-2.51633324631003,9.24180561378778));
#44629=CARTESIAN_POINT('Ctrl Pts',(18.112583302492,-2.5208033701771,10.0011896703713));
#44630=CARTESIAN_POINT('Ctrl Pts',(18.387416697508,-2.51518334819126,9.99809619657404));
#44631=CARTESIAN_POINT('Ctrl Pts',(18.4050398986747,-2.51716582916276,9.71876050048428));
#44632=CARTESIAN_POINT('Ctrl Pts',(18.4226630998413,-2.474223826934,9.44001683058457));
#44633=CARTESIAN_POINT('Ctrl Pts',(18.4402863010079,-2.3837243979264,9.17767919384928));
#44634=CARTESIAN_POINT('Ctrl Pts',(18.4930377375309,-2.11283292710244,8.39242530830563));
#44635=CARTESIAN_POINT('Ctrl Pts',(18.5457891740538,-1.41583576764798,7.75416642507215));
#44636=CARTESIAN_POINT('Ctrl Pts',(18.5985406105767,-0.609828023666041,
7.55327498581276));
#44637=CARTESIAN_POINT('Ctrl Pts',(18.6512920470996,0.196179720315914,7.35238354655336));
#44638=CARTESIAN_POINT('Ctrl Pts',(18.7040434836226,1.11119804882536,7.58885955126807));
#44639=CARTESIAN_POINT('Ctrl Pts',(18.7567949201455,1.71894430102338,8.15511951512376));
#44640=CARTESIAN_POINT('Ctrl Pts',(18.8095463566684,2.32669055322138,8.72137947897945));
#44641=CARTESIAN_POINT('Ctrl Pts',(18.8622977931914,2.62716472910797,9.61742340197613));
#44642=CARTESIAN_POINT('Ctrl Pts',(18.9150492297143,2.48366772052954,10.4356009268786));
#44643=CARTESIAN_POINT('Ctrl Pts',(18.9678006662372,2.34017071195111,11.2537784517812));
#44644=CARTESIAN_POINT('Ctrl Pts',(19.0205521027601,1.75270251890765,11.9940895785895));
#44645=CARTESIAN_POINT('Ctrl Pts',(19.0733035392831,0.988528632087992,12.319733747015));
#44646=CARTESIAN_POINT('Ctrl Pts',(19.126054975806,0.224354745268327,12.6453779154405));
#44647=CARTESIAN_POINT('Ctrl Pts',(19.1788064123289,-0.716524835327532,
12.556355125483));
#44648=CARTESIAN_POINT('Ctrl Pts',(19.2315578488519,-1.40606201149648,12.0931658160128));
#44649=CARTESIAN_POINT('Ctrl Pts',(19.2835107984039,-2.08516181406211,11.6369877019343));
#44650=CARTESIAN_POINT('Ctrl Pts',(19.335463747956,-2.52047065422532,10.8178846922386));
#44651=CARTESIAN_POINT('Ctrl Pts',(19.387416697508,-2.52155059213328,9.99976874863484));
#44652=CARTESIAN_POINT('Origin',(17.,0.,10.));
#44653=CARTESIAN_POINT('',(20.387416697508,-2.5158164891674,10.0020963764446));
#44654=CARTESIAN_POINT('',(20.112583302492,-2.51728339305687,9.99777041742395));
#44655=CARTESIAN_POINT('',(17.,-2.5175,10.));
#44656=CARTESIAN_POINT('Ctrl Pts',(20.112583302492,-2.51728339305687,9.99777041742395));
#44657=CARTESIAN_POINT('Ctrl Pts',(20.0727097195748,-2.51164716853644,10.6284495053142));
#44658=CARTESIAN_POINT('Ctrl Pts',(20.0328361366577,-2.27096645283767,11.2629653655237));
#44659=CARTESIAN_POINT('Ctrl Pts',(19.9929625537406,-1.84222126852405,11.7217183801906));
#44660=CARTESIAN_POINT('Ctrl Pts',(19.9403618407856,-1.27662618724459,12.3268994017176));
#44661=CARTESIAN_POINT('Ctrl Pts',(19.8877611278306,-0.383751089025701,
12.6262083598496));
#44662=CARTESIAN_POINT('Ctrl Pts',(19.8351604148756,0.432320130131445,12.4841885371227));
#44663=CARTESIAN_POINT('Ctrl Pts',(19.7825597019206,1.2483913492886,12.3421687143957));
#44664=CARTESIAN_POINT('Ctrl Pts',(19.7299589889656,1.98765868938402,11.7588201108097));
#44665=CARTESIAN_POINT('Ctrl Pts',(19.6773582760106,2.31555572834135,10.9981458069009));
#44666=CARTESIAN_POINT('Ctrl Pts',(19.6247575630556,2.64345276729868,10.2374715029922));
#44667=CARTESIAN_POINT('Ctrl Pts',(19.5721568501006,2.55997950511793,9.29947149876068));
#44668=CARTESIAN_POINT('Ctrl Pts',(19.5195561371456,2.10291300721531,8.60865163708974));
#44669=CARTESIAN_POINT('Ctrl Pts',(19.4669554241906,1.64584650931268,7.91783177541879));
#44670=CARTESIAN_POINT('Ctrl Pts',(19.4143547112356,0.815186775688189,7.47419205630841));
#44671=CARTESIAN_POINT('Ctrl Pts',(19.3617539982806,-0.0131387855763111,
7.47850822821053));
#44672=CARTESIAN_POINT('Ctrl Pts',(19.3091532853256,-0.841464346840806,
7.48282440011265));
#44673=CARTESIAN_POINT('Ctrl Pts',(19.2565525723705,-1.66745573574531,7.93509646302726));
#44674=CARTESIAN_POINT('Ctrl Pts',(19.2039518594155,-2.11729827299398,8.63064197301616));
#44675=CARTESIAN_POINT('Ctrl Pts',(19.1734956737744,-2.37776029059948,9.03336775341074));
#44676=CARTESIAN_POINT('Ctrl Pts',(19.1430394881332,-2.51211870356159,9.51765076428747));
#44677=CARTESIAN_POINT('Ctrl Pts',(19.112583302492,-2.51389966012859,10.0010175250377));
#44678=CARTESIAN_POINT('Ctrl Pts',(19.387416697508,-2.52155059213328,9.99976874863484));
#44679=CARTESIAN_POINT('Ctrl Pts',(19.3882151844789,-2.52156719015815,9.98719477685344));
#44680=CARTESIAN_POINT('Ctrl Pts',(19.3890136714498,-2.52148121496597,9.97462103823604));
#44681=CARTESIAN_POINT('Ctrl Pts',(19.3898121584206,-2.52129197516155,9.96204885398458));
#44682=CARTESIAN_POINT('Ctrl Pts',(19.4425635949436,-2.50878999091566,9.1314770304097));
#44683=CARTESIAN_POINT('Ctrl Pts',(19.4953150314665,-2.0455912506818,8.30768921224301));
#44684=CARTESIAN_POINT('Ctrl Pts',(19.5480664679894,-1.34242552683065,7.8654632309535));
#44685=CARTESIAN_POINT('Ctrl Pts',(19.6008179045124,-0.639259802979503,
7.423237249664));
#44686=CARTESIAN_POINT('Ctrl Pts',(19.6535693410353,0.30387290448894,7.36257310525166));
#44687=CARTESIAN_POINT('Ctrl Pts',(19.7063207775582,1.0578994494348,7.71106962351769));
#44688=CARTESIAN_POINT('Ctrl Pts',(19.7590722140811,1.81192599438068,8.05956614178372));
#44689=CARTESIAN_POINT('Ctrl Pts',(19.811823650604,2.37684637680396,8.81722332272812));
#44690=CARTESIAN_POINT('Ctrl Pts',(19.864575087127,2.49565311102915,9.63934911214806));
#44691=CARTESIAN_POINT('Ctrl Pts',(19.9173265236499,2.61445984525433,10.461474901568));
#44692=CARTESIAN_POINT('Ctrl Pts',(19.9700779601728,2.2871529312814,11.3480692994635));
#44693=CARTESIAN_POINT('Ctrl Pts',(20.0228293966958,1.66263888695187,11.8957809591547));
#44694=CARTESIAN_POINT('Ctrl Pts',(20.0755808332187,1.03812484262234,12.443492618846));
#44695=CARTESIAN_POINT('Ctrl Pts',(20.1283322697416,0.116403667936205,12.6523215403331));
#44696=CARTESIAN_POINT('Ctrl Pts',(20.1810837062646,-0.683192552496604,
12.4272621304076));
#44697=CARTESIAN_POINT('Ctrl Pts',(20.2338351427875,-1.48278877292941,12.2022027204822));
#44698=CARTESIAN_POINT('Ctrl Pts',(20.2865865793104,-2.16026003910891,11.5432549791442));
#44699=CARTESIAN_POINT('Ctrl Pts',(20.3393380158334,-2.40739444692378,10.7502036326345));
#44700=CARTESIAN_POINT('Ctrl Pts',(20.3553642430582,-2.48247547666995,10.5092695099277));
#44701=CARTESIAN_POINT('Ctrl Pts',(20.3713904702831,-2.51783711775732,10.2559578436506));
#44702=CARTESIAN_POINT('Ctrl Pts',(20.387416697508,-2.5158164891674,10.0020963764446));
#44703=CARTESIAN_POINT('Origin',(17.,0.,10.));
#44704=CARTESIAN_POINT('',(21.387416697508,-2.51442093719447,9.99847790324227));
#44705=CARTESIAN_POINT('',(21.112583302492,-2.5206186296165,10.0013249946411));
#44706=CARTESIAN_POINT('',(17.,-2.5175,10.));
#44707=CARTESIAN_POINT('Ctrl Pts',(21.112583302492,-2.5206186296165,10.0013249946411));
#44708=CARTESIAN_POINT('Ctrl Pts',(21.1075813769266,-2.52112526980945,10.0801690222653));
#44709=CARTESIAN_POINT('Ctrl Pts',(21.1025794513611,-2.51774238317523,10.1589690246946));
#44710=CARTESIAN_POINT('Ctrl Pts',(21.0975775257956,-2.51032676658054,10.2373876742263));
#44711=CARTESIAN_POINT('Ctrl Pts',(21.0449768128406,-2.43234345499833,11.0620454625851));
#44712=CARTESIAN_POINT('Ctrl Pts',(20.9923760998856,-1.90838777260282,11.8445301182286));
#44713=CARTESIAN_POINT('Ctrl Pts',(20.9397753869306,-1.17558365071925,12.2307165806189));
#44714=CARTESIAN_POINT('Ctrl Pts',(20.8871746739756,-0.442779528835683,
12.6169030430092));
#44715=CARTESIAN_POINT('Ctrl Pts',(20.8345739610206,0.498873032535946,12.6067913121462));
#44716=CARTESIAN_POINT('Ctrl Pts',(20.7819732480656,1.22321517149131,12.2049576021148));
#44717=CARTESIAN_POINT('Ctrl Pts',(20.7293725351106,1.94755731044668,11.8031238920834));
#44718=CARTESIAN_POINT('Ctrl Pts',(20.6767718221556,2.45458902698578,11.0095682028835));
#44719=CARTESIAN_POINT('Ctrl Pts',(20.6241711092006,2.51484558206126,10.1834259558372));
#44720=CARTESIAN_POINT('Ctrl Pts',(20.5715703962456,2.57510213713674,9.35728370879087));
#44721=CARTESIAN_POINT('Ctrl Pts',(20.5189696832906,2.18858353074863,8.49855490389815));
#44722=CARTESIAN_POINT('Ctrl Pts',(20.4663689703356,1.53021450282693,7.99587002461758));
#44723=CARTESIAN_POINT('Ctrl Pts',(20.4137682573806,0.871845474905217,7.49318514533701));
#44724=CARTESIAN_POINT('Ctrl Pts',(20.3611675444256,-0.0583739745500803,
7.34654419166858));
#44725=CARTESIAN_POINT('Ctrl Pts',(20.3085668314706,-0.839459208357427,
7.6223117066376));
#44726=CARTESIAN_POINT('Ctrl Pts',(20.2559661185156,-1.62054444216476,7.89807922160661));
#44727=CARTESIAN_POINT('Ctrl Pts',(20.2033654055606,-2.25249546032415,8.59625520521304));
#44728=CARTESIAN_POINT('Ctrl Pts',(20.1507646926056,-2.44931343723384,9.40086973947727));
#44729=CARTESIAN_POINT('Ctrl Pts',(20.1380375625677,-2.49693499681351,9.59555215408064));
#44730=CARTESIAN_POINT('Ctrl Pts',(20.1253104325298,-2.51908240275568,9.79646583989391));
#44731=CARTESIAN_POINT('Ctrl Pts',(20.112583302492,-2.51728339305687,9.99777041742395));
#44732=CARTESIAN_POINT('Ctrl Pts',(20.387416697508,-2.5158164891674,10.0020963764446));
#44733=CARTESIAN_POINT('Ctrl Pts',(20.424141906806,-2.51118607885081,9.42035524766764));
#44734=CARTESIAN_POINT('Ctrl Pts',(20.4608671161041,-2.31025054570517,8.8357269550081));
#44735=CARTESIAN_POINT('Ctrl Pts',(20.4975923254021,-1.94113406353733,8.39054292978191));
#44736=CARTESIAN_POINT('Ctrl Pts',(20.550343761925,-1.41094172288576,7.75108852512045));
#44737=CARTESIAN_POINT('Ctrl Pts',(20.603095198448,-0.533759492132356,7.39933466747897));
#44738=CARTESIAN_POINT('Ctrl Pts',(20.6558466349709,0.291343296794607,7.49530988006332));
#44739=CARTESIAN_POINT('Ctrl Pts',(20.7085980714939,1.11644608572156,7.59128509264767));
#44740=CARTESIAN_POINT('Ctrl Pts',(20.7613495080168,1.88946943282209,8.13498937545785));
#44741=CARTESIAN_POINT('Ctrl Pts',(20.8141009445397,2.25873052935675,8.87906739308414));
#44742=CARTESIAN_POINT('Ctrl Pts',(20.8668523810626,2.62799162589142,9.62314541071043));
#44743=CARTESIAN_POINT('Ctrl Pts',(20.9196038175855,2.59349047186024,10.5675971631528));
#44744=CARTESIAN_POINT('Ctrl Pts',(20.9723552541085,2.17092318148099,11.2827494118573));
#44745=CARTESIAN_POINT('Ctrl Pts',(21.0251066906314,1.74835589110173,11.9979016605619));
#44746=CARTESIAN_POINT('Ctrl Pts',(21.0778581271544,0.937722464374398,12.4837544055285));
#44747=CARTESIAN_POINT('Ctrl Pts',(21.1306095636773,0.107816213237538,12.5192715569468));
#44748=CARTESIAN_POINT('Ctrl Pts',(21.1833610002002,-0.722090037899322,
12.5547887083651));
#44749=CARTESIAN_POINT('Ctrl Pts',(21.2361124367231,-1.57126911344571,12.1399702662351));
#44750=CARTESIAN_POINT('Ctrl Pts',(21.288863873246,-2.05339156615543,11.4635356468258));
#44751=CARTESIAN_POINT('Ctrl Pts',(21.3217148146667,-2.35363318032772,11.0422861885773));
#44752=CARTESIAN_POINT('Ctrl Pts',(21.3545657560874,-2.51152392557026,10.5195774789631));
#44753=CARTESIAN_POINT('Ctrl Pts',(21.387416697508,-2.51442093719447,9.99847790324227));
#44754=CARTESIAN_POINT('Origin',(17.,0.,10.));
#44755=CARTESIAN_POINT('',(22.387416697508,-2.52120696757832,9.99913427807354));
#44756=CARTESIAN_POINT('',(22.112583302492,-2.51379319101573,10.0008824115804));
#44757=CARTESIAN_POINT('',(17.,-2.5175,10.));
#44758=CARTESIAN_POINT('Ctrl Pts',(22.112583302492,-2.51379319101573,10.0008824115804));
#44759=CARTESIAN_POINT('Ctrl Pts',(22.0898523213232,-2.51494301618215,10.3616815724226));
#44760=CARTESIAN_POINT('Ctrl Pts',(22.0671213401545,-2.44231188243548,10.7220393548632));
#44761=CARTESIAN_POINT('Ctrl Pts',(22.0443903589857,-2.29358750221295,11.0476400873122));
#44762=CARTESIAN_POINT('Ctrl Pts',(21.9917896460307,-1.94943128759939,11.8010976938417));
#44763=CARTESIAN_POINT('Ctrl Pts',(21.9391889330757,-1.19780753951549,12.3684366881852));
#44764=CARTESIAN_POINT('Ctrl Pts',(21.8865882201207,-0.378874755990178,
12.4928993766318));
#44765=CARTESIAN_POINT('Ctrl Pts',(21.8339875071657,0.440058027535147,12.6173620650784));
#44766=CARTESIAN_POINT('Ctrl Pts',(21.7813867942107,1.32629984650189,12.2989484476281));
#44767=CARTESIAN_POINT('Ctrl Pts',(21.7287860812557,1.8787687939542,11.6817613391465));
#44768=CARTESIAN_POINT('Ctrl Pts',(21.6761853683007,2.4312377414065,11.064574230665));
#44769=CARTESIAN_POINT('Ctrl Pts',(21.6235846553457,2.64993381734437,10.1486136311522));
#44770=CARTESIAN_POINT('Ctrl Pts',(21.5709839423907,2.43588286227969,9.34841112338628));
#44771=CARTESIAN_POINT('Ctrl Pts',(21.5183832294356,2.221831907215,8.54820861562035));
#44772=CARTESIAN_POINT('Ctrl Pts',(21.4657825164807,1.57503392114776,7.86376419960125));
#44773=CARTESIAN_POINT('Ctrl Pts',(21.4131818035257,0.788206945650621,7.60483336828132));
#44774=CARTESIAN_POINT('Ctrl Pts',(21.3605810905707,0.00137997015348126,
7.3459025369614));
#44775=CARTESIAN_POINT('Ctrl Pts',(21.3079803776156,-0.925475994773556,
7.51248529034064));
#44776=CARTESIAN_POINT('Ctrl Pts',(21.2553796646606,-1.57289850685262,8.0291921275672));
#44777=CARTESIAN_POINT('Ctrl Pts',(21.2077808772711,-2.15875608885959,8.49676409582006));
#44778=CARTESIAN_POINT('Ctrl Pts',(21.1601820898816,-2.51579739457182,9.25103791845196));
#44779=CARTESIAN_POINT('Ctrl Pts',(21.112583302492,-2.5206186296165,10.0013249946411));
#44780=CARTESIAN_POINT('Ctrl Pts',(21.387416697508,-2.51442093719447,9.99847790324227));
#44781=CARTESIAN_POINT('Ctrl Pts',(21.4073171926103,-2.51617589346499,9.68280538044796));
#44782=CARTESIAN_POINT('Ctrl Pts',(21.4272176877126,-2.46105259485335,9.36772336364112));
#44783=CARTESIAN_POINT('Ctrl Pts',(21.4471181828148,-2.34624047609594,9.07614441500762));
#44784=CARTESIAN_POINT('Ctrl Pts',(21.4998696193378,-2.0419011034537,8.30323859928707));
#44785=CARTESIAN_POINT('Ctrl Pts',(21.5526210558607,-1.31815652829618,7.69547776453441));
#44786=CARTESIAN_POINT('Ctrl Pts',(21.6053724923836,-0.504270447552835,
7.52935942940694));
#44787=CARTESIAN_POINT('Ctrl Pts',(21.6581239289065,0.309615633190516,7.36324109427946));
#44788=CARTESIAN_POINT('Ctrl Pts',(21.7108753654295,1.2136432195197,7.63876525877716));
#44789=CARTESIAN_POINT('Ctrl Pts',(21.7636268019524,1.79652982974861,8.23058368824306));
#44790=CARTESIAN_POINT('Ctrl Pts',(21.8163782384753,2.37941643997752,8.82240211770896));
#44791=CARTESIAN_POINT('Ctrl Pts',(21.8691296749983,2.64116207410616,9.73051481214307));
#44792=CARTESIAN_POINT('Ctrl Pts',(21.9218811115212,2.46268696512556,10.5417807913922));
#44793=CARTESIAN_POINT('Ctrl Pts',(21.9746325480441,2.28421185614497,11.3530467706413));
#44794=CARTESIAN_POINT('Ctrl Pts',(22.0273839845671,1.66551600405516,12.0674660347054));
#44795=CARTESIAN_POINT('Ctrl Pts',(22.08013542109,0.888071755549521,12.360017387483));
#44796=CARTESIAN_POINT('Ctrl Pts',(22.1328868576129,0.11062750704388,12.6525687402605));
#44797=CARTESIAN_POINT('Ctrl Pts',(22.1856382941358,-0.82556513787759,12.5232521817515));
#44798=CARTESIAN_POINT('Ctrl Pts',(22.2383897306588,-1.49459037849252,12.0308995825432));
#44799=CARTESIAN_POINT('Ctrl Pts',(22.2880653862752,-2.12460672765935,11.5672546133773));
#44800=CARTESIAN_POINT('Ctrl Pts',(22.3377410418916,-2.51770286914662,10.7816745100176));
#44801=CARTESIAN_POINT('Ctrl Pts',(22.387416697508,-2.52120696757832,9.99913427807354));
#44802=CARTESIAN_POINT('Origin',(17.,0.,10.));
#44803=CARTESIAN_POINT('',(23.387416697508,-2.51682157436921,10.00224693272));
#44804=CARTESIAN_POINT('',(23.112583302492,-2.51755781857958,9.99777508489969));
#44805=CARTESIAN_POINT('',(17.,-2.5175,10.));
#44806=CARTESIAN_POINT('Ctrl Pts',(23.112583302492,-2.51755781857958,9.99777508489969));
#44807=CARTESIAN_POINT('Ctrl Pts',(23.0721232657199,-2.51179213810653,10.6375515055505));
#44808=CARTESIAN_POINT('Ctrl Pts',(23.0316632289478,-2.26324677579117,11.2813147064433));
#44809=CARTESIAN_POINT('Ctrl Pts',(22.9912031921757,-1.82307654140638,11.7419774141668));
#44810=CARTESIAN_POINT('Ctrl Pts',(22.9386024792207,-1.25082624216336,12.3408692786139));
#44811=CARTESIAN_POINT('Ctrl Pts',(22.8860017662657,-0.354697089633438,
12.6302899500812));
#44812=CARTESIAN_POINT('Ctrl Pts',(22.8334010533107,0.459754356125098,12.4792578134635));
#44813=CARTESIAN_POINT('Ctrl Pts',(22.7808003403557,1.27420580188363,12.3282256768458));
#44814=CARTESIAN_POINT('Ctrl Pts',(22.7281996274007,2.00697954087078,11.736740732143));
#44815=CARTESIAN_POINT('Ctrl Pts',(22.6755989144457,2.3264479232838,10.9724882761411));
#44816=CARTESIAN_POINT('Ctrl Pts',(22.6229982014907,2.64591630569681,10.2082358201392));
#44817=CARTESIAN_POINT('Ctrl Pts',(22.5703974885357,2.5520793315357,9.27121585283808));
#44818=CARTESIAN_POINT('Ctrl Pts',(22.5177967755807,2.08740431987843,8.5854906898792));
#44819=CARTESIAN_POINT('Ctrl Pts',(22.4651960626257,1.62272930822116,7.8997655269203));
#44820=CARTESIAN_POINT('Ctrl Pts',(22.4125953496707,0.787216259067707,7.46533516830362));
#44821=CARTESIAN_POINT('Ctrl Pts',(22.3599946367157,-0.0410109803468926,
7.47880752793945));
#44822=CARTESIAN_POINT('Ctrl Pts',(22.3073939237607,-0.869238219761481,
7.49227988757529));
#44823=CARTESIAN_POINT('Ctrl Pts',(22.2547932108057,-1.69017964943722,7.95365496546363));
#44824=CARTESIAN_POINT('Ctrl Pts',(22.2021924978507,-2.13230602370348,8.65413061376549));
#44825=CARTESIAN_POINT('Ctrl Pts',(22.1723227660645,-2.3833709898048,9.0519012629098));
#44826=CARTESIAN_POINT('Ctrl Pts',(22.1424530342782,-2.51228225890651,9.52677290952939));
#44827=CARTESIAN_POINT('Ctrl Pts',(22.112583302492,-2.51379319101573,10.0008824115804));
#44828=CARTESIAN_POINT('Ctrl Pts',(22.387416697508,-2.52120696757832,9.99913427807354));
#44829=CARTESIAN_POINT('Ctrl Pts',(22.3904924784145,-2.52142393178175,9.9506815244235));
#44830=CARTESIAN_POINT('Ctrl Pts',(22.393568259321,-2.52014729821555,9.90224042487485));
#44831=CARTESIAN_POINT('Ctrl Pts',(22.3966440402275,-2.5173408263703,9.85388812043869));
#44832=CARTESIAN_POINT('Ctrl Pts',(22.4493954767505,-2.46920819732477,9.0246178974504));
#44833=CARTESIAN_POINT('Ctrl Pts',(22.5021469132734,-1.97108510292534,8.22146609138159));
#44834=CARTESIAN_POINT('Ctrl Pts',(22.5548983497963,-1.24958996734608,7.80982228635205));
#44835=CARTESIAN_POINT('Ctrl Pts',(22.6076497863193,-0.528094831766828,
7.39817848132251));
#44836=CARTESIAN_POINT('Ctrl Pts',(22.6604012228422,0.41677234499225,7.37804267733221));
#44837=CARTESIAN_POINT('Ctrl Pts',(22.7131526593651,1.1551493388732,7.75857555916865));
#44838=CARTESIAN_POINT('Ctrl Pts',(22.765904095888,1.89352633275415,8.13910844100509));
#44839=CARTESIAN_POINT('Ctrl Pts',(22.818655532411,2.42541314375697,8.92031000866826));
#44840=CARTESIAN_POINT('Ctrl Pts',(22.8714069689339,2.50883071324478,9.74677679829437));
#44841=CARTESIAN_POINT('Ctrl Pts',(22.9241584054568,2.59224828273258,10.5732435879205));
#44842=CARTESIAN_POINT('Ctrl Pts',(22.9769098419798,2.22719661070537,11.4449755995095));
#44843=CARTESIAN_POINT('Ctrl Pts',(23.0296612785027,1.57975402480848,11.9653830831136));
#44844=CARTESIAN_POINT('Ctrl Pts',(23.0824127150256,0.932311438911595,12.4857905667176));
#44845=CARTESIAN_POINT('Ctrl Pts',(23.1351641515485,0.00247793914503677,
12.6548735223365));
#44846=CARTESIAN_POINT('Ctrl Pts',(23.1879155880715,-0.786723799438258,
12.3957085041788));
#44847=CARTESIAN_POINT('Ctrl Pts',(23.2406670245944,-1.57592553802155,12.1365434860212));
#44848=CARTESIAN_POINT('Ctrl Pts',(23.2934184611173,-2.22449551542159,11.4491304940869));
#44849=CARTESIAN_POINT('Ctrl Pts',(23.3461698976402,-2.4373701819469,10.6462044936153));
#44850=CARTESIAN_POINT('Ctrl Pts',(23.3599188309295,-2.49285302340009,10.4369329221786));
#44851=CARTESIAN_POINT('Ctrl Pts',(23.3736677642188,-2.51873854991203,10.2198144109009));
#44852=CARTESIAN_POINT('Ctrl Pts',(23.387416697508,-2.51682157436921,10.00224693272));
#44853=CARTESIAN_POINT('Origin',(17.,0.,10.));
#44854=CARTESIAN_POINT('',(24.387416697508,-2.51385573226095,9.99896352468483));
#44855=CARTESIAN_POINT('',(24.112583302492,-2.52041830912221,10.0014523913097));
#44856=CARTESIAN_POINT('',(17.,-2.5175,10.));
#44857=CARTESIAN_POINT('Ctrl Pts',(24.112583302492,-2.52041830912221,10.0014523913097));
#44858=CARTESIAN_POINT('Ctrl Pts',(24.1069949230716,-2.5210272662623,10.0895589550511));
#44859=CARTESIAN_POINT('Ctrl Pts',(24.1014065436512,-2.51680247988567,10.1776065034683));
#44860=CARTESIAN_POINT('Ctrl Pts',(24.0958181642308,-2.50754945116842,10.265122427668));
#44861=CARTESIAN_POINT('Ctrl Pts',(24.0432174512758,-2.42045516659928,11.0888674996318));
#44862=CARTESIAN_POINT('Ctrl Pts',(23.9906167383208,-1.88788141364161,11.865513076825));
#44863=CARTESIAN_POINT('Ctrl Pts',(23.9380160253658,-1.15085300692774,12.243575552908));
#44864=CARTESIAN_POINT('Ctrl Pts',(23.8854153124108,-0.413824600213868,
12.6216380289909));
#44865=CARTESIAN_POINT('Ctrl Pts',(23.8328145994558,0.527658460256214,12.6011174039635));
#44866=CARTESIAN_POINT('Ctrl Pts',(23.7802138865008,1.24751435885636,12.1913011667028));
#44867=CARTESIAN_POINT('Ctrl Pts',(23.7276131735458,1.96737025745651,11.7814849294421));
#44868=CARTESIAN_POINT('Ctrl Pts',(23.6750124605908,2.46559899418673,10.982373079948));
#44869=CARTESIAN_POINT('Ctrl Pts',(23.6224117476358,2.51671957482837,10.1556152639013));
#44870=CARTESIAN_POINT('Ctrl Pts',(23.5698110346808,2.56784015547002,9.3288574478546));
#44871=CARTESIAN_POINT('Ctrl Pts',(23.5172103217258,2.17185258002309,8.47445366525525));
#44872=CARTESIAN_POINT('Ctrl Pts',(23.4646096087708,1.50796700170717,7.97907720145607));
#44873=CARTESIAN_POINT('Ctrl Pts',(23.4120088958157,0.844081423391251,7.48370073765689));
#44874=CARTESIAN_POINT('Ctrl Pts',(23.3594081828607,-0.0877021577936639,
7.3473515926579));
#44875=CARTESIAN_POINT('Ctrl Pts',(23.3068074699057,-0.865691280649959,
7.63173651802616));
#44876=CARTESIAN_POINT('Ctrl Pts',(23.2542067569507,-1.64368040350625,7.91612144339442));
#44877=CARTESIAN_POINT('Ctrl Pts',(23.2016060439957,-2.26787506803393,8.62124043912995));
#44878=CARTESIAN_POINT('Ctrl Pts',(23.1490053310407,-2.45578667731971,9.42798146571124));
#44879=CARTESIAN_POINT('Ctrl Pts',(23.1368646548578,-2.499158218715,9.61418391463194));
#44880=CARTESIAN_POINT('Ctrl Pts',(23.1247239786749,-2.51928790251381,9.80580001586207));
#44881=CARTESIAN_POINT('Ctrl Pts',(23.112583302492,-2.51755781857958,9.99777508489969));
#44882=CARTESIAN_POINT('Ctrl Pts',(23.387416697508,-2.51682157436921,10.00224693272));
#44883=CARTESIAN_POINT('Ctrl Pts',(23.4264192007417,-2.51138356378068,9.38505895945965));
#44884=CARTESIAN_POINT('Ctrl Pts',(23.4654217039754,-2.28221214670945,8.76425804178077));
#44885=CARTESIAN_POINT('Ctrl Pts',(23.504424207209,-1.87027955385458,8.30872610392666));
#44886=CARTESIAN_POINT('Ctrl Pts',(23.557175643732,-1.31313490358636,7.69261272371846));
#44887=CARTESIAN_POINT('Ctrl Pts',(23.6099270802549,-0.421666247399317,
7.37882497231092));
#44888=CARTESIAN_POINT('Ctrl Pts',(23.6626785167778,0.398558037255763,7.51011936658926));
#44889=CARTESIAN_POINT('Ctrl Pts',(23.7154299533007,1.21878232191084,7.64141376086759));
#44890=CARTESIAN_POINT('Ctrl Pts',(23.7681813898237,1.96776223503395,8.21779030083179));
#44891=CARTESIAN_POINT('Ctrl Pts',(23.8209328263466,2.30475246126436,8.97702867998691));
#44892=CARTESIAN_POINT('Ctrl Pts',(23.8736842628695,2.64174268749477,9.73626705914203));
#44893=CARTESIAN_POINT('Ctrl Pts',(23.9264356993925,2.56674322683247,10.6783672774881));
#44894=CARTESIAN_POINT('Ctrl Pts',(23.9791871359154,2.1138764852266,11.3747276544192));
#44895=CARTESIAN_POINT('Ctrl Pts',(24.0319385724383,1.66100974362073,12.0710880313502));
#44896=CARTESIAN_POINT('Ctrl Pts',(24.0846900089612,0.830275721071305,12.5217085668663));
#44897=CARTESIAN_POINT('Ctrl Pts',(24.1374414454842,-0.000391089040924892,
12.5215785240049));
#44898=CARTESIAN_POINT('Ctrl Pts',(24.1901928820071,-0.831057899153163,
12.5214484811436));
#44899=CARTESIAN_POINT('Ctrl Pts',(24.24294431853,-1.6616574968282,12.0705678599046));
#44900=CARTESIAN_POINT('Ctrl Pts',(24.295695755053,-2.11430637366214,11.3740688240468));
#44901=CARTESIAN_POINT('Ctrl Pts',(24.326269402538,-2.37665235145929,10.9703923102003));
#44902=CARTESIAN_POINT('Ctrl Pts',(24.356843050023,-2.51204002762718,10.4842095460693));
#44903=CARTESIAN_POINT('Ctrl Pts',(24.387416697508,-2.51385573226095,9.99896352468483));
#44904=CARTESIAN_POINT('Origin',(17.,0.,10.));
#44905=CARTESIAN_POINT('',(25.387416697508,-2.52031926711485,9.99879747833012));
#44906=CARTESIAN_POINT('',(25.112583302492,-2.51369118594155,10.0007624228313));
#44907=CARTESIAN_POINT('',(17.,-2.5175,10.));
#44908=CARTESIAN_POINT('',(25.8782388507408,2.51331533716111,9.85490600980483));
#44909=CARTESIAN_POINT('Ctrl Pts',(25.387416697508,-2.52031926711485,9.99879747833012));
#44910=CARTESIAN_POINT('Ctrl Pts',(25.3927697723502,-2.5208983757328,9.91440472807825));
#44911=CARTESIAN_POINT('Ctrl Pts',(25.3981228471923,-2.51703766949288,9.83006045553805));
#44912=CARTESIAN_POINT('Ctrl Pts',(25.4034759220345,-2.50856460058327,9.74617830516996));
#44913=CARTESIAN_POINT('Ctrl Pts',(25.4562273585574,-2.42506743868645,8.91956854142917));
#44914=CARTESIAN_POINT('Ctrl Pts',(25.5089787950803,-1.89366580395695,8.13783525482216));
#44915=CARTESIAN_POINT('Ctrl Pts',(25.5617302316032,-1.15478948854362,7.75787973679709));
#44916=CARTESIAN_POINT('Ctrl Pts',(25.6144816681262,-0.415913173130291,
7.37792421877201));
#44917=CARTESIAN_POINT('Ctrl Pts',(25.6672331046491,0.530437822966877,7.39974646932889));
#44918=CARTESIAN_POINT('Ctrl Pts',(25.719984541172,1.25072220675159,7.81073417797026));
#44919=CARTESIAN_POINT('Ctrl Pts',(25.772735977695,1.9710065905363,8.22172188661162));
#44920=CARTESIAN_POINT('Ctrl Pts',(25.8254874142179,2.46522436200856,9.02187505333746));
#44921=CARTESIAN_POINT('Ctrl Pts',(25.8782388507408,2.51331533716111,9.85490600980485));
#44922=CARTESIAN_POINT('',(25.9598438343188,-1.44740009951425,12.0606038454663));
#44923=CARTESIAN_POINT('Ctrl Pts',(25.9598438343188,-1.44447502497693,12.0618676369297));
#44924=CARTESIAN_POINT('Ctrl Pts',(25.9680986111512,-1.29612166908485,12.1657990016882));
#44925=CARTESIAN_POINT('Ctrl Pts',(25.9758261020123,-1.13376695951384,12.2552771340403));
#44926=CARTESIAN_POINT('Ctrl Pts',(25.9936363108284,-0.65357955075694,12.454243785592));
#44927=CARTESIAN_POINT('Ctrl Pts',(26.,-0.316315187408128,12.5175));
#44928=CARTESIAN_POINT('Ctrl Pts',(26.,0.316315187408128,12.5175));
#44929=CARTESIAN_POINT('Ctrl Pts',(25.9936363108284,0.65357955075694,12.454243785592));
#44930=CARTESIAN_POINT('Ctrl Pts',(25.9706329474538,1.27378145661654,12.1972618359521));
#44931=CARTESIAN_POINT('Ctrl Pts',(25.954319860997,1.55673560227871,12.0035470409956));
#44932=CARTESIAN_POINT('Ctrl Pts',(25.9236560318941,2.00354770900701,11.5567349342673));
#44933=CARTESIAN_POINT('Ctrl Pts',(25.9073094472621,2.19726198315605,11.2737810818527));
#44934=CARTESIAN_POINT('Ctrl Pts',(25.8842294016963,2.45424354267521,10.6535801565147));
#44935=CARTESIAN_POINT('Ctrl Pts',(25.8778320913866,2.5175,10.3163161332307));
#44936=CARTESIAN_POINT('Ctrl Pts',(25.8778320913866,2.5175,9.95206425392299));
#44937=CARTESIAN_POINT('Ctrl Pts',(25.8779655959498,2.51612889288328,9.90364236848503));
#44938=CARTESIAN_POINT('Ctrl Pts',(25.8782388507408,2.51331533716111,9.85490600980483));
#44939=CARTESIAN_POINT('Ctrl Pts',(25.9598438343188,-1.44740009951425,12.0606038454663));
#44940=CARTESIAN_POINT('Ctrl Pts',(25.9171097867945,-0.891269470133681,
12.4428005051404));
#44941=CARTESIAN_POINT('Ctrl Pts',(25.8743757392702,-0.173138502655974,
12.6040916696052));
#44942=CARTESIAN_POINT('Ctrl Pts',(25.8316416917459,0.487362244993046,12.4744336608074));
#44943=CARTESIAN_POINT('Ctrl Pts',(25.7790409787909,1.30036293756482,12.3148395175376));
#44944=CARTESIAN_POINT('Ctrl Pts',(25.7264402658359,2.02604930930844,11.7144344675171));
#44945=CARTESIAN_POINT('Ctrl Pts',(25.6738395528809,2.33692684617734,10.9464895031126));
#44946=CARTESIAN_POINT('Ctrl Pts',(25.6212388399259,2.64780438304624,10.1785445387081));
#44947=CARTESIAN_POINT('Ctrl Pts',(25.5686381269709,2.54387308504042,9.24305965991953));
#44948=CARTESIAN_POINT('Ctrl Pts',(25.5160374140159,2.07170855144438,8.56261910495375));
#44949=CARTESIAN_POINT('Ctrl Pts',(25.4634367010609,1.59954401784833,7.88217854998797));
#44950=CARTESIAN_POINT('Ctrl Pts',(25.4108359881058,0.759146248662072,7.45678231884493));
#44951=CARTESIAN_POINT('Ctrl Pts',(25.3582352751508,-0.0689135765338292,
7.47935431018827));
#44952=CARTESIAN_POINT('Ctrl Pts',(25.3056345621958,-0.896973401729732,
7.50192630153161));
#44953=CARTESIAN_POINT('Ctrl Pts',(25.2530338492408,-1.71269528293527,7.97246651536133));
#44954=CARTESIAN_POINT('Ctrl Pts',(25.2004331362858,-2.14703481200095,8.67781519460184));
#44955=CARTESIAN_POINT('Ctrl Pts',(25.1711498583546,-2.38883543468551,9.07048898650142));
#44956=CARTESIAN_POINT('Ctrl Pts',(25.1418665804233,-2.51243626586703,9.53593570955259));
#44957=CARTESIAN_POINT('Ctrl Pts',(25.112583302492,-2.51369118594155,10.0007624228313));
#44958=CARTESIAN_POINT('Origin',(28.2084234471774,0.,10.));
#44959=CARTESIAN_POINT('',(8.79157655282254,-3.07807615307783,10.0009342588364));
#44960=CARTESIAN_POINT('',(8.70842344717745,-3.06851316107703,10.0005037120289));
#44961=CARTESIAN_POINT('',(28.2084234471774,-3.0735,10.0000000000003));
#44962=CARTESIAN_POINT('',(8.,0.793799282532897,7.03077704625431));
#44963=CARTESIAN_POINT('Ctrl Pts',(8.70842344717745,-3.06851316107703,10.0005037120289));
#44964=CARTESIAN_POINT('Ctrl Pts',(8.68328804421001,-3.06903018828163,10.4877872520226));
#44965=CARTESIAN_POINT('Ctrl Pts',(8.60540120471965,-2.73029264571413,11.9969233978531));
#44966=CARTESIAN_POINT('Ctrl Pts',(8.47476292870636,-0.372557211312175,
13.6086112664375));
#44967=CARTESIAN_POINT('Ctrl Pts',(8.31650861913757,2.82494041479191,12.281332723926));
#44968=CARTESIAN_POINT('Ctrl Pts',(8.15825430956879,3.44737991946778,8.87067395584943));
#44969=CARTESIAN_POINT('Ctrl Pts',(8.05275143652293,1.7779394739971,7.29387947745118));
#44970=CARTESIAN_POINT('Ctrl Pts',(8.,0.793799282532855,7.0307770462543));
#44971=CARTESIAN_POINT('',(8.,0.,6.9265));
#44972=CARTESIAN_POINT('Origin',(8.,0.,10.));
#44973=CARTESIAN_POINT('',(8.,-0.7937992825328,7.03077704625429));
#44974=CARTESIAN_POINT('Origin',(8.,0.,10.));
#44975=CARTESIAN_POINT('Ctrl Pts',(8.79157655282254,-3.07807615307782,10.0009342588364));
#44976=CARTESIAN_POINT('Ctrl Pts',(8.7889204426769,-3.07827713215033,10.0520138798573));
#44977=CARTESIAN_POINT('Ctrl Pts',(8.73366361957626,-3.05408484518725,11.114459619653));
#44978=CARTESIAN_POINT('Ctrl Pts',(8.62580608352061,-1.83029914535168,13.1291833116438));
#44979=CARTESIAN_POINT('Ctrl Pts',(8.46800394465562,1.61680800983869,13.245137596954));
#44980=CARTESIAN_POINT('Ctrl Pts',(8.31020180579059,3.60054044813756,10.4226504132617));
#44981=CARTESIAN_POINT('Ctrl Pts',(8.15420049090541,2.33978014667001,7.25641897300791));
#44982=CARTESIAN_POINT('Ctrl Pts',(8.0507998889752,0.148780815319225,6.77559856235343));
#44983=CARTESIAN_POINT('Ctrl Pts',(8.,-0.795613156383193,7.02571472931219));
#44984=CARTESIAN_POINT('Origin',(28.2084234471774,0.,10.));
#44985=CARTESIAN_POINT('',(9.79157655282253,-3.06960368404499,10.0017022409322));
#44986=CARTESIAN_POINT('',(9.70842344717744,-3.07437462459256,9.99730908511578));
#44987=CARTESIAN_POINT('',(28.2084234471774,-3.0735,10.0000000000003));
#44988=CARTESIAN_POINT('Ctrl Pts',(9.70842344717744,-3.07437462459256,9.99730908511578));
#44989=CARTESIAN_POINT('Ctrl Pts',(9.66646333001425,-3.06699116075788,10.8067972882056));
#44990=CARTESIAN_POINT('Ctrl Pts',(9.57175177632812,-2.325029441416,12.6459346938779));
#44991=CARTESIAN_POINT('Ctrl Pts',(9.42428878611906,0.772313381832412,13.5456136953941));
#44992=CARTESIAN_POINT('Ctrl Pts',(9.26603447655028,3.39364577165048,11.2850883447562));
#44993=CARTESIAN_POINT('Ctrl Pts',(9.1077801669815,2.92704762252235,7.85513439723516));
#44994=CARTESIAN_POINT('Ctrl Pts',(8.94952585741271,-0.20266861905204,6.37704123220448));
#44995=CARTESIAN_POINT('Ctrl Pts',(8.81640695081136,-2.68045467182773,7.9061860654363));
#44996=CARTESIAN_POINT('Ctrl Pts',(8.73603948073294,-3.06794510809417,9.46512981693207));
#44997=CARTESIAN_POINT('Ctrl Pts',(8.70842344717745,-3.06851316107703,10.0005037120289));
#44998=CARTESIAN_POINT('Ctrl Pts',(9.79157655282253,-3.069603684045,10.0017022409322));
#44999=CARTESIAN_POINT('Ctrl Pts',(9.77119138707358,-3.07161716533022,10.3965250682061));
#45000=CARTESIAN_POINT('Ctrl Pts',(9.69820550836963,-2.81824968568554,11.8076406238949));
#45001=CARTESIAN_POINT('Ctrl Pts',(9.57261891671066,-0.702623662064588,
13.5565683145601));
#45002=CARTESIAN_POINT('Ctrl Pts',(9.41481677784566,2.59166910069841,12.5349881811848));
#45003=CARTESIAN_POINT('Ctrl Pts',(9.25701463898065,3.54016602667422,9.21889196466343));
#45004=CARTESIAN_POINT('Ctrl Pts',(9.09921250011564,1.28435171110455,6.60984400954655));
#45005=CARTESIAN_POINT('Ctrl Pts',(8.94406647139626,-2.07642740645684,7.06150941801092));
#45006=CARTESIAN_POINT('Ctrl Pts',(8.8415211556319,-3.07429701012116,9.04045022629949));
#45007=CARTESIAN_POINT('Ctrl Pts',(8.79157655282254,-3.07807615307782,10.0009342588364));
#45008=CARTESIAN_POINT('Origin',(28.2084234471774,0.,10.));
#45009=CARTESIAN_POINT('',(10.7915765528225,-3.07225467518151,9.99733889552176));
#45010=CARTESIAN_POINT('',(10.7084234471774,-3.07691672930537,10.0019090684753));
#45011=CARTESIAN_POINT('',(28.2084234471774,-3.0735,10.0000000000003));
#45012=CARTESIAN_POINT('Ctrl Pts',(10.7084234471774,-3.07691672930537,10.0019090684753));
#45013=CARTESIAN_POINT('Ctrl Pts',(10.7023900523414,-3.07776457748099,10.1180544945408));
#45014=CARTESIAN_POINT('Ctrl Pts',(10.6436052209824,-3.01920281481477,11.2488245350352));
#45015=CARTESIAN_POINT('Ctrl Pts',(10.5320689531006,-1.61985329993334,13.2471660282134));
#45016=CARTESIAN_POINT('Ctrl Pts',(10.3738146435318,1.83951385849227,13.127969994097));
#45017=CARTESIAN_POINT('Ctrl Pts',(10.215560333963,3.62512807421833,10.1626691840488));
#45018=CARTESIAN_POINT('Ctrl Pts',(10.0573060243942,2.11227555931511,7.04935467956235));
#45019=CARTESIAN_POINT('Ctrl Pts',(9.89905171482542,-1.32251038305822,6.62080587867383));
#45020=CARTESIAN_POINT('Ctrl Pts',(9.78275752241983,-2.96230896709799,8.56533388251318));
#45021=CARTESIAN_POINT('Ctrl Pts',(9.71921476653717,-3.07627350671224,9.78912459212447));
#45022=CARTESIAN_POINT('Ctrl Pts',(9.70842344717744,-3.07437462459256,9.99730908511578));
#45023=CARTESIAN_POINT('Ctrl Pts',(10.7915765528225,-3.07225467518151,9.99733889552176));
#45024=CARTESIAN_POINT('Ctrl Pts',(10.7534623314703,-3.06599829486339,10.7339319007572));
#45025=CARTESIAN_POINT('Ctrl Pts',(10.662747397163,-2.43255612271171,12.4967446704248));
#45026=CARTESIAN_POINT('Ctrl Pts',(10.5194317499007,0.502799430185017,13.5902749971079));
#45027=CARTESIAN_POINT('Ctrl Pts',(10.3616296110357,3.27976499314249,11.5446760958796));
#45028=CARTESIAN_POINT('Ctrl Pts',(10.2038274721707,3.08811778788391,8.10094449581088));
#45029=CARTESIAN_POINT('Ctrl Pts',(10.0460253333057,0.101323344801963,6.37610534685446));
#45030=CARTESIAN_POINT('Ctrl Pts',(9.90860836018963,-2.5794949399918,7.73044878286791));
#45031=CARTESIAN_POINT('Ctrl Pts',(9.82379210002858,-3.06642169366084,9.37774688110278));
#45032=CARTESIAN_POINT('Ctrl Pts',(9.79157655282253,-3.069603684045,10.0017022409322));
#45033=CARTESIAN_POINT('Origin',(28.2084234471774,0.,10.));
#45034=CARTESIAN_POINT('',(11.7915765528225,-3.07791877256789,10.001096933631));
#45035=CARTESIAN_POINT('',(11.7084234471774,-3.06890348767814,10.0010756969218));
#45036=CARTESIAN_POINT('',(28.2084234471774,-3.0735,10.0000000000003));
#45037=CARTESIAN_POINT('Ctrl Pts',(11.7084234471774,-3.06890348767814,10.0010756969218));
#45038=CARTESIAN_POINT('Ctrl Pts',(11.6855653381456,-3.07030490094272,10.4440452179421));
#45039=CARTESIAN_POINT('Ctrl Pts',(11.6099557925909,-2.77375822075196,11.907501720394));
#45040=CARTESIAN_POINT('Ctrl Pts',(11.4815948105133,-0.526448883152259,
13.5903847416995));
#45041=CARTESIAN_POINT('Ctrl Pts',(11.3233405009445,2.72323490185543,12.3983332956597));
#45042=CARTESIAN_POINT('Ctrl Pts',(11.1650861913757,3.49507659867442,9.02406424380673));
#45043=CARTESIAN_POINT('Ctrl Pts',(11.0068318818069,1.08678570881093,6.53778857091659));
#45044=CARTESIAN_POINT('Ctrl Pts',(10.8546109670742,-2.18084464523734,7.17642888325995));
#45045=CARTESIAN_POINT('Ctrl Pts',(10.7551414888643,-3.07035163494491,9.10256682349923));
#45046=CARTESIAN_POINT('Ctrl Pts',(10.7084234471774,-3.07691672930537,10.0019090684753));
#45047=CARTESIAN_POINT('Ctrl Pts',(11.7915765528225,-3.07791877256789,10.001096933631));
#45048=CARTESIAN_POINT('Ctrl Pts',(11.788333988822,-3.07820828582192,10.0634639827233));
#45049=CARTESIAN_POINT('Ctrl Pts',(11.7324907118664,-3.04835338254568,11.137263907321));
#45050=CARTESIAN_POINT('Ctrl Pts',(11.6240467219557,-1.7956016590295,13.1493962879665));
#45051=CARTESIAN_POINT('Ctrl Pts',(11.4662445830908,1.65259091012735,13.2267360548792));
#45052=CARTESIAN_POINT('Ctrl Pts',(11.3084424442257,3.60497432328288,10.3834611087496));
#45053=CARTESIAN_POINT('Ctrl Pts',(11.1506403053608,2.29438831935563,7.19310410595708));
#45054=CARTESIAN_POINT('Ctrl Pts',(10.9928381664957,-1.09291675350356,6.5433520284504));
#45055=CARTESIAN_POINT('Ctrl Pts',(10.873150248983,-2.91177954598531,8.42356662734618));
#45056=CARTESIAN_POINT('Ctrl Pts',(10.8060630444253,-3.07463260650809,9.71737388491982));
#45057=CARTESIAN_POINT('Ctrl Pts',(10.7915765528225,-3.07225467518151,9.99733889552176));
#45058=CARTESIAN_POINT('Origin',(28.2084234471774,0.,10.));
#45059=CARTESIAN_POINT('',(12.7915765528225,-3.06941961343749,10.0015551958711));
#45060=CARTESIAN_POINT('',(12.7084234471775,-3.07305765256541,9.99723902520708));
#45061=CARTESIAN_POINT('',(28.2084234471774,-3.0735,10.0000000000003));
#45062=CARTESIAN_POINT('Ctrl Pts',(12.7084234471775,-3.0730576525654,9.99723902520708));
#45063=CARTESIAN_POINT('Ctrl Pts',(12.6687406239499,-3.06618522061749,10.763633229918));
#45064=CARTESIAN_POINT('Ctrl Pts',(12.5763063641994,-2.38924445855591,12.5596491752114));
#45065=CARTESIAN_POINT('Ctrl Pts',(12.431120667926,0.619461886626625,13.5755108676666));
#45066=CARTESIAN_POINT('Ctrl Pts',(12.2728663583572,3.33534949119645,11.4294945832771));
#45067=CARTESIAN_POINT('Ctrl Pts',(12.1146120487884,3.01643851828712,7.98279657484158));
#45068=CARTESIAN_POINT('Ctrl Pts',(11.9563577392196,-0.047097373778369,
6.37153023510597));
#45069=CARTESIAN_POINT('Ctrl Pts',(11.8209615386826,-2.63147522942551,7.81763283424629));
#45070=CARTESIAN_POINT('Ctrl Pts',(11.7383167746686,-3.0670707505252,9.42176999223617));
#45071=CARTESIAN_POINT('Ctrl Pts',(11.7084234471774,-3.06890348767814,10.0010756969218));
#45072=CARTESIAN_POINT('Ctrl Pts',(12.7915765528225,-3.06941961343749,10.0015551958711));
#45073=CARTESIAN_POINT('Ctrl Pts',(12.7706049332186,-3.07130561059382,10.4077975568445));
#45074=CARTESIAN_POINT('Ctrl Pts',(12.6970326006597,-2.808064557181,11.8306255759708));
#45075=CARTESIAN_POINT('Ctrl Pts',(12.5708595551458,-0.663265918297566,
13.5641212961923));
#45076=CARTESIAN_POINT('Ctrl Pts',(12.4130574162808,2.61953312462283,12.5061780665257));
#45077=CARTESIAN_POINT('Ctrl Pts',(12.2552552774158,3.53131487113802,9.17981857309606));
#45078=CARTESIAN_POINT('Ctrl Pts',(12.0974531385508,1.2467985598852,6.59582966877859));
#45079=CARTESIAN_POINT('Ctrl Pts',(11.9428935636864,-2.09610024567504,7.08283935894699));
#45080=CARTESIAN_POINT('Ctrl Pts',(11.840934701777,-3.07351181612411,9.05174879481766));
#45081=CARTESIAN_POINT('Ctrl Pts',(11.7915765528225,-3.07791877256789,10.001096933631));
#45082=CARTESIAN_POINT('Origin',(28.2084234471774,0.,10.));
#45083=CARTESIAN_POINT('',(13.7915765528225,-3.07257624006984,9.99730578639428));
#45084=CARTESIAN_POINT('',(13.7084234471775,-3.0778195052343,10.0012720431918));
#45085=CARTESIAN_POINT('',(28.2084234471774,-3.0735,10.0000000000003));
#45086=CARTESIAN_POINT('Ctrl Pts',(13.7084234471775,-3.0778195052343,10.0012720431918));
#45087=CARTESIAN_POINT('Ctrl Pts',(13.7046673462771,-3.07819893618978,10.0735226333015));
#45088=CARTESIAN_POINT('Ctrl Pts',(13.6481598088537,-3.04321810478186,11.1601013791998));
#45089=CARTESIAN_POINT('Ctrl Pts',(13.5389008349074,-1.75770622879056,13.1746621562634));
#45090=CARTESIAN_POINT('Ctrl Pts',(13.3806465253387,1.70358963251637,13.2040276773368));
#45091=CARTESIAN_POINT('Ctrl Pts',(13.2223922157699,3.6148076361298,10.3180829245743));
#45092=CARTESIAN_POINT('Ctrl Pts',(13.0641379062011,2.23695110582196,7.14271794474384));
#45093=CARTESIAN_POINT('Ctrl Pts',(12.9058835966323,-1.17628314204709,6.5671631319018));
#45094=CARTESIAN_POINT('Ctrl Pts',(12.7873121102911,-2.93172787836758,8.47620309413993));
#45095=CARTESIAN_POINT('Ctrl Pts',(12.7214920604728,-3.0753209279128,9.74484494941923));
#45096=CARTESIAN_POINT('Ctrl Pts',(12.7084234471775,-3.0730576525654,9.99723902520708));
#45097=CARTESIAN_POINT('Ctrl Pts',(13.7915765528225,-3.07257624006985,9.99730578639428));
#45098=CARTESIAN_POINT('Ctrl Pts',(13.7528758776153,-3.06608888043261,10.7450332734399));
#45099=CARTESIAN_POINT('Ctrl Pts',(13.6615744894531,-2.41686838919438,12.519140261949));
#45100=CARTESIAN_POINT('Ctrl Pts',(13.5176723883359,0.542456216386849,13.5844976699054));
#45101=CARTESIAN_POINT('Ctrl Pts',(13.3598702494708,3.2966397172568,11.5083265120178));
#45102=CARTESIAN_POINT('Ctrl Pts',(13.2020681106059,3.06693661782036,8.06692419328139));
#45103=CARTESIAN_POINT('Ctrl Pts',(13.0442659717408,0.0612580212745303,
6.37520624764731));
#45104=CARTESIAN_POINT('Ctrl Pts',(12.9074354524797,-2.59304903354642,7.75319630627082));
#45105=CARTESIAN_POINT('Ctrl Pts',(12.8232056461736,-3.06657517980556,9.38886634297939));
#45106=CARTESIAN_POINT('Ctrl Pts',(12.7915765528225,-3.06941961343749,10.0015551958711));
#45107=CARTESIAN_POINT('Origin',(28.2084234471774,0.,10.));
#45108=CARTESIAN_POINT('',(14.7915765528225,-3.07773737838628,10.0012785594934));
#45109=CARTESIAN_POINT('',(14.7084234471774,-3.0695085210094,10.001693524509));
#45110=CARTESIAN_POINT('',(28.2084234471774,-3.0735,10.0000000000003));
#45111=CARTESIAN_POINT('Ctrl Pts',(14.7084234471774,-3.0695085210094,10.001693524509));
#45112=CARTESIAN_POINT('Ctrl Pts',(14.6878426320813,-3.07151848242124,10.4003342894936));
#45113=CARTESIAN_POINT('Ctrl Pts',(14.6145103804622,-2.81450704047269,11.8182548620302));
#45114=CARTESIAN_POINT('Ctrl Pts',(14.4884266923202,-0.680037386513999,
13.5644859581834));
#45115=CARTESIAN_POINT('Ctrl Pts',(14.3301723827514,2.61780712972438,12.5129856395747));
#45116=CARTESIAN_POINT('Ctrl Pts',(14.1719180731826,3.53373713437049,9.17494675425479));
#45117=CARTESIAN_POINT('Ctrl Pts',(14.0136637636138,1.23435778144942,6.58761493079715));
#45118=CARTESIAN_POINT('Ctrl Pts',(13.8591655549454,-2.10691859834803,7.09289144011877));
#45119=CARTESIAN_POINT('Ctrl Pts',(13.7574187828,-3.07287013153473,9.05882081378745));
#45120=CARTESIAN_POINT('Ctrl Pts',(13.7084234471775,-3.0778195052343,10.0012720431918));
#45121=CARTESIAN_POINT('Ctrl Pts',(14.7915765528225,-3.07773737838628,10.0012785594934));
#45122=CARTESIAN_POINT('Ctrl Pts',(14.787747534967,-3.07812719640924,10.0749369260762));
#45123=CARTESIAN_POINT('Ctrl Pts',(14.7313178041565,-3.04249024488253,11.1600855874984));
#45124=CARTESIAN_POINT('Ctrl Pts',(14.6222873603909,-1.76067798849733,13.1690527469692));
#45125=CARTESIAN_POINT('Ctrl Pts',(14.4644852215259,1.68815882569895,13.2082708849888));
#45126=CARTESIAN_POINT('Ctrl Pts',(14.3066830826609,3.60899290643803,10.3435876795407));
#45127=CARTESIAN_POINT('Ctrl Pts',(14.1488809437959,2.26322023068206,7.16791305223806));
#45128=CARTESIAN_POINT('Ctrl Pts',(13.9910788049309,-1.13106034981207,6.55564450479696));
#45129=CARTESIAN_POINT('Ctrl Pts',(13.8719773412731,-2.92021801474013,8.44653952308092));
#45130=CARTESIAN_POINT('Ctrl Pts',(13.8054765905703,-3.07490629098906,9.72874612330486));
#45131=CARTESIAN_POINT('Ctrl Pts',(13.7915765528225,-3.07257624006985,9.99730578639428));
#45132=CARTESIAN_POINT('Origin',(28.2084234471774,0.,10.));
#45133=CARTESIAN_POINT('',(15.7915765528225,-3.06925303971756,10.0014017874572));
#45134=CARTESIAN_POINT('',(15.7084234471775,-3.07179824204593,9.99736628792378));
#45135=CARTESIAN_POINT('',(28.2084234471774,-3.0735,10.0000000000003));
#45136=CARTESIAN_POINT('Ctrl Pts',(15.7084234471775,-3.07179824204593,9.99736628792378));
#45137=CARTESIAN_POINT('Ctrl Pts',(15.6710179178855,-3.0658222301893,10.7205329315404));
#45138=CARTESIAN_POINT('Ctrl Pts',(15.5808609520707,-2.45041977337874,12.4727067956687));
#45139=CARTESIAN_POINT('Ctrl Pts',(15.4379525497329,0.465456076952267,13.598800026894));
#45140=CARTESIAN_POINT('Ctrl Pts',(15.2796982401641,3.27093342747344,11.5713069420647));
#45141=CARTESIAN_POINT('Ctrl Pts',(15.1214439305953,3.10022368274011,8.11409859480372));
#45142=CARTESIAN_POINT('Ctrl Pts',(14.9631896210265,0.108653800813268,6.37285162355982));
#45143=CARTESIAN_POINT('Ctrl Pts',(14.8255161265539,-2.57987130069616,7.7291541803051));
#45144=CARTESIAN_POINT('Ctrl Pts',(14.7405940686042,-3.06636667714361,9.37856363020343));
#45145=CARTESIAN_POINT('Ctrl Pts',(14.7084234471774,-3.0695085210094,10.001693524509));
#45146=CARTESIAN_POINT('Ctrl Pts',(15.7915765528225,-3.06925303971756,10.0014017874572));
#45147=CARTESIAN_POINT('Ctrl Pts',(15.7700184793637,-3.0709947854797,10.419061215057));
#45148=CARTESIAN_POINT('Ctrl Pts',(15.6958596929498,-2.79771444910674,11.8536079306759));
#45149=CARTESIAN_POINT('Ctrl Pts',(15.569100193581,-0.623826992014808,13.5712353851694));
#45150=CARTESIAN_POINT('Ctrl Pts',(15.4112980547159,2.6470767906288,12.4770681776581));
#45151=CARTESIAN_POINT('Ctrl Pts',(15.2534959158509,3.52203268603658,9.14083293199628));
#45152=CARTESIAN_POINT('Ctrl Pts',(15.0956937769859,1.20909210531671,6.58225533822185));
#45153=CARTESIAN_POINT('Ctrl Pts',(14.9417206559765,-2.11555602202281,7.10420025525831));
#45154=CARTESIAN_POINT('Ctrl Pts',(14.840348247922,-3.07277211406065,9.06306319147173));
#45155=CARTESIAN_POINT('Ctrl Pts',(14.7915765528225,-3.07773737838628,10.0012785594934));
#45156=CARTESIAN_POINT('Origin',(28.2084234471774,0.,10.));
#45157=CARTESIAN_POINT('',(16.7915765528225,-3.07290364494114,9.99728541773805));
#45158=CARTESIAN_POINT('',(16.7084234471774,-3.07836763528546,10.0005201776737));
#45159=CARTESIAN_POINT('',(28.2084234471774,-3.0735,10.0000000000003));
#45160=CARTESIAN_POINT('Ctrl Pts',(16.7084234471774,-3.07836763528546,10.0005201776737));
#45161=CARTESIAN_POINT('Ctrl Pts',(16.7069446402127,-3.07843463866697,10.0289523017141));
#45162=CARTESIAN_POINT('Ctrl Pts',(16.652714396725,-3.06523049811435,11.0715405015603));
#45163=CARTESIAN_POINT('Ctrl Pts',(16.5457327167144,-1.89232070283748,13.0963096341866));
#45164=CARTESIAN_POINT('Ctrl Pts',(16.3874784071456,1.56452653085165,13.2741819936291));
#45165=CARTESIAN_POINT('Ctrl Pts',(16.2292240975768,3.59782792524174,10.4729114224616));
#45166=CARTESIAN_POINT('Ctrl Pts',(16.070969788008,2.35750444175658,7.24134384160661));
#45167=CARTESIAN_POINT('Ctrl Pts',(15.9127154784392,-1.02788694119381,6.51984778648015));
#45168=CARTESIAN_POINT('Ctrl Pts',(15.7918666981624,-2.89889441257722,8.38698272986147));
#45169=CARTESIAN_POINT('Ctrl Pts',(15.7237693544085,-3.07424994705583,9.70068158821311));
#45170=CARTESIAN_POINT('Ctrl Pts',(15.7084234471775,-3.07179824204593,9.99736628792378));
#45171=CARTESIAN_POINT('Ctrl Pts',(16.7915765528225,-3.07290364494114,9.99728541773805));
#45172=CARTESIAN_POINT('Ctrl Pts',(16.7522894237604,-3.0662073138402,10.7561373882069));
#45173=CARTESIAN_POINT('Ctrl Pts',(16.6604015817432,-2.4009813074848,12.541494677525));
#45174=CARTESIAN_POINT('Ctrl Pts',(16.515913026771,0.582046717903019,13.5782822569538));
#45175=CARTESIAN_POINT('Ctrl Pts',(16.358110887906,3.3131115922785,11.4717927399475));
#45176=CARTESIAN_POINT('Ctrl Pts',(16.200308749041,3.04538068264102,8.03313986515331));
#45177=CARTESIAN_POINT('Ctrl Pts',(16.042506610176,0.0211851935724078,6.37475056308874));
#45178=CARTESIAN_POINT('Ctrl Pts',(15.9062625447698,-2.60641680486434,7.77596614521566));
#45179=CARTESIAN_POINT('Ctrl Pts',(15.8226191923187,-3.06674500550516,9.39999131968569));
#45180=CARTESIAN_POINT('Ctrl Pts',(15.7915765528225,-3.06925303971756,10.0014017874572));
#45181=CARTESIAN_POINT('Origin',(28.2084234471774,0.,10.));
#45182=CARTESIAN_POINT('',(17.7915765528225,-3.07753293276637,10.0014524138578));
#45183=CARTESIAN_POINT('',(17.7084234471775,-3.07037063174865,10.0022000552251));
#45184=CARTESIAN_POINT('',(28.2084234471774,-3.0735,10.0000000000003));
#45185=CARTESIAN_POINT('Ctrl Pts',(17.7084234471775,-3.07037063174865,10.0022000552251));
#45186=CARTESIAN_POINT('Ctrl Pts',(17.6901199260169,-3.07273452913448,10.3564806138557));
#45187=CARTESIAN_POINT('Ctrl Pts',(17.6190649683335,-2.85277747528598,11.7289669017069));
#45188=CARTESIAN_POINT('Ctrl Pts',(17.4952585741271,-0.832373015781326,
13.5320201239153));
#45189=CARTESIAN_POINT('Ctrl Pts',(17.3370042645583,2.50755641786257,12.6230081594193));
#45190=CARTESIAN_POINT('Ctrl Pts',(17.1787499549895,3.56588727515458,9.32734932243063));
#45191=CARTESIAN_POINT('Ctrl Pts',(17.0204956454207,1.37965570806092,6.64372809201059));
#45192=CARTESIAN_POINT('Ctrl Pts',(16.8637201428167,-2.02975002902867,7.01048305338277));
#45193=CARTESIAN_POINT('Ctrl Pts',(16.7596960767356,-3.07604451966515,9.0147324459357));
#45194=CARTESIAN_POINT('Ctrl Pts',(16.7084234471774,-3.07836763528546,10.0005201776737));
#45195=CARTESIAN_POINT('Ctrl Pts',(17.7915765528225,-3.07753293276637,10.0014524138578));
#45196=CARTESIAN_POINT('Ctrl Pts',(17.787161081112,-3.07803302068731,10.0864072843152));
#45197=CARTESIAN_POINT('Ctrl Pts',(17.7301448964466,-3.03649421916237,11.1829179356957));
#45198=CARTESIAN_POINT('Ctrl Pts',(17.6205279988261,-1.72553916596101,13.1883219534713));
#45199=CARTESIAN_POINT('Ctrl Pts',(17.462725859961,1.72352045101636,13.1894136682438));
#45200=CARTESIAN_POINT('Ctrl Pts',(17.3049237210961,3.61257047634171,10.3036722669531));
#45201=CARTESIAN_POINT('Ctrl Pts',(17.147121582231,2.23177558030935,7.14306807022165));
#45202=CARTESIAN_POINT('Ctrl Pts',(16.989319443366,-1.1690657327204,6.56835788508897));
#45203=CARTESIAN_POINT('Ctrl Pts',(16.8708044335632,-2.92850548206875,8.46950746821872));
#45204=CARTESIAN_POINT('Ctrl Pts',(16.8048901367154,-3.07517289107886,9.74012640377492));
#45205=CARTESIAN_POINT('Ctrl Pts',(16.7915765528225,-3.07290364494114,9.99728541773805));
#45206=CARTESIAN_POINT('Origin',(28.2084234471774,0.,10.));
#45207=CARTESIAN_POINT('',(18.7915765528225,-3.06910451058797,10.0012422495348));
#45208=CARTESIAN_POINT('',(18.7084234471775,-3.07067170632208,9.99767573393063));
#45209=CARTESIAN_POINT('',(28.2084234471774,-3.0735,10.0000000000003));
#45210=CARTESIAN_POINT('Ctrl Pts',(18.7084234471775,-3.07067170632208,9.99767573393063));
#45211=CARTESIAN_POINT('Ctrl Pts',(18.6732952118212,-3.06584729530095,10.6774452904515));
#45212=CARTESIAN_POINT('Ctrl Pts',(18.585415539942,-2.50862065342642,12.3851967347818));
#45213=CARTESIAN_POINT('Ctrl Pts',(18.4447844315398,0.31059273116958,13.6154589125709));
#45214=CARTESIAN_POINT('Ctrl Pts',(18.286530121971,3.2004911372734,11.7102243926977));
#45215=CARTESIAN_POINT('Ctrl Pts',(18.1282758124023,3.17829712925949,8.24887511830688));
#45216=CARTESIAN_POINT('Ctrl Pts',(17.9700215028334,0.264204795973602,6.38085551284168));
#45217=CARTESIAN_POINT('Ctrl Pts',(17.8300707144252,-2.52543982199027,7.64104243304114));
#45218=CARTESIAN_POINT('Ctrl Pts',(17.7428713625399,-3.06592168794387,9.33543071662528));
#45219=CARTESIAN_POINT('Ctrl Pts',(17.7084234471775,-3.07037063174865,10.0022000552251));
#45220=CARTESIAN_POINT('Ctrl Pts',(18.7915765528225,-3.06910451058797,10.0012422495348));
#45221=CARTESIAN_POINT('Ctrl Pts',(18.7694320255087,-3.07068542358524,10.4303154839391));
#45222=CARTESIAN_POINT('Ctrl Pts',(18.6946867852399,-2.78719815131979,11.8765861322557));
#45223=CARTESIAN_POINT('Ctrl Pts',(18.5673408320161,-0.584311835073177,
13.5779130749147));
#45224=CARTESIAN_POINT('Ctrl Pts',(18.4095386931511,2.6742969880911,12.4476555950008));
#45225=CARTESIAN_POINT('Ctrl Pts',(18.2517365542861,3.51232011417934,9.10195227978501));
#45226=CARTESIAN_POINT('Ctrl Pts',(18.0939344154211,1.17123790163294,6.56909865049566));
#45227=CARTESIAN_POINT('Ctrl Pts',(17.9405477482666,-2.13479723191698,7.12563505721765));
#45228=CARTESIAN_POINT('Ctrl Pts',(17.8397617940671,-3.07207556406519,9.07435533425115));
#45229=CARTESIAN_POINT('Ctrl Pts',(17.7915765528225,-3.07753293276637,10.0014524138578));
#45230=CARTESIAN_POINT('Origin',(28.2084234471774,0.,10.));
#45231=CARTESIAN_POINT('',(19.7915765528226,-3.07323555454232,9.99727800514525));
#45232=CARTESIAN_POINT('',(19.7084234471775,-3.07844518169678,9.99971767584083));
#45233=CARTESIAN_POINT('',(28.2084234471774,-3.0735,10.0000000000003));
#45234=CARTESIAN_POINT('Ctrl Pts',(19.7084234471775,-3.07844518169678,9.99971767584083));
#45235=CARTESIAN_POINT('Ctrl Pts',(19.6564704976254,-3.07712673515848,10.9985178159267));
#45236=CARTESIAN_POINT('Ctrl Pts',(19.5517661115504,-2.00606157994286,13.0138977284695));
#45237=CARTESIAN_POINT('Ctrl Pts',(19.3943102889525,1.42258101312554,13.3383040985265));
#45238=CARTESIAN_POINT('Ctrl Pts',(19.2360559793837,3.57421973167857,10.6268686487801));
#45239=CARTESIAN_POINT('Ctrl Pts',(19.0778016698149,2.47371441340158,7.34505216735374));
#45240=CARTESIAN_POINT('Ctrl Pts',(18.9195473602461,-0.877597005871997,
6.47894412307493));
#45241=CARTESIAN_POINT('Ctrl Pts',(18.7964212860336,-2.86373988760194,8.297708117217));
#45242=CARTESIAN_POINT('Ctrl Pts',(18.7260466483441,-3.07309202618938,9.65664762591398));
#45243=CARTESIAN_POINT('Ctrl Pts',(18.7084234471775,-3.07067170632208,9.99767573393063));
#45244=CARTESIAN_POINT('Ctrl Pts',(19.7915765528226,-3.07323555454232,9.99727800514525));
#45245=CARTESIAN_POINT('Ctrl Pts',(19.7517029699054,-3.06635454716845,10.7672451060908));
#45246=CARTESIAN_POINT('Ctrl Pts',(19.6592286740333,-2.38489386469174,12.5638062052433));
#45247=CARTESIAN_POINT('Ctrl Pts',(19.5141536652062,0.621566094242422,13.5716295836412));
#45248=CARTESIAN_POINT('Ctrl Pts',(19.3563515263411,3.32917861036942,11.4350791171607));
#45249=CARTESIAN_POINT('Ctrl Pts',(19.1985493874761,3.02345260681924,7.99959588418488));
#45250=CARTESIAN_POINT('Ctrl Pts',(19.0407472486111,-0.0188902229263912,
6.37473787820383));
#45251=CARTESIAN_POINT('Ctrl Pts',(18.9050896370599,-2.61959942140483,7.79875770460526));
#45252=CARTESIAN_POINT('Ctrl Pts',(18.8220327384637,-3.06693022260047,9.4111219956457));
#45253=CARTESIAN_POINT('Ctrl Pts',(18.7915765528225,-3.06910451058797,10.0012422495348));
#45254=CARTESIAN_POINT('Origin',(28.2084234471774,0.,10.));
#45255=CARTESIAN_POINT('',(20.7915765528225,-3.07730739150996,10.0016176250368));
#45256=CARTESIAN_POINT('',(20.7084234471775,-3.0714446790292,10.0025593696137));
#45257=CARTESIAN_POINT('',(28.2084234471774,-3.0735,10.0000000000003));
#45258=CARTESIAN_POINT('Ctrl Pts',(20.7084234471775,-3.0714446790292,10.0025593696137));
#45259=CARTESIAN_POINT('Ctrl Pts',(20.6923972199526,-3.07391157156986,10.3124871628441));
#45260=CARTESIAN_POINT('Ctrl Pts',(20.6236195562048,-2.88863851193006,11.6396831302958));
#45261=CARTESIAN_POINT('Ctrl Pts',(20.502090455934,-0.983175116979502,13.4930470484227));
#45262=CARTESIAN_POINT('Ctrl Pts',(20.3438361463652,2.39268589243202,12.7281981623963));
#45263=CARTESIAN_POINT('Ctrl Pts',(20.1855818367964,3.59146777933862,9.48099115314302));
#45264=CARTESIAN_POINT('Ctrl Pts',(20.0273275272277,1.52241181662405,6.70602470353113));
#45265=CARTESIAN_POINT('Ctrl Pts',(19.8690732176588,-1.93187026052108,6.9282108975943));
#45266=CARTESIAN_POINT('Ctrl Pts',(19.7627718576421,-3.07142617074966,8.95488367414853));
#45267=CARTESIAN_POINT('Ctrl Pts',(19.7092219341483,-3.0784654454622,9.9843666918209));
#45268=CARTESIAN_POINT('Ctrl Pts',(19.7084234471775,-3.07844518169678,9.99971767584083));
#45269=CARTESIAN_POINT('Ctrl Pts',(20.7915765528225,-3.07730739150996,10.0016176250368));
#45270=CARTESIAN_POINT('Ctrl Pts',(20.7865746272571,-3.07792592522714,10.0978746732603));
#45271=CARTESIAN_POINT('Ctrl Pts',(20.7289719887367,-3.03036433852053,11.2057607933903));
#45272=CARTESIAN_POINT('Ctrl Pts',(20.6187686372612,-1.69018948530375,13.2072015521334));
#45273=CARTESIAN_POINT('Ctrl Pts',(20.4609664983962,1.75867146489572,13.1701667102578));
#45274=CARTESIAN_POINT('Ctrl Pts',(20.3031643595312,3.61570659591804,10.2637197460999));
#45275=CARTESIAN_POINT('Ctrl Pts',(20.1453622206662,2.20005821053506,7.11857220071228));
#45276=CARTESIAN_POINT('Ctrl Pts',(19.9875600818011,-1.20692825766852,6.58149060655154));
#45277=CARTESIAN_POINT('Ctrl Pts',(19.8696315258533,-2.93664307613956,8.49246995470104));
#45278=CARTESIAN_POINT('Ctrl Pts',(19.8043036828604,-3.07543188276848,9.75151450205139));
#45279=CARTESIAN_POINT('Ctrl Pts',(19.7915765528226,-3.07323555454232,9.99727800514525));
#45280=CARTESIAN_POINT('Origin',(28.2084234471774,0.,10.));
#45281=CARTESIAN_POINT('',(21.7915765528225,-3.06897452734334,10.0010772957271));
#45282=CARTESIAN_POINT('',(21.7084234471775,-3.06974091379035,9.99814174205166));
#45283=CARTESIAN_POINT('',(28.2084234471774,-3.0735,10.0000000000003));
#45284=CARTESIAN_POINT('Ctrl Pts',(21.7084234471775,-3.06974091379035,9.99814174205167));
#45285=CARTESIAN_POINT('Ctrl Pts',(21.6755725057568,-3.0662040854976,10.6343282548533));
#45286=CARTESIAN_POINT('Ctrl Pts',(21.5899701278132,-2.56390958624238,12.2972104532282));
#45287=CARTESIAN_POINT('Ctrl Pts',(21.4516163133467,0.155157162744094,13.6254568329877));
#45288=CARTESIAN_POINT('Ctrl Pts',(21.2933620037779,3.1241524005353,11.845990999834));
#45289=CARTESIAN_POINT('Ctrl Pts',(21.1351076942091,3.2505150185073,8.38687783860446));
#45290=CARTESIAN_POINT('Ctrl Pts',(20.9768533846404,0.419269031639233,6.39552715751162));
#45291=CARTESIAN_POINT('Ctrl Pts',(20.8346253022964,-2.46811551266869,7.55338081248407));
#45292=CARTESIAN_POINT('Ctrl Pts',(20.7451486564755,-3.06579162397138,9.29233837287249));
#45293=CARTESIAN_POINT('Ctrl Pts',(20.7084234471775,-3.0714446790292,10.0025593696137));
#45294=CARTESIAN_POINT('Ctrl Pts',(21.7915765528226,-3.06897452734334,10.0010772957271));
#45295=CARTESIAN_POINT('Ctrl Pts',(21.7688455716538,-3.07037829602215,10.4415604023203));
#45296=CARTESIAN_POINT('Ctrl Pts',(21.69351387753,-2.77651448008785,11.8995593015108));
#45297=CARTESIAN_POINT('Ctrl Pts',(21.5655814704513,-0.544725276252224,
13.5841535492561));
#45298=CARTESIAN_POINT('Ctrl Pts',(21.4077793315862,2.70119039079158,12.4179439128307));
#45299=CARTESIAN_POINT('Ctrl Pts',(21.2499771927212,3.50217834240436,9.06318136752485));
#45300=CARTESIAN_POINT('Ctrl Pts',(21.0921750538562,1.13324057456603,6.55636121344182));
#45301=CARTESIAN_POINT('Ctrl Pts',(20.9393748405567,-2.15382461611422,7.14714164828928));
#45302=CARTESIAN_POINT('Ctrl Pts',(20.8391753402121,-3.07142136731547,9.0856266305313));
#45303=CARTESIAN_POINT('Ctrl Pts',(20.7915765528225,-3.07730739150996,10.0016176250368));
#45304=CARTESIAN_POINT('Origin',(28.2084234471774,0.,10.));
#45305=CARTESIAN_POINT('',(22.7915765528226,-3.07357058804542,9.99728370345179));
#45306=CARTESIAN_POINT('',(22.7084234471774,-3.07802566627685,9.99894307990421));
#45307=CARTESIAN_POINT('',(28.2084234471774,-3.0735,10.0000000000003));
#45308=CARTESIAN_POINT('Ctrl Pts',(22.7084234471774,-3.07802566627685,9.99894307990421));
#45309=CARTESIAN_POINT('Ctrl Pts',(22.658747791561,-3.07374767361358,10.9543104693303));
#45310=CARTESIAN_POINT('Ctrl Pts',(22.5563206994218,-2.08420676059476,12.9318512556298));
#45311=CARTESIAN_POINT('Ctrl Pts',(22.4011421707594,1.27801459267746,13.39627585532));
#45312=CARTESIAN_POINT('Ctrl Pts',(22.2428878611907,3.5440265506493,10.7796709598669));
#45313=CARTESIAN_POINT('Ctrl Pts',(22.0846335516218,2.58536692026875,7.45365185399615));
#45314=CARTESIAN_POINT('Ctrl Pts',(21.9263792420531,-0.725690223623306,
6.44452750096693));
#45315=CARTESIAN_POINT('Ctrl Pts',(21.8009758739049,-2.82619643473853,8.2084169339104));
#45316=CARTESIAN_POINT('Ctrl Pts',(21.7283239422797,-3.07188345921138,9.61275167301163));
#45317=CARTESIAN_POINT('Ctrl Pts',(21.7084234471775,-3.06974091379035,9.99814174205167));
#45318=CARTESIAN_POINT('Ctrl Pts',(22.7915765528226,-3.07357058804542,9.99728370345179));
#45319=CARTESIAN_POINT('Ctrl Pts',(22.7511165160505,-3.06653153385114,10.7783573196862));
#45320=CARTESIAN_POINT('Ctrl Pts',(22.6580557663234,-2.36860505410454,12.5860731442903));
#45321=CARTESIAN_POINT('Ctrl Pts',(22.5123943036413,0.661009511544134,13.5645404549472));
#45322=CARTESIAN_POINT('Ctrl Pts',(22.3545921647763,3.34483881058325,11.3981901341401));
#45323=CARTESIAN_POINT('Ctrl Pts',(22.1967900259113,3.0011550686756,7.96629634724844));
#45324=CARTESIAN_POINT('Ctrl Pts',(22.0389878870462,-0.0589633304184637,
6.37516819565949));
#45325=CARTESIAN_POINT('Ctrl Pts',(21.90391672935,-2.63259802844919,7.82156968830812));
#45326=CARTESIAN_POINT('Ctrl Pts',(21.8214462846088,-3.06712989980111,9.42225880335216));
#45327=CARTESIAN_POINT('Ctrl Pts',(21.7915765528226,-3.06897452734334,10.0010772957271));
#45328=CARTESIAN_POINT('Origin',(28.2084234471774,0.,10.));
#45329=CARTESIAN_POINT('',(23.7915765528225,-3.07706282942884,10.001773157772));
#45330=CARTESIAN_POINT('',(23.7084234471775,-3.07267174134012,10.002743176848));
#45331=CARTESIAN_POINT('',(28.2084234471774,-3.0735,10.0000000000003));
#45332=CARTESIAN_POINT('Ctrl Pts',(23.7084234471775,-3.07267174134012,10.002743176848));
#45333=CARTESIAN_POINT('Ctrl Pts',(23.6946745138882,-3.07501208864137,10.2683613076082));
#45334=CARTESIAN_POINT('Ctrl Pts',(23.628174144076,-2.92215844456484,11.5504428457205));
#45335=CARTESIAN_POINT('Ctrl Pts',(23.5089223377409,-1.13216576586705,13.447638623633));
#45336=CARTESIAN_POINT('Ctrl Pts',(23.3506680281721,2.27340713764739,12.8283618044535));
#45337=CARTESIAN_POINT('Ctrl Pts',(23.1924137186033,3.61043154357666,9.63558920748943));
#45338=CARTESIAN_POINT('Ctrl Pts',(23.0341594090345,1.66236308643603,6.77438998022499));
#45339=CARTESIAN_POINT('Ctrl Pts',(22.8759050994658,-1.79827159213679,6.848138612079));
#45340=CARTESIAN_POINT('Ctrl Pts',(22.7673264455134,-3.05000135332916,8.86637271869838));
#45341=CARTESIAN_POINT('Ctrl Pts',(22.7114992280839,-3.07829054789721,9.93978934074102));
#45342=CARTESIAN_POINT('Ctrl Pts',(22.7084234471774,-3.07802566627685,9.99894307990421));
#45343=CARTESIAN_POINT('Ctrl Pts',(23.7915765528225,-3.07706282942884,10.001773157772));
#45344=CARTESIAN_POINT('Ctrl Pts',(23.7859881734021,-3.07780627720245,10.1093384104667));
#45345=CARTESIAN_POINT('Ctrl Pts',(23.7277990810267,-3.02410010614128,11.2286131560421));
#45346=CARTESIAN_POINT('Ctrl Pts',(23.6170092756964,-1.65463280838614,13.2256900191163));
#45347=CARTESIAN_POINT('Ctrl Pts',(23.4592071368313,1.79360733424122,13.1505319563297));
#45348=CARTESIAN_POINT('Ctrl Pts',(23.3014049979663,3.61840100535183,10.2237352102483));
#45349=CARTESIAN_POINT('Ctrl Pts',(23.1436028591013,2.16807193309428,7.09442832744505));
#45350=CARTESIAN_POINT('Ctrl Pts',(22.9858007202363,-1.24464326464773,6.59504112130271));
#45351=CARTESIAN_POINT('Ctrl Pts',(22.8684586181434,-2.94463192189129,8.5154264800344));
#45352=CARTESIAN_POINT('Ctrl Pts',(22.8037172290055,-3.07568276797467,9.76291016832276));
#45353=CARTESIAN_POINT('Ctrl Pts',(22.7915765528226,-3.07357058804542,9.99728370345179));
#45354=CARTESIAN_POINT('Origin',(28.2084234471774,0.,10.));
#45355=CARTESIAN_POINT('',(24.7915765528225,-3.06884999403827,10.0009308069803));
#45356=CARTESIAN_POINT('',(24.7084234471775,-3.06905088107409,9.99873461494295));
#45357=CARTESIAN_POINT('',(28.2084234471774,-3.0735,10.0000000000003));
#45358=CARTESIAN_POINT('Ctrl Pts',(24.7084234471775,-3.06905088107409,9.99873461494295));
#45359=CARTESIAN_POINT('Ctrl Pts',(24.6778497996924,-3.06683417076947,10.5911491717355));
#45360=CARTESIAN_POINT('Ctrl Pts',(24.5945247156845,-2.6163584606915,12.2088261427766));
#45361=CARTESIAN_POINT('Ctrl Pts',(24.4584481951536,-0.000559519202797285,
13.6287799388967));
#45362=CARTESIAN_POINT('Ctrl Pts',(24.3001938855848,3.04205539834121,11.9783542595615));
#45363=CARTESIAN_POINT('Ctrl Pts',(24.141939576016,3.31674557789901,8.52785373790922));
#45364=CARTESIAN_POINT('Ctrl Pts',(23.9836852664473,0.573560160241939,6.41683888716847));
#45365=CARTESIAN_POINT('Ctrl Pts',(23.8391798901677,-2.40783492161846,7.46625913576792));
#45366=CARTESIAN_POINT('Ctrl Pts',(23.7474259504111,-3.06603272424225,9.24924675745743));
#45367=CARTESIAN_POINT('Ctrl Pts',(23.7084234471775,-3.07267174134012,10.002743176848));
#45368=CARTESIAN_POINT('Ctrl Pts',(24.7915765528225,-3.06884999403827,10.0009308069803));
#45369=CARTESIAN_POINT('Ctrl Pts',(24.7682591177988,-3.07006994083386,10.4528032974328));
#45370=CARTESIAN_POINT('Ctrl Pts',(24.6923409698201,-2.76569457382785,11.9224712354734));
#45371=CARTESIAN_POINT('Ctrl Pts',(24.5638221088864,-0.505048782495192,
13.5899960272459));
#45372=CARTESIAN_POINT('Ctrl Pts',(24.4060199700213,2.72774157840345,12.387916003312));
#45373=CARTESIAN_POINT('Ctrl Pts',(24.2482178311564,3.49161491002287,9.0245357108578));
#45374=CARTESIAN_POINT('Ctrl Pts',(24.0904156922914,1.09510149634942,6.54403898763965));
#45375=CARTESIAN_POINT('Ctrl Pts',(23.9382019328468,-2.17263741343222,7.16872054184951));
#45376=CARTESIAN_POINT('Ctrl Pts',(23.8385888863571,-3.07080856283935,9.09687870519458));
#45377=CARTESIAN_POINT('Ctrl Pts',(23.7915765528225,-3.07706282942884,10.001773157772));
#45378=CARTESIAN_POINT('Origin',(28.2084234471774,0.,10.));
#45379=CARTESIAN_POINT('',(25.7915765528225,-3.07002684332744,10.000064028751));
#45380=CARTESIAN_POINT('',(25.7084234471775,-3.07694191359583,9.99853189658296));
#45381=CARTESIAN_POINT('',(28.2084234471774,-3.0735,10.0000000000003));
#45382=CARTESIAN_POINT('',(25.8262392198064,-3.00089449353541,9.33589572455161));
#45383=CARTESIAN_POINT('Ctrl Pts',(25.8262392198064,-3.0008944935354,9.33589572455155));
#45384=CARTESIAN_POINT('Ctrl Pts',(25.8146849974785,-3.04910668411157,9.55375262228589));
#45385=CARTESIAN_POINT('Ctrl Pts',(25.8031307751505,-3.07166211508236,9.77686471172983));
#45386=CARTESIAN_POINT('Ctrl Pts',(25.7915765528226,-3.07002654794609,10.0000640341964));
#45387=CARTESIAN_POINT('',(26.,1.26217744835362E-28,6.9265));
#45388=CARTESIAN_POINT('Ctrl Pts',(26.,-2.4980018054066E-15,6.9265));
#45389=CARTESIAN_POINT('Ctrl Pts',(26.,-0.386302212465491,6.9265));
#45390=CARTESIAN_POINT('Ctrl Pts',(25.9905104526593,-0.79810794837382,7.00377648233523));
#45391=CARTESIAN_POINT('Ctrl Pts',(25.9562094606332,-1.55524928118873,7.31755124766488));
#45392=CARTESIAN_POINT('Ctrl Pts',(25.9318826712469,-1.9006150067912,7.55402962283749));
#45393=CARTESIAN_POINT('Ctrl Pts',(25.8861371643816,-2.44597219633851,8.0993868123848));
#45394=CARTESIAN_POINT('Ctrl Pts',(25.8617357704543,-2.68244914732635,8.4447517454274));
#45395=CARTESIAN_POINT('Ctrl Pts',(25.8369342606554,-2.90820005126638,8.98949060270564));
#45396=CARTESIAN_POINT('Ctrl Pts',(25.8307130606305,-2.96239181255062,9.16191328290026));
#45397=CARTESIAN_POINT('Ctrl Pts',(25.8262392198064,-3.00089449353541,9.33589572455161));
#45398=CARTESIAN_POINT('',(25.9920223077014,0.645410697669269,6.99640220569977));
#45399=CARTESIAN_POINT('Ctrl Pts',(25.9920223077014,0.644031331499173,6.99473364008323));
#45400=CARTESIAN_POINT('Ctrl Pts',(25.9973703299551,0.428194140166751,6.94847953243578));
#45401=CARTESIAN_POINT('Ctrl Pts',(26.,0.210221720574735,6.9265));
#45402=CARTESIAN_POINT('Ctrl Pts',(26.,-2.42861286636753E-15,6.9265));
#45403=CARTESIAN_POINT('Ctrl Pts',(25.9920223077014,0.647043985098389,6.99837792998922));
#45404=CARTESIAN_POINT('Ctrl Pts',(25.9555938655585,-0.0431691754597013,
6.85594805878722));
#45405=CARTESIAN_POINT('Ctrl Pts',(25.8664139868927,-1.86387412312115,7.06750307061891));
#45406=CARTESIAN_POINT('Ctrl Pts',(25.7718810333847,-3.02648815522162,8.77779906703974));
#45407=CARTESIAN_POINT('Ctrl Pts',(25.7137765220196,-3.07764892068114,9.89550066802324));
#45408=CARTESIAN_POINT('Ctrl Pts',(25.7084234471775,-3.07694191359583,9.99853189658296));
#45409=CARTESIAN_POINT('Origin',(0.,0.,181.5));
#45410=CARTESIAN_POINT('',(-19.,-2.32682891837997E-15,181.));
#45411=CARTESIAN_POINT('Origin',(0.,0.,181.));
#45412=CARTESIAN_POINT('',(-19.,-2.32682891837997E-15,182.));
#45413=CARTESIAN_POINT('',(-19.,-2.32682891837997E-15,181.5));
#45414=CARTESIAN_POINT('Origin',(0.,0.,182.));
#45415=CARTESIAN_POINT('Origin',(23.,0.,181.));
#45416=CARTESIAN_POINT('',(-20.,2.44929359829471E-15,181.));
#45417=CARTESIAN_POINT('Origin',(0.,0.,181.));
#45418=CARTESIAN_POINT('Origin',(19.,0.,182.));
#45419=CARTESIAN_POINT('',(-20.,-2.44929359829471E-15,182.));
#45420=CARTESIAN_POINT('Origin',(0.,0.,182.));
#45421=CARTESIAN_POINT('Origin',(0.,0.,20.));
#45422=CARTESIAN_POINT('',(-20.,-2.44929359829471E-15,225.));
#45423=CARTESIAN_POINT('Origin',(0.,0.,225.));
#45424=CARTESIAN_POINT('',(-20.,-2.44929359829471E-15,20.));
#45425=CARTESIAN_POINT('Origin',(12.,-4.,240.));
#45426=CARTESIAN_POINT('',(11.3137084989848,-4.,225.));
#45427=CARTESIAN_POINT('',(11.3137084989848,-4.,255.));
#45428=CARTESIAN_POINT('',(11.3137084989848,-4.,220.));
#45429=CARTESIAN_POINT('',(8.,-4.,225.));
#45430=CARTESIAN_POINT('',(8.,-4.,225.));
#45431=CARTESIAN_POINT('',(8.,-4.,255.));
#45432=CARTESIAN_POINT('',(8.,-4.,255.));
#45433=CARTESIAN_POINT('',(16.,-4.,255.));
#45434=CARTESIAN_POINT('Origin',(8.,0.,225.));
#45435=CARTESIAN_POINT('',(8.,4.,255.));
#45436=CARTESIAN_POINT('',(8.,0.,255.));
#45437=CARTESIAN_POINT('',(8.,4.,225.));
#45438=CARTESIAN_POINT('',(8.,0.,225.));
#45439=CARTESIAN_POINT('',(8.,4.,255.));
#45440=CARTESIAN_POINT('Origin',(8.,0.,255.));
#45441=CARTESIAN_POINT('',(11.3137084989848,4.,255.));
#45442=CARTESIAN_POINT('Origin',(0.,0.,255.));
#45443=CARTESIAN_POINT('',(16.,4.,255.));
#45444=CARTESIAN_POINT('Origin',(12.,4.,240.));
#45445=CARTESIAN_POINT('',(11.3137084989848,4.,225.));
#45446=CARTESIAN_POINT('',(11.3137084989848,4.,220.));
#45447=CARTESIAN_POINT('',(8.,4.,225.));
#45448=CARTESIAN_POINT('Origin',(0.,0.,225.));
#45449=CARTESIAN_POINT('',(-12.,-1.46957615897682E-15,225.));
#45450=CARTESIAN_POINT('Origin',(0.,0.,225.));
#45451=CARTESIAN_POINT('Origin',(0.,0.,225.));
#45452=CARTESIAN_POINT('Ctrl Pts',(25.8782388507408,2.51331533716111,9.85490600980488));
#45453=CARTESIAN_POINT('Ctrl Pts',(25.8254874142179,2.46522436200857,9.02187505333748));
#45454=CARTESIAN_POINT('Ctrl Pts',(25.719984541172,1.47678881906405,7.42156871988577));
#45455=CARTESIAN_POINT('Ctrl Pts',(25.5617302316032,-1.36226416922746,7.35610196821514));
#45456=CARTESIAN_POINT('Ctrl Pts',(25.4034759220345,-2.95646907341594,9.70130182803619));
#45457=CARTESIAN_POINT('Ctrl Pts',(25.2452216124657,-1.86324714060836,12.3157605506598));
#45458=CARTESIAN_POINT('Ctrl Pts',(25.0869673028969,0.926675464118667,12.8244356151764));
#45459=CARTESIAN_POINT('Ctrl Pts',(24.9287129933281,2.87272546418627,10.7625119609902));
#45460=CARTESIAN_POINT('Ctrl Pts',(24.7704586837593,2.20527713880316,8.00713739835836));
#45461=CARTESIAN_POINT('Ctrl Pts',(24.6122043741905,-0.468917913780222,
7.06486504705933));
#45462=CARTESIAN_POINT('Ctrl Pts',(24.4539500646218,-2.71635156248176,8.79333488723566));
#45463=CARTESIAN_POINT('Ctrl Pts',(24.295695755053,-2.49225709450323,11.6196872386657));
#45464=CARTESIAN_POINT('Ctrl Pts',(24.1374414454842,-0.000458301478133477,
12.9723291023825));
#45465=CARTESIAN_POINT('Ctrl Pts',(23.9791871359154,2.49174376617016,11.6204674958341));
#45466=CARTESIAN_POINT('Ctrl Pts',(23.8209328263466,2.71674214815707,8.794166840796));
#45467=CARTESIAN_POINT('Ctrl Pts',(23.6626785167778,0.469802408787728,7.06503722090339));
#45468=CARTESIAN_POINT('Ctrl Pts',(23.504424207209,-2.20460355977341,8.00640047512599));
#45469=CARTESIAN_POINT('Ctrl Pts',(23.3461698976402,-2.87306549282161,10.7617175021526));
#45470=CARTESIAN_POINT('Ctrl Pts',(23.1879155880715,-0.927355560621537,
12.8239564779555));
#45471=CARTESIAN_POINT('Ctrl Pts',(23.0296612785027,1.86214493867816,12.3167076110986));
#45472=CARTESIAN_POINT('Ctrl Pts',(22.8714069689339,2.9572999547598,9.70151157633143));
#45473=CARTESIAN_POINT('Ctrl Pts',(22.7131526593651,1.36163952175133,7.35790687334192));
#45474=CARTESIAN_POINT('Ctrl Pts',(22.5548983497963,-1.47296200852591,7.4183142853128));
#45475=CARTESIAN_POINT('Ctrl Pts',(22.3966440402275,-2.9673312917242,9.8277697035192));
#45476=CARTESIAN_POINT('Ctrl Pts',(22.2383897306587,-1.76175778279907,12.3939356232425));
#45477=CARTESIAN_POINT('Ctrl Pts',(22.08013542109,1.04682015196535,12.7818852987695));
#45478=CARTESIAN_POINT('Ctrl Pts',(21.9218811115212,2.90290770823478,10.6386275065772));
#45479=CARTESIAN_POINT('Ctrl Pts',(21.7636268019524,2.1176708058489,7.91428942327487));
#45480=CARTESIAN_POINT('Ctrl Pts',(21.6053724923836,-0.594411953138661,
7.08771692978175));
#45481=CARTESIAN_POINT('Ctrl Pts',(21.4471181828149,-2.76564567861122,8.91099943403972));
#45482=CARTESIAN_POINT('Ctrl Pts',(21.288863873246,-2.4204481889921,11.7251518241051));
#45483=CARTESIAN_POINT('Ctrl Pts',(21.1306095636773,0.127089037647067,12.9696071504951));
#45484=CARTESIAN_POINT('Ctrl Pts',(20.9723552541085,2.55898931782906,11.5120489155952));
#45485=CARTESIAN_POINT('Ctrl Pts',(20.8141009445397,2.66249277992261,8.67869365826803));
#45486=CARTESIAN_POINT('Ctrl Pts',(20.655846634971,0.34342273862104,7.04758080983749));
#45487=CARTESIAN_POINT('Ctrl Pts',(20.4975923254021,-2.28812395363916,8.10284238276193));
#45488=CARTESIAN_POINT('Ctrl Pts',(20.3393380158334,-2.8377313052884,10.8843072378062));
#45489=CARTESIAN_POINT('Ctrl Pts',(20.1810837062645,-0.805317506749925,
12.8611504618201));
#45490=CARTESIAN_POINT('Ctrl Pts',(20.0228293966958,1.95984601730847,12.2346636973589));
#45491=CARTESIAN_POINT('Ctrl Pts',(19.864575087127,2.94176675922726,9.57488050367255));
#45492=CARTESIAN_POINT('Ctrl Pts',(19.7063207775582,1.24700561195739,7.30190896083931));
#45493=CARTESIAN_POINT('Ctrl Pts',(19.5480664679894,-1.58239251044796,7.48390139407635));
#45494=CARTESIAN_POINT('Ctrl Pts',(19.3898121584206,-2.9719887311495,9.95526484857637));
#45495=CARTESIAN_POINT('Ctrl Pts',(19.2315578488518,-1.65740441592337,12.4673323355256));
#45496=CARTESIAN_POINT('Ctrl Pts',(19.0733035392831,1.16523432586418,12.7344007053979));
#45497=CARTESIAN_POINT('Ctrl Pts',(18.9150492297143,2.92763890499457,10.5134673249728));
#45498=CARTESIAN_POINT('Ctrl Pts',(18.7567949201455,2.02621637733479,7.82533555598277));
#45499=CARTESIAN_POINT('Ctrl Pts',(18.5985406105767,-0.718838608193511,
7.11590754183866));
#45500=CARTESIAN_POINT('Ctrl Pts',(18.4402863010079,-2.80983008655689,9.0306841915391));
#45501=CARTESIAN_POINT('Ctrl Pts',(18.2820319914391,-2.34418743313729,11.8274308551006));
#45502=CARTESIAN_POINT('Ctrl Pts',(18.1237776818704,0.254406117039017,12.9614178664055));
#45503=CARTESIAN_POINT('Ctrl Pts',(17.9655233723016,2.62151828146601,11.4008426577571));
#45504=CARTESIAN_POINT('Ctrl Pts',(17.8072690627328,2.603339197303,8.56565580294047));
#45505=CARTESIAN_POINT('Ctrl Pts',(17.649014753164,0.21640981742754,7.03556328406668));
#45506=CARTESIAN_POINT('Ctrl Pts',(17.4907604435952,-2.36742852442935,8.20277980381625));
#45507=CARTESIAN_POINT('Ctrl Pts',(17.3325061340264,-2.79716915088687,11.0052676226654));
#45508=CARTESIAN_POINT('Ctrl Pts',(17.1742518244576,-0.681795694559783,
12.8930732591368));
#45509=CARTESIAN_POINT('Ctrl Pts',(17.0159975148889,2.05393632079682,12.148502697686));
#45510=CARTESIAN_POINT('Ctrl Pts',(16.8577432053201,2.92081380029337,9.44903267259446));
#45511=CARTESIAN_POINT('Ctrl Pts',(16.6994888957513,1.13007426225585,7.25088188437829));
#45512=CARTESIAN_POINT('Ctrl Pts',(16.5412345861825,-1.68890767526181,7.55412405950459));
#45513=CARTESIAN_POINT('Ctrl Pts',(16.3829802766137,-2.97117070985973,10.0828424089713));
#45514=CARTESIAN_POINT('Ctrl Pts',(16.2247259670449,-1.54999751729083,12.5361833427899));
#45515=CARTESIAN_POINT('Ctrl Pts',(16.0664716574761,1.28150172162649,12.6818783695986));
#45516=CARTESIAN_POINT('Ctrl Pts',(15.9082173479074,2.9469763467695,10.3873611537488));
#45517=CARTESIAN_POINT('Ctrl Pts',(15.7499630383386,1.93102893513004,7.74038819627284));
#45518=CARTESIAN_POINT('Ctrl Pts',(15.5917087287698,-0.841940905955885,
7.14941168129618));
#45519=CARTESIAN_POINT('Ctrl Pts',(15.433454419201,-2.8488377850469,9.15215477453626));
#45520=CARTESIAN_POINT('Ctrl Pts',(15.2752001096322,-2.26360784764101,11.9263431064976));
#45521=CARTESIAN_POINT('Ctrl Pts',(15.1169458000635,0.381254489581041,12.9477725940152));
#45522=CARTESIAN_POINT('Ctrl Pts',(14.9586914904947,2.67921747312979,11.2870555479577));
#45523=CARTESIAN_POINT('Ctrl Pts',(14.8004371809259,2.53938933505717,8.455260521366));
#45524=CARTESIAN_POINT('Ctrl Pts',(14.6421828713571,0.0889981921416642,
7.02900730838193));
#45525=CARTESIAN_POINT('Ctrl Pts',(14.4839285617883,-2.44237144722633,8.30602834568397));
#45526=CARTESIAN_POINT('Ctrl Pts',(14.3256742522195,-2.75145361293339,11.1243759459044));
#45527=CARTESIAN_POINT('Ctrl Pts',(14.1674199426507,-0.55701777144916,12.9196659833176));
#45528=CARTESIAN_POINT('Ctrl Pts',(14.009165633082,2.14424254077798,12.0583833895003));
#45529=CARTESIAN_POINT('Ctrl Pts',(13.8509113235132,2.89447966024978,9.32419991990774));
#45530=CARTESIAN_POINT('Ctrl Pts',(13.6926570139444,1.01106091257489,7.20491966431815));
#45531=CARTESIAN_POINT('Ctrl Pts',(13.5344027043756,-1.79231126956862,7.62885290105586));
#45532=CARTESIAN_POINT('Ctrl Pts',(13.3761483948068,-2.96487873206638,10.2102673440928));
#45533=CARTESIAN_POINT('Ctrl Pts',(13.217894085238,-1.43973497022295,12.6003617954753));
#45534=CARTESIAN_POINT('Ctrl Pts',(13.0596397756693,1.39540813400357,12.6244150570019));
#45535=CARTESIAN_POINT('Ctrl Pts',(12.9013854661004,2.96088440668839,10.2605413250743));
#45536=CARTESIAN_POINT('Ctrl Pts',(12.7431311565317,1.83228384867635,7.65960384769567));
#45537=CARTESIAN_POINT('Ctrl Pts',(12.5848768469629,-0.963492048187264,
7.18816762146178));
#45538=CARTESIAN_POINT('Ctrl Pts',(12.4266225373941,-2.88259690791579,9.27518739095129));
#45539=CARTESIAN_POINT('Ctrl Pts',(12.2683682278253,-2.17885788889992,12.0217063465763));
#45540=CARTESIAN_POINT('Ctrl Pts',(12.1101139182565,0.507400455370921,12.9286964728651));
#45541=CARTESIAN_POINT('Ctrl Pts',(11.9518596086877,2.73198059023493,11.170897222515));
#45542=CARTESIAN_POINT('Ctrl Pts',(11.793605299119,2.47076101180668,8.34771120128963));
#45543=CARTESIAN_POINT('Ctrl Pts',(11.6353509895502,-0.0385773998656385,
7.0279249607546));
#45544=CARTESIAN_POINT('Ctrl Pts',(11.4770966799814,-2.51281464985175,8.41239778862548));
#45545=CARTESIAN_POINT('Ctrl Pts',(11.3188423704126,-2.70066891686761,11.2414127657423));
#45546=CARTESIAN_POINT('Ctrl Pts',(11.1605880608438,-0.43121362073721,12.9408796444537));
#45547=CARTESIAN_POINT('Ctrl Pts',(11.0023337512751,2.2305982968671,11.9644717982181));
#45548=CARTESIAN_POINT('Ctrl Pts',(10.8440794417063,2.862812863889,9.20061224460173));
#45549=CARTESIAN_POINT('Ctrl Pts',(10.6858251321375,0.890184812731906,7.16410695535464));
#45550=CARTESIAN_POINT('Ctrl Pts',(10.5275708225687,-1.89241275771817,7.70795028797535));
#45551=CARTESIAN_POINT('Ctrl Pts',(10.3693165129999,-2.95312444633263,10.33730480233));
#45552=CARTESIAN_POINT('Ctrl Pts',(10.2110622034311,-1.32681980887658,12.659749626168));
#45553=CARTESIAN_POINT('Ctrl Pts',(10.0528078938623,1.50674349723582,12.5621163039333));
#45554=CARTESIAN_POINT('Ctrl Pts',(9.89455358429355,2.96933786459887,10.1332421248879));
#45555=CARTESIAN_POINT('Ctrl Pts',(9.73629927472478,1.73016226470662,7.58313011413639));
#45556=CARTESIAN_POINT('Ctrl Pts',(9.57804496515598,-1.08326659812887,7.23210632814751));
#45557=CARTESIAN_POINT('Ctrl Pts',(9.4197906555872,-2.9110481400647,9.39955081052956));
#45558=CARTESIAN_POINT('Ctrl Pts',(9.26153634601842,-2.09008814807197,12.1133536640817));
#45559=CARTESIAN_POINT('Ctrl Pts',(9.10328203644963,0.63260092362554,12.9042077365071));
#45560=CARTESIAN_POINT('Ctrl Pts',(8.94502772688085,2.77973100053036,11.0526142534321));
#45561=CARTESIAN_POINT('Ctrl Pts',(8.78677341731206,2.39754104106069,8.24314327152743));
#45562=CARTESIAN_POINT('Ctrl Pts',(8.62851910774328,-0.166005611993985,
7.03243901157466));
#45563=CARTESIAN_POINT('Ctrl Pts',(8.47026479817449,-2.57877530773441,8.52145954661513));
#45564=CARTESIAN_POINT('Ctrl Pts',(8.31201048860571,-2.64462552602106,11.3566107260726));
#45565=CARTESIAN_POINT('Ctrl Pts',(8.15375617903693,-0.305161145104408,
12.9558089680353));
#45566=CARTESIAN_POINT('Ctrl Pts',(7.99550186946814,2.31390515511262,11.868636776471));
#45567=CARTESIAN_POINT('Ctrl Pts',(7.83724755989935,2.82374457369778,9.07497045187927));
#45568=CARTESIAN_POINT('Ctrl Pts',(7.7317446868535,1.45630799602658,7.78342006978472));
#45569=CARTESIAN_POINT('Ctrl Pts',(7.67899325033057,0.650199997975098,7.56791319796493));
#45570=CARTESIAN_POINT('Ctrl Pts',(25.9852411006306,2.69834060395509,9.84422447937807));
#45571=CARTESIAN_POINT('Ctrl Pts',(25.9324896641077,2.64670926704356,8.94986744389102));
#45572=CARTESIAN_POINT('Ctrl Pts',(25.8269867910618,1.58550706910041,7.23174974712926));
#45573=CARTESIAN_POINT('Ctrl Pts',(25.668732481493,-1.46255134275814,7.1614634636574));
#45574=CARTESIAN_POINT('Ctrl Pts',(25.5104781719243,-3.17411843519274,9.67931226383733));
#45575=CARTESIAN_POINT('Ctrl Pts',(25.3522238623555,-2.0004156821745,12.4862422277425));
#45576=CARTESIAN_POINT('Ctrl Pts',(25.1939695527867,0.994895465184538,13.032364936863));
#45577=CARTESIAN_POINT('Ctrl Pts',(25.0357152432179,3.08420978832894,10.8186465720873));
#45578=CARTESIAN_POINT('Ctrl Pts',(24.8774609336491,2.36762524726719,7.86042682483797));
#45579=CARTESIAN_POINT('Ctrl Pts',(24.7192066240803,-0.503438716171723,
6.84878626071905));
#45580=CARTESIAN_POINT('Ctrl Pts',(24.5609523145115,-2.91632395158999,8.70450260617681));
#45581=CARTESIAN_POINT('Ctrl Pts',(24.4026980049428,-2.67573209543587,11.738925385597));
#45582=CARTESIAN_POINT('Ctrl Pts',(24.244443695374,-0.00049204071968808,
13.1911460478872));
#45583=CARTESIAN_POINT('Ctrl Pts',(24.0861893858052,2.67518097689384,11.7397630837433));
#45584=CARTESIAN_POINT('Ctrl Pts',(23.9279350762364,2.91674329140439,8.70539580650041));
#45585=CARTESIAN_POINT('Ctrl Pts',(23.7696807666676,0.504388325939132,6.84897110965841));
#45586=CARTESIAN_POINT('Ctrl Pts',(23.6114264570989,-2.36690208069152,7.85963565078572));
#45587=CARTESIAN_POINT('Ctrl Pts',(23.45317214753,-3.08457484919484,10.8177936267731));
#45588=CARTESIAN_POINT('Ctrl Pts',(23.2949178379613,-0.995625629036708,
13.0318505265147));
#45589=CARTESIAN_POINT('Ctrl Pts',(23.1366635283925,1.99923233833457,12.4872590088835));
#45590=CARTESIAN_POINT('Ctrl Pts',(22.9784092188237,3.17501048436542,9.67953745338411));
#45591=CARTESIAN_POINT('Ctrl Pts',(22.8201549092549,1.46188070997956,7.16340124230294));
#45592=CARTESIAN_POINT('Ctrl Pts',(22.6619005996861,-1.5813985363962,7.2282557275682));
#45593=CARTESIAN_POINT('Ctrl Pts',(22.5036462901173,-3.18578030836752,9.81509045229863));
#45594=CARTESIAN_POINT('Ctrl Pts',(22.3453919805486,-1.89145488008292,12.5701723933879));
#45595=CARTESIAN_POINT('Ctrl Pts',(22.1871376709798,1.12388496553606,12.986682150953));
#45596=CARTESIAN_POINT('Ctrl Pts',(22.028883361411,3.11661398903962,10.6856419910071));
#45597=CARTESIAN_POINT('Ctrl Pts',(21.8706290518422,2.27356951065551,7.76074356684863));
#45598=CARTESIAN_POINT('Ctrl Pts',(21.7123747422734,-0.638171376633541,
6.87332045351015));
#45599=CARTESIAN_POINT('Ctrl Pts',(21.5541204327046,-2.96924700231964,8.83082938244435));
#45600=CARTESIAN_POINT('Ctrl Pts',(21.3958661231359,-2.59863676139588,11.8521540636552));
#45601=CARTESIAN_POINT('Ctrl Pts',(21.2376118135671,0.136445079346075,13.188223711326));
#45602=CARTESIAN_POINT('Ctrl Pts',(21.0793575039983,2.74737701206447,11.6233629436748));
#45603=CARTESIAN_POINT('Ctrl Pts',(20.9211031944295,2.85850019278417,8.58142171838018));
#45604=CARTESIAN_POINT('Ctrl Pts',(20.7628488848607,0.36870483629377,6.83022959239551));
#45605=CARTESIAN_POINT('Ctrl Pts',(20.6045945752919,-2.4565710795211,7.96317741948034));
#45606=CARTESIAN_POINT('Ctrl Pts',(20.4463402657232,-3.0466394291865,10.9494081744789));
#45607=CARTESIAN_POINT('Ctrl Pts',(20.2880859561544,-0.86460337682645,13.0717826573543));
#45608=CARTESIAN_POINT('Ctrl Pts',(20.1298316465856,2.10412597568299,12.3991751857047));
#45609=CARTESIAN_POINT('Ctrl Pts',(19.9715773370168,3.15833376593105,9.54358405349603));
#45610=CARTESIAN_POINT('Ctrl Pts',(19.813323027448,1.33880768017961,7.10328087506992));
#45611=CARTESIAN_POINT('Ctrl Pts',(19.6550687178792,-1.69888509380567,7.29867122858234));
#45612=CARTESIAN_POINT('Ctrl Pts',(19.4968144083105,-3.19078061920234,9.95197153587308));
#45613=CARTESIAN_POINT('Ctrl Pts',(19.3385600987416,-1.77941922628463,12.6489724253703));
#45614=CARTESIAN_POINT('Ctrl Pts',(19.1803057891729,1.2510165549513,12.9357018364408));
#45615=CARTESIAN_POINT('Ctrl Pts',(19.0220514796041,3.14316584722257,10.5512677662419));
#45616=CARTESIAN_POINT('Ctrl Pts',(18.8637971700353,2.17538238935706,7.66524109310643));
#45617=CARTESIAN_POINT('Ctrl Pts',(18.7055428604665,-0.77175807408634,6.90358640225075));
#45618=CARTESIAN_POINT('Ctrl Pts',(18.5472885508978,-3.01668417833122,8.95932509329292));
#45619=CARTESIAN_POINT('Ctrl Pts',(18.389034241329,-2.51676184066121,11.9619626730994));
#45620=CARTESIAN_POINT('Ctrl Pts',(18.2307799317602,0.27313498841587,13.1794315484606));
#45621=CARTESIAN_POINT('Ctrl Pts',(18.0725256221914,2.81450923340181,11.5039699027373));
#45622=CARTESIAN_POINT('Ctrl Pts',(17.9142713126226,2.79499184128849,8.46006224139594));
#45623=CARTESIAN_POINT('Ctrl Pts',(17.7560170030538,0.232341476942896,6.81732736032501));
#45624=CARTESIAN_POINT('Ctrl Pts',(17.597762693485,-2.54171389478125,8.07047203432559));
#45625=CARTESIAN_POINT('Ctrl Pts',(17.4395083839162,-3.00309116980684,11.0792734218315));
#45626=CARTESIAN_POINT('Ctrl Pts',(17.2812540743475,-0.731988134966967,
13.1060555473963));
#45627=CARTESIAN_POINT('Ctrl Pts',(17.1229997647787,2.20514301981873,12.3066711849304));
#45628=CARTESIAN_POINT('Ctrl Pts',(16.9647454552099,3.13583829191377,9.40847155587319));
#45629=CARTESIAN_POINT('Ctrl Pts',(16.8064911456411,1.21326807752421,7.04849728692239));
#45630=CARTESIAN_POINT('Ctrl Pts',(16.6482368360723,-1.81324169279846,7.37406354670546));
#45631=CARTESIAN_POINT('Ctrl Pts',(16.4899825265035,-3.1899023768153,10.0889411020383));
#45632=CARTESIAN_POINT('Ctrl Pts',(16.3317282169347,-1.66410524580638,12.7228921065888));
#45633=CARTESIAN_POINT('Ctrl Pts',(16.173473907366,1.37584332470155,12.8793129109421));
#45634=CARTESIAN_POINT('Ctrl Pts',(16.0152195977972,3.16392687292691,10.4158779099864));
#45635=CARTESIAN_POINT('Ctrl Pts',(15.8569652882284,2.07318743733889,7.57404007805077));
#45636=CARTESIAN_POINT('Ctrl Pts',(15.6987109786596,-0.90392291770186,6.93955704969084));
#45637=CARTESIAN_POINT('Ctrl Pts',(15.5404566690908,-3.05856354585273,9.08973809855375));
#45638=CARTESIAN_POINT('Ctrl Pts',(15.3822023595221,-2.43025014665305,12.06815664734));
#45639=CARTESIAN_POINT('Ctrl Pts',(15.2239480499532,0.409321685371451,13.1647817383081));
#45640=CARTESIAN_POINT('Ctrl Pts',(15.0656937403845,2.87645612457767,11.38180601266));
#45641=CARTESIAN_POINT('Ctrl Pts',(14.9074394308157,2.72633411761815,8.34153987917857));
#45642=CARTESIAN_POINT('Ctrl Pts',(14.7491851212469,0.0955500616988636,
6.81028874677455));
#45643=CARTESIAN_POINT('Ctrl Pts',(14.5909308116781,-2.62217396621445,8.18132152810044));
#45644=CARTESIAN_POINT('Ctrl Pts',(14.4326765021093,-2.95401014504738,11.2071502624781));
#45645=CARTESIAN_POINT('Ctrl Pts',(14.2744221925406,-0.598024309804106,
13.1346059749396));
#45646=CARTESIAN_POINT('Ctrl Pts',(14.1161678829718,2.30209740376012,12.2099174728584));
#45647=CARTESIAN_POINT('Ctrl Pts',(13.957913573403,3.10756548495669,9.27444886469009));
#45648=CARTESIAN_POINT('Ctrl Pts',(13.7996592638342,1.08549320219973,6.99915141981115));
#45649=CARTESIAN_POINT('Ctrl Pts',(13.6414049542654,-1.92425765366397,7.45429377665825));
#45650=CARTESIAN_POINT('Ctrl Pts',(13.4831506446966,-3.18314719615494,10.2257468069615));
#45651=CARTESIAN_POINT('Ctrl Pts',(13.3248963351278,-1.54572538974549,12.7917952490713));
#45652=CARTESIAN_POINT('Ctrl Pts',(13.1666420255591,1.4981353001745,12.8176192637802));
#45653=CARTESIAN_POINT('Ctrl Pts',(13.0083877159903,3.17885881650219,10.2797218582409));
#45654=CARTESIAN_POINT('Ctrl Pts',(12.8501334064215,1.96717293439155,7.48730854671172));
#45655=CARTESIAN_POINT('Ctrl Pts',(12.6918790968527,-1.03442241280721,6.9811661249418));
#45656=CARTESIAN_POINT('Ctrl Pts',(12.5336247872839,-3.09480794807483,9.22182813101998));
#45657=CARTESIAN_POINT('Ctrl Pts',(12.3753704777151,-2.33926106483218,12.1705403391213));
#45658=CARTESIAN_POINT('Ctrl Pts',(12.2171161681464,0.54475426578949,13.1443012711322));
#45659=CARTESIAN_POINT('Ctrl Pts',(12.0588618585775,2.9331035572221,11.257096342769));
#45660=CARTESIAN_POINT('Ctrl Pts',(11.9006075490088,2.65265351396683,8.22607299247362));
#45661=CARTESIAN_POINT('Ctrl Pts',(11.74235323944,-0.0414173911698831,6.80912671887172));
#45662=CARTESIAN_POINT('Ctrl Pts',(11.5840989298712,-2.69780305704375,8.29552167746703));
#45663=CARTESIAN_POINT('Ctrl Pts',(11.4258446203024,-2.89948678085681,11.3328030997711));
#45664=CARTESIAN_POINT('Ctrl Pts',(11.2675903107337,-0.462958708208892,
13.1573813435356));
#45665=CARTESIAN_POINT('Ctrl Pts',(11.1093360011649,2.39481049852988,12.1090922973653));
#45666=CARTESIAN_POINT('Ctrl Pts',(10.9510816915961,3.07356744215081,9.14176291100341));
#45667=CARTESIAN_POINT('Ctrl Pts',(10.7928273820273,0.955718444758249,6.95533416054196));
#45668=CARTESIAN_POINT('Ctrl Pts',(10.6345730724585,-2.03172841389709,7.53921415558398));
#45669=CARTESIAN_POINT('Ctrl Pts',(10.4763187628897,-3.17052758332845,10.3621365097244));
#45670=CARTESIAN_POINT('Ctrl Pts',(10.3180644533209,-1.42449763922883,12.8555550935164));
#45671=CARTESIAN_POINT('Ctrl Pts',(10.1598101437521,1.61766695098797,12.7507342006546));
#45672=CARTESIAN_POINT('Ctrl Pts',(10.0015558341834,3.18793460113869,10.1430511446082));
#45673=CARTESIAN_POINT('Ctrl Pts',(9.84330152461458,1.85753336290945,7.4052049692784));
#45674=CARTESIAN_POINT('Ctrl Pts',(9.6850472150458,-1.16301452643865,7.02833951165627));
#45675=CARTESIAN_POINT('Ctrl Pts',(9.52679290547701,-3.12535370323928,9.35534693772645));
#45676=CARTESIAN_POINT('Ctrl Pts',(9.36853859590823,-2.2439562725775,12.2689345495142));
#45677=CARTESIAN_POINT('Ctrl Pts',(9.21028428633944,0.679171743027831,13.1180097228028));
#45678=CARTESIAN_POINT('Ctrl Pts',(9.05202997677066,2.9843692575704,11.1301056172068));
#45679=CARTESIAN_POINT('Ctrl Pts',(8.89377566720187,2.57404323488125,8.11380698009667));
#45680=CARTESIAN_POINT('Ctrl Pts',(8.73552135763309,-0.178226614346673,
6.81397308511794));
#45681=CARTESIAN_POINT('Ctrl Pts',(8.57726704806431,-2.76861960711876,8.41261234475057));
#45682=CARTESIAN_POINT('Ctrl Pts',(8.41901273849552,-2.83931758725479,11.456481704384));
#45683=CARTESIAN_POINT('Ctrl Pts',(8.26075842892673,-0.327626500506996,
13.1734097341694));
#45684=CARTESIAN_POINT('Ctrl Pts',(8.10250411935795,2.48425024167238,12.0062020922894));
#45685=CARTESIAN_POINT('Ctrl Pts',(7.94424980978916,3.03162302228778,9.00687161986933));
#45686=CARTESIAN_POINT('Ctrl Pts',(7.83874693674331,1.56351848868342,7.62023987234021));
#45687=CARTESIAN_POINT('Ctrl Pts',(7.78599550022038,0.698066426161017,7.38886781406139));
#45688=CARTESIAN_POINT('Ctrl Pts',(26.0922433505204,2.88336587074908,9.83354294895125));
#45689=CARTESIAN_POINT('Ctrl Pts',(26.0394919139975,2.82819417207855,8.87785983444456));
#45690=CARTESIAN_POINT('Ctrl Pts',(25.9339890409517,1.69422531913677,7.04193077437275));
#45691=CARTESIAN_POINT('Ctrl Pts',(25.7757347313828,-1.56283851628882,6.96682495909965));
#45692=CARTESIAN_POINT('Ctrl Pts',(25.6174804218141,-3.39176779696954,9.65732269963848));
#45693=CARTESIAN_POINT('Ctrl Pts',(25.4592261122453,-2.13758422374064,12.6567239048252));
#45694=CARTESIAN_POINT('Ctrl Pts',(25.3009718026765,1.06311546625041,13.2402942585496));
#45695=CARTESIAN_POINT('Ctrl Pts',(25.1427174931077,3.29569411247162,10.8747811831844));
#45696=CARTESIAN_POINT('Ctrl Pts',(24.9844631835389,2.52997335573122,7.71371625131757));
#45697=CARTESIAN_POINT('Ctrl Pts',(24.8262088739702,-0.537959518563222,
6.63270747437876));
#45698=CARTESIAN_POINT('Ctrl Pts',(24.6679545644013,-3.11629634069821,8.61567032511795));
#45699=CARTESIAN_POINT('Ctrl Pts',(24.5097002548326,-2.85920709636852,11.8581635325282));
#45700=CARTESIAN_POINT('Ctrl Pts',(24.3514459452638,-0.000525779961243345,
13.409962993392));
#45701=CARTESIAN_POINT('Ctrl Pts',(24.193191635695,2.85861818761752,11.8590586716524));
#45702=CARTESIAN_POINT('Ctrl Pts',(24.0349373261262,3.1167444346517,8.61662477220482));
#45703=CARTESIAN_POINT('Ctrl Pts',(23.8766830165574,0.538974243090536,6.63290499841343));
#45704=CARTESIAN_POINT('Ctrl Pts',(23.7184287069887,-2.52920060160962,7.71287082644543));
#45705=CARTESIAN_POINT('Ctrl Pts',(23.5601743974198,-3.29608420556807,10.8738697513937));
#45706=CARTESIAN_POINT('Ctrl Pts',(23.4019200878511,-1.06389569745188,13.2397445750738));
#45707=CARTESIAN_POINT('Ctrl Pts',(23.2436657782823,2.13631973799098,12.6578104066685));
#45708=CARTESIAN_POINT('Ctrl Pts',(23.0854114687135,3.39272101397104,9.65756333043674));
#45709=CARTESIAN_POINT('Ctrl Pts',(22.9271571591447,1.5621218982078,6.96889561126398));
#45710=CARTESIAN_POINT('Ctrl Pts',(22.768902849576,-1.6898350642665,7.03819716982359));
#45711=CARTESIAN_POINT('Ctrl Pts',(22.6106485400071,-3.40422932501084,9.80241120107808));
#45712=CARTESIAN_POINT('Ctrl Pts',(22.4523942304384,-2.02115197736677,12.7464091635333));
#45713=CARTESIAN_POINT('Ctrl Pts',(22.2941399208696,1.20094977910676,13.1914790031365));
#45714=CARTESIAN_POINT('Ctrl Pts',(22.1358856113008,3.33032026984446,10.732656475437));
#45715=CARTESIAN_POINT('Ctrl Pts',(21.977631301732,2.42946821546214,7.6071977104224));
#45716=CARTESIAN_POINT('Ctrl Pts',(21.8193769921633,-0.681930800128424,
6.65892397723854));
#45717=CARTESIAN_POINT('Ctrl Pts',(21.6611226825944,-3.17284832602806,8.750659330849));
#45718=CARTESIAN_POINT('Ctrl Pts',(21.5028683730257,-2.77682533379967,11.9791563032054));
#45719=CARTESIAN_POINT('Ctrl Pts',(21.3446140634568,0.145801121045086,13.4068402721569));
#45720=CARTESIAN_POINT('Ctrl Pts',(21.1863597538881,2.93576470629988,11.7346769717544));
#45721=CARTESIAN_POINT('Ctrl Pts',(21.0281054443193,3.05450760564573,8.48414977849232));
#45722=CARTESIAN_POINT('Ctrl Pts',(20.8698511347506,0.393986933966499,6.61287837495358));
#45723=CARTESIAN_POINT('Ctrl Pts',(20.7115968251817,-2.62501820540304,7.82351245619871));
#45724=CARTESIAN_POINT('Ctrl Pts',(20.553342515613,-3.25554755308459,11.0145091111515));
#45725=CARTESIAN_POINT('Ctrl Pts',(20.3950882060442,-0.923889246902975,
13.2824148528885));
#45726=CARTESIAN_POINT('Ctrl Pts',(20.2368338964754,2.2484059340575,12.5636866740505));
#45727=CARTESIAN_POINT('Ctrl Pts',(20.0785795869066,3.37490077263483,9.51228760331953));
#45728=CARTESIAN_POINT('Ctrl Pts',(19.9203252773378,1.43060974840183,6.90465278930053));
#45729=CARTESIAN_POINT('Ctrl Pts',(19.762070967769,-1.81537767716337,7.11344106308832));
#45730=CARTESIAN_POINT('Ctrl Pts',(19.6038166582003,-3.40957250725519,9.9486782231698));
#45731=CARTESIAN_POINT('Ctrl Pts',(19.4455623486315,-1.90143403664589,12.830612515215));
#45732=CARTESIAN_POINT('Ctrl Pts',(19.2873080390627,1.33679878403842,13.1370029674836));
#45733=CARTESIAN_POINT('Ctrl Pts',(19.1290537294939,3.35869278945057,10.589068207511));
#45734=CARTESIAN_POINT('Ctrl Pts',(18.9707994199251,2.32454840137932,7.50514663023009));
#45735=CARTESIAN_POINT('Ctrl Pts',(18.8125451103563,-0.824677539979167,
6.69126526266284));
#45736=CARTESIAN_POINT('Ctrl Pts',(18.6542908007876,-3.22353827010556,8.88796599504674));
#45737=CARTESIAN_POINT('Ctrl Pts',(18.4960364912188,-2.68933624818511,12.0964944910982));
#45738=CARTESIAN_POINT('Ctrl Pts',(18.33778218165,0.291863859792721,13.3974452305158));
#45739=CARTESIAN_POINT('Ctrl Pts',(18.1795278720812,3.00750018533761,11.6070971477175));
#45740=CARTESIAN_POINT('Ctrl Pts',(18.0212735625124,2.98664448527398,8.3544686798514));
#45741=CARTESIAN_POINT('Ctrl Pts',(17.8630192529436,0.248273136458253,6.59909143658335));
#45742=CARTESIAN_POINT('Ctrl Pts',(17.7047649433748,-2.71599926513316,7.93816426483493));
#45743=CARTESIAN_POINT('Ctrl Pts',(17.5465106338061,-3.20901318872681,11.1532792209976));
#45744=CARTESIAN_POINT('Ctrl Pts',(17.3882563242373,-0.78218057537415,13.3190378356558));
#45745=CARTESIAN_POINT('Ctrl Pts',(17.2300020146685,2.35634971884065,12.4648396721749));
#45746=CARTESIAN_POINT('Ctrl Pts',(17.0717477050997,3.35086278353417,9.36791043915191));
#45747=CARTESIAN_POINT('Ctrl Pts',(16.9134933955309,1.29646189279257,6.84611268946649));
#45748=CARTESIAN_POINT('Ctrl Pts',(16.7552390859622,-1.93757571033511,7.19400303390634));
#45749=CARTESIAN_POINT('Ctrl Pts',(16.5969847763933,-3.40863404377088,10.0950397951052));
#45750=CARTESIAN_POINT('Ctrl Pts',(16.4387304668246,-1.77821297432193,12.9096008703877));
#45751=CARTESIAN_POINT('Ctrl Pts',(16.2804761572558,1.4701849277766,13.0767474522856));
#45752=CARTESIAN_POINT('Ctrl Pts',(16.122221847687,3.38087739908433,10.444394666224));
#45753=CARTESIAN_POINT('Ctrl Pts',(15.9639675381182,2.21534593954773,7.40769195982868));
#45754=CARTESIAN_POINT('Ctrl Pts',(15.8057132285494,-0.965904929447833,
6.72970241808549));
#45755=CARTESIAN_POINT('Ctrl Pts',(15.6474589189806,-3.26828930665857,9.02732142257126));
#45756=CARTESIAN_POINT('Ctrl Pts',(15.4892046094119,-2.59689244566508,12.2099701881825));
#45757=CARTESIAN_POINT('Ctrl Pts',(15.3309502998431,0.437388881161856,13.381790882601));
#45758=CARTESIAN_POINT('Ctrl Pts',(15.1726959902743,3.07369477602556,11.4765564773624));
#45759=CARTESIAN_POINT('Ctrl Pts',(15.0144416807055,2.91327890017913,8.22781923699113));
#45760=CARTESIAN_POINT('Ctrl Pts',(14.8561873711367,0.102101931256069,6.59157018516719));
#45761=CARTESIAN_POINT('Ctrl Pts',(14.6979330615679,-2.80197648520258,8.0566147105169));
#45762=CARTESIAN_POINT('Ctrl Pts',(14.5396787519991,-3.15656667716138,11.2899245790518));
#45763=CARTESIAN_POINT('Ctrl Pts',(14.3814244424304,-0.639030848159055,
13.3495459665615));
#45764=CARTESIAN_POINT('Ctrl Pts',(14.2231701328616,2.45995226674225,12.3614515562165));
#45765=CARTESIAN_POINT('Ctrl Pts',(14.0649158232928,3.32065130966359,9.22469780947245));
#45766=CARTESIAN_POINT('Ctrl Pts',(13.906661513724,1.15992549182458,6.79338317530414));
#45767=CARTESIAN_POINT('Ctrl Pts',(13.7484072041552,-2.05620403775932,7.27973465226065));
#45768=CARTESIAN_POINT('Ctrl Pts',(13.5901528945864,-3.40141566024351,10.2412262698301));
#45769=CARTESIAN_POINT('Ctrl Pts',(13.4318985850176,-1.65171580926802,12.9832287026674));
#45770=CARTESIAN_POINT('Ctrl Pts',(13.2736442754489,1.60086246634544,13.0108234705585));
#45771=CARTESIAN_POINT('Ctrl Pts',(13.1153899658801,3.396833226316,10.2989023914076));
#45772=CARTESIAN_POINT('Ctrl Pts',(12.9571356563113,2.10206202010675,7.31501324572778));
#45773=CARTESIAN_POINT('Ctrl Pts',(12.7988813467425,-1.10535277742715,6.7741646284218));
#45774=CARTESIAN_POINT('Ctrl Pts',(12.6406270371737,-3.30701898823388,9.16846887108869));
#45775=CARTESIAN_POINT('Ctrl Pts',(12.482372727605,-2.49966424076443,12.3193743316664));
#45776=CARTESIAN_POINT('Ctrl Pts',(12.3241184180362,0.582108076208057,13.3599060693994));
#45777=CARTESIAN_POINT('Ctrl Pts',(12.1658641084674,3.13422652420927,11.3432954630231));
#45778=CARTESIAN_POINT('Ctrl Pts',(12.0076097988986,2.83454601612698,8.1044347836576));
#45779=CARTESIAN_POINT('Ctrl Pts',(11.8493554893298,-0.0442573824741247,
6.59032847698884));
#45780=CARTESIAN_POINT('Ctrl Pts',(11.691101179761,-2.88279146423575,8.17864556630858));
#45781=CARTESIAN_POINT('Ctrl Pts',(11.5328468701922,-3.098304644846,11.4241934337999));
#45782=CARTESIAN_POINT('Ctrl Pts',(11.3745925606235,-0.494703795680576,
13.3738830426176));
#45783=CARTESIAN_POINT('Ctrl Pts',(11.2163382510547,2.55902270019265,12.2537127965125));
#45784=CARTESIAN_POINT('Ctrl Pts',(11.0580839414859,3.28432202041261,9.08291357740508));
#45785=CARTESIAN_POINT('Ctrl Pts',(10.8998296319171,1.02125207678459,6.74656136572925));
#45786=CARTESIAN_POINT('Ctrl Pts',(10.7415753223483,-2.17104407007601,7.37047802319264));
#45787=CARTESIAN_POINT('Ctrl Pts',(10.5833210127795,-3.38793072032428,10.3869682171186));
#45788=CARTESIAN_POINT('Ctrl Pts',(10.4250667032107,-1.52217546958108,13.0513605608649));
#45789=CARTESIAN_POINT('Ctrl Pts',(10.266812393642,1.72859040474012,12.9393520973757));
#45790=CARTESIAN_POINT('Ctrl Pts',(10.1085580840732,3.40653133767851,10.1528601643285));
#45791=CARTESIAN_POINT('Ctrl Pts',(9.95030377450439,1.98490446111228,7.22727982442037));
#45792=CARTESIAN_POINT('Ctrl Pts',(9.79204946493561,-1.24276245474844,6.82457269516505));
#45793=CARTESIAN_POINT('Ctrl Pts',(9.63379515536682,-3.33965926641385,9.31114306492331));
#45794=CARTESIAN_POINT('Ctrl Pts',(9.47554084579804,-2.39782439708303,12.4245154349468));
#45795=CARTESIAN_POINT('Ctrl Pts',(9.31728653622925,0.725742562430119,13.3318117090984));
#45796=CARTESIAN_POINT('Ctrl Pts',(9.15903222666047,3.18900751461044,11.2075969809815));
#45797=CARTESIAN_POINT('Ctrl Pts',(9.00077791709168,2.7505454287018,7.98447068866592));
#45798=CARTESIAN_POINT('Ctrl Pts',(8.8425236075229,-0.190447616699357,6.5955071586612));
#45799=CARTESIAN_POINT('Ctrl Pts',(8.68426929795412,-2.95846390650311,8.30376514288603));
#45800=CARTESIAN_POINT('Ctrl Pts',(8.52601498838534,-3.03400964848852,11.5563526826953));
#45801=CARTESIAN_POINT('Ctrl Pts',(8.36776067881654,-0.350091855909584,
13.3910105003035));
#45802=CARTESIAN_POINT('Ctrl Pts',(8.20950636924776,2.65459532823215,12.1437674081077));
#45803=CARTESIAN_POINT('Ctrl Pts',(8.05125205967898,3.23950147087779,8.93877278785939));
#45804=CARTESIAN_POINT('Ctrl Pts',(7.94574918663312,1.67072898134026,7.45705967489569));
#45805=CARTESIAN_POINT('Ctrl Pts',(7.89299775011019,0.745932854346936,7.20982243015784));
#45806=CARTESIAN_POINT('Ctrl Pts',(26.1992456004102,3.06839113754307,9.82286141852444));
#45807=CARTESIAN_POINT('Ctrl Pts',(26.1464941638873,3.00967907711354,8.80585222499811));
#45808=CARTESIAN_POINT('Ctrl Pts',(26.0409912908414,1.80294356917313,6.85211180161624));
#45809=CARTESIAN_POINT('Ctrl Pts',(25.8827369812727,-1.66312568981951,6.77218645454191));
#45810=CARTESIAN_POINT('Ctrl Pts',(25.7244826717039,-3.60941715874633,9.63533313543961));
#45811=CARTESIAN_POINT('Ctrl Pts',(25.5662283621351,-2.27475276530677,12.8272055819078));
#45812=CARTESIAN_POINT('Ctrl Pts',(25.4079740525663,1.13133546731627,13.4482235802362));
#45813=CARTESIAN_POINT('Ctrl Pts',(25.2497197429975,3.5071784366143,10.9309157942814));
#45814=CARTESIAN_POINT('Ctrl Pts',(25.0914654334287,2.69232146419524,7.56700567779718));
#45815=CARTESIAN_POINT('Ctrl Pts',(24.93321112386,-0.572480320954722,6.41662868803847));
#45816=CARTESIAN_POINT('Ctrl Pts',(24.7749568142912,-3.31626872980643,8.5268380440591));
#45817=CARTESIAN_POINT('Ctrl Pts',(24.6167025047224,-3.04268209730116,11.9774016794594));
#45818=CARTESIAN_POINT('Ctrl Pts',(24.4584481951536,-0.000559519202797285,
13.6287799388967));
#45819=CARTESIAN_POINT('Ctrl Pts',(24.3001938855848,3.04205539834121,11.9783542595615));
#45820=CARTESIAN_POINT('Ctrl Pts',(24.141939576016,3.31674557789901,8.52785373790922));
#45821=CARTESIAN_POINT('Ctrl Pts',(23.9836852664473,0.573560160241939,6.41683888716847));
#45822=CARTESIAN_POINT('Ctrl Pts',(23.8254309568785,-2.69149912252773,7.56610600210514));
#45823=CARTESIAN_POINT('Ctrl Pts',(23.6671766473097,-3.5075935619413,10.9299458760143));
#45824=CARTESIAN_POINT('Ctrl Pts',(23.5089223377409,-1.13216576586705,13.447638623633));
#45825=CARTESIAN_POINT('Ctrl Pts',(23.3506680281721,2.27340713764739,12.8283618044535));
#45826=CARTESIAN_POINT('Ctrl Pts',(23.1924137186033,3.61043154357666,9.63558920748943));
#45827=CARTESIAN_POINT('Ctrl Pts',(23.0341594090345,1.66236308643603,6.77438998022499));
#45828=CARTESIAN_POINT('Ctrl Pts',(22.8759050994658,-1.79827159213679,6.848138612079));
#45829=CARTESIAN_POINT('Ctrl Pts',(22.7176507898969,-3.62267834165416,9.7897319498575));
#45830=CARTESIAN_POINT('Ctrl Pts',(22.5593964803283,-2.15084907465062,12.9226459336786));
#45831=CARTESIAN_POINT('Ctrl Pts',(22.4011421707594,1.27801459267746,13.39627585532));
#45832=CARTESIAN_POINT('Ctrl Pts',(22.2428878611907,3.5440265506493,10.7796709598669));
#45833=CARTESIAN_POINT('Ctrl Pts',(22.0846335516218,2.58536692026875,7.45365185399615));
#45834=CARTESIAN_POINT('Ctrl Pts',(21.9263792420531,-0.725690223623306,
6.44452750096693));
#45835=CARTESIAN_POINT('Ctrl Pts',(21.7681249324843,-3.37644964973648,8.67048927925364));
#45836=CARTESIAN_POINT('Ctrl Pts',(21.6098706229155,-2.95501390620346,12.1061585427555));
#45837=CARTESIAN_POINT('Ctrl Pts',(21.4516163133467,0.155157162744094,13.6254568329877));
#45838=CARTESIAN_POINT('Ctrl Pts',(21.2933620037779,3.1241524005353,11.845990999834));
#45839=CARTESIAN_POINT('Ctrl Pts',(21.1351076942091,3.2505150185073,8.38687783860446));
#45840=CARTESIAN_POINT('Ctrl Pts',(20.9768533846404,0.419269031639233,6.39552715751162));
#45841=CARTESIAN_POINT('Ctrl Pts',(20.8185990750715,-2.79346533128499,7.6838474929171));
#45842=CARTESIAN_POINT('Ctrl Pts',(20.6603447655028,-3.46445567698268,11.0796100478242));
#45843=CARTESIAN_POINT('Ctrl Pts',(20.502090455934,-0.983175116979502,13.4930470484227));
#45844=CARTESIAN_POINT('Ctrl Pts',(20.3438361463652,2.39268589243202,12.7281981623963));
#45845=CARTESIAN_POINT('Ctrl Pts',(20.1855818367964,3.59146777933862,9.48099115314302));
#45846=CARTESIAN_POINT('Ctrl Pts',(20.0273275272277,1.52241181662405,6.70602470353113));
#45847=CARTESIAN_POINT('Ctrl Pts',(19.8690732176588,-1.93187026052108,6.9282108975943));
#45848=CARTESIAN_POINT('Ctrl Pts',(19.7108189080901,-3.62836439530803,9.94538491046653));
#45849=CARTESIAN_POINT('Ctrl Pts',(19.5525645985213,-2.02344884700714,13.0122526050597));
#45850=CARTESIAN_POINT('Ctrl Pts',(19.3943102889525,1.42258101312554,13.3383040985265));
#45851=CARTESIAN_POINT('Ctrl Pts',(19.2360559793837,3.57421973167857,10.6268686487801));
#45852=CARTESIAN_POINT('Ctrl Pts',(19.0778016698149,2.47371441340158,7.34505216735374));
#45853=CARTESIAN_POINT('Ctrl Pts',(18.9195473602461,-0.877597005871997,
6.47894412307493));
#45854=CARTESIAN_POINT('Ctrl Pts',(18.7612930506773,-3.43039236187988,8.81660689680056));
#45855=CARTESIAN_POINT('Ctrl Pts',(18.6030387411086,-2.86191065570903,12.231026309097));
#45856=CARTESIAN_POINT('Ctrl Pts',(18.4447844315398,0.31059273116958,13.6154589125709));
#45857=CARTESIAN_POINT('Ctrl Pts',(18.286530121971,3.2004911372734,11.7102243926977));
#45858=CARTESIAN_POINT('Ctrl Pts',(18.1282758124023,3.17829712925949,8.24887511830688));
#45859=CARTESIAN_POINT('Ctrl Pts',(17.9700215028334,0.264204795973602,6.38085551284168));
#45860=CARTESIAN_POINT('Ctrl Pts',(17.8117671932647,-2.89028463548505,7.80585649534429));
#45861=CARTESIAN_POINT('Ctrl Pts',(17.6535128836959,-3.41493520764679,11.2272850201637));
#45862=CARTESIAN_POINT('Ctrl Pts',(17.4952585741271,-0.832373015781326,
13.5320201239153));
#45863=CARTESIAN_POINT('Ctrl Pts',(17.3370042645583,2.50755641786257,12.6230081594193));
#45864=CARTESIAN_POINT('Ctrl Pts',(17.1787499549895,3.56588727515458,9.32734932243063));
#45865=CARTESIAN_POINT('Ctrl Pts',(17.0204956454207,1.37965570806092,6.64372809201059));
#45866=CARTESIAN_POINT('Ctrl Pts',(16.862241335852,-2.06190972787176,7.0139425211072));
#45867=CARTESIAN_POINT('Ctrl Pts',(16.7039870262831,-3.62736571072646,10.1011384881722));
#45868=CARTESIAN_POINT('Ctrl Pts',(16.5457327167144,-1.89232070283748,13.0963096341866));
#45869=CARTESIAN_POINT('Ctrl Pts',(16.3874784071456,1.56452653085165,13.2741819936291));
#45870=CARTESIAN_POINT('Ctrl Pts',(16.2292240975768,3.59782792524174,10.4729114224616));
#45871=CARTESIAN_POINT('Ctrl Pts',(16.070969788008,2.35750444175658,7.24134384160661));
#45872=CARTESIAN_POINT('Ctrl Pts',(15.9127154784392,-1.02788694119381,6.51984778648015));
#45873=CARTESIAN_POINT('Ctrl Pts',(15.7544611688705,-3.4780150674644,8.96490474658875));
#45874=CARTESIAN_POINT('Ctrl Pts',(15.5962068593017,-2.76353474467712,12.3517837290249));
#45875=CARTESIAN_POINT('Ctrl Pts',(15.4379525497329,0.465456076952267,13.598800026894));
#45876=CARTESIAN_POINT('Ctrl Pts',(15.2796982401641,3.27093342747344,11.5713069420647));
#45877=CARTESIAN_POINT('Ctrl Pts',(15.1214439305953,3.10022368274011,8.11409859480372));
#45878=CARTESIAN_POINT('Ctrl Pts',(14.9631896210265,0.108653800813268,6.37285162355982));
#45879=CARTESIAN_POINT('Ctrl Pts',(14.8049353114577,-2.98177900419071,7.93190789293335));
#45880=CARTESIAN_POINT('Ctrl Pts',(14.6466810018889,-3.35912320927538,11.3726988956255));
#45881=CARTESIAN_POINT('Ctrl Pts',(14.4884266923202,-0.680037386513999,
13.5644859581834));
#45882=CARTESIAN_POINT('Ctrl Pts',(14.3301723827514,2.61780712972438,12.5129856395747));
#45883=CARTESIAN_POINT('Ctrl Pts',(14.1719180731826,3.53373713437049,9.17494675425479));
#45884=CARTESIAN_POINT('Ctrl Pts',(14.0136637636138,1.23435778144942,6.58761493079715));
#45885=CARTESIAN_POINT('Ctrl Pts',(13.855409454045,-2.18815042185467,7.10517552786303));
#45886=CARTESIAN_POINT('Ctrl Pts',(13.6971551444763,-3.61968412433208,10.2567057326988));
#45887=CARTESIAN_POINT('Ctrl Pts',(13.5389008349074,-1.75770622879056,13.1746621562634));
#45888=CARTESIAN_POINT('Ctrl Pts',(13.3806465253387,1.70358963251637,13.2040276773368));
#45889=CARTESIAN_POINT('Ctrl Pts',(13.2223922157699,3.6148076361298,10.3180829245743));
#45890=CARTESIAN_POINT('Ctrl Pts',(13.0641379062011,2.23695110582196,7.14271794474384));
#45891=CARTESIAN_POINT('Ctrl Pts',(12.9058835966323,-1.17628314204709,6.5671631319018));
#45892=CARTESIAN_POINT('Ctrl Pts',(12.7476292870635,-3.51923002839292,9.11510961115741));
#45893=CARTESIAN_POINT('Ctrl Pts',(12.5893749774948,-2.66006741669669,12.4682083242114));
#45894=CARTESIAN_POINT('Ctrl Pts',(12.431120667926,0.619461886626625,13.5755108676666));
#45895=CARTESIAN_POINT('Ctrl Pts',(12.2728663583572,3.33534949119645,11.4294945832771));
#45896=CARTESIAN_POINT('Ctrl Pts',(12.1146120487884,3.01643851828712,7.98279657484158));
#45897=CARTESIAN_POINT('Ctrl Pts',(11.9563577392196,-0.047097373778369,
6.37153023510597));
#45898=CARTESIAN_POINT('Ctrl Pts',(11.7981034296508,-3.06777987142775,8.06176945515013));
#45899=CARTESIAN_POINT('Ctrl Pts',(11.639849120082,-3.2971225088352,11.5155837678287));
#45900=CARTESIAN_POINT('Ctrl Pts',(11.4815948105133,-0.526448883152259,
13.5903847416995));
#45901=CARTESIAN_POINT('Ctrl Pts',(11.3233405009445,2.72323490185543,12.3983332956597));
#45902=CARTESIAN_POINT('Ctrl Pts',(11.1650861913757,3.49507659867442,9.02406424380673));
#45903=CARTESIAN_POINT('Ctrl Pts',(11.0068318818069,1.08678570881093,6.53778857091659));
#45904=CARTESIAN_POINT('Ctrl Pts',(10.8485775722381,-2.31035972625494,7.20174189080126));
#45905=CARTESIAN_POINT('Ctrl Pts',(10.6903232626693,-3.60533385732009,10.411799924513));
#45906=CARTESIAN_POINT('Ctrl Pts',(10.5320689531006,-1.61985329993334,13.2471660282134));
#45907=CARTESIAN_POINT('Ctrl Pts',(10.3738146435318,1.83951385849227,13.127969994097));
#45908=CARTESIAN_POINT('Ctrl Pts',(10.215560333963,3.62512807421833,10.1626691840488));
#45909=CARTESIAN_POINT('Ctrl Pts',(10.0573060243942,2.11227555931511,7.04935467956235));
#45910=CARTESIAN_POINT('Ctrl Pts',(9.89905171482542,-1.32251038305822,6.62080587867383));
#45911=CARTESIAN_POINT('Ctrl Pts',(9.74079740525663,-3.55396482958843,9.2669391921202));
#45912=CARTESIAN_POINT('Ctrl Pts',(9.58254309568785,-2.55169252158856,12.5800963203793));
#45913=CARTESIAN_POINT('Ctrl Pts',(9.42428878611906,0.772313381832412,13.5456136953941));
#45914=CARTESIAN_POINT('Ctrl Pts',(9.26603447655028,3.39364577165048,11.2850883447562));
#45915=CARTESIAN_POINT('Ctrl Pts',(9.1077801669815,2.92704762252235,7.85513439723516));
#45916=CARTESIAN_POINT('Ctrl Pts',(8.94952585741271,-0.20266861905204,6.37704123220448));
#45917=CARTESIAN_POINT('Ctrl Pts',(8.79127154784393,-3.14830820588747,8.19491794102147));
#45918=CARTESIAN_POINT('Ctrl Pts',(8.63301723827514,-3.22870170972224,11.6562236610067));
#45919=CARTESIAN_POINT('Ctrl Pts',(8.47476292870636,-0.372557211312175,
13.6086112664375));
#45920=CARTESIAN_POINT('Ctrl Pts',(8.31650861913757,2.82494041479191,12.281332723926));
#45921=CARTESIAN_POINT('Ctrl Pts',(8.15825430956879,3.44737991946778,8.87067395584943));
#45922=CARTESIAN_POINT('Ctrl Pts',(8.05275143652293,1.7779394739971,7.29387947745118));
#45923=CARTESIAN_POINT('Ctrl Pts',(8.,0.793799282532855,7.0307770462543));
#45924=CARTESIAN_POINT('Ctrl Pts',(25.8782388507408,2.51331533716111,9.85490600980487));
#45925=CARTESIAN_POINT('Ctrl Pts',(25.8769239147893,2.52685451631763,9.54765567369101));
#45926=CARTESIAN_POINT('Ctrl Pts',(25.8804442384711,2.49183285130677,9.23944408489687));
#45927=CARTESIAN_POINT('Ctrl Pts',(25.8965480296803,2.31890412387178,8.60639456830937));
#45928=CARTESIAN_POINT('Ctrl Pts',(25.9101919837067,2.16864405658939,8.28772728731036));
#45929=CARTESIAN_POINT('Ctrl Pts',(25.9371024584265,1.81388157912996,7.7895766632932));
#45930=CARTESIAN_POINT('Ctrl Pts',(25.9495040585495,1.63266221909673,7.59663063038989));
#45931=CARTESIAN_POINT('Ctrl Pts',(25.9737270380795,1.19204230912881,7.24399771550759));
#45932=CARTESIAN_POINT('Ctrl Pts',(25.9849858624053,0.928010439591528,7.09546117333466));
#45933=CARTESIAN_POINT('Ctrl Pts',(25.9920223077014,0.644031331499198,6.99473364008323));
#45934=CARTESIAN_POINT('Ctrl Pts',(24.387416697508,-2.51385573226095,9.99896352468483));
#45935=CARTESIAN_POINT('Ctrl Pts',(24.4095944865459,-2.51517282451638,9.64697137526858));
#45936=CARTESIAN_POINT('Ctrl Pts',(24.4317722755838,-2.44620577848239,9.29547212983497));
#45937=CARTESIAN_POINT('Ctrl Pts',(24.4539500646217,-2.30443020970175,8.97631530577795));
#45938=CARTESIAN_POINT('Ctrl Pts',(24.5067015011447,-1.96720701291458,8.21717827384355));
#45939=CARTESIAN_POINT('Ctrl Pts',(24.5594529376676,-1.2180624633474,7.64102166045144));
#45940=CARTESIAN_POINT('Ctrl Pts',(24.6122043741905,-0.397791013133248,
7.50998874563856));
#45941=CARTESIAN_POINT('Ctrl Pts',(24.6649558107135,0.422480437080906,7.37895583082568));
#45942=CARTESIAN_POINT('Ctrl Pts',(24.7177072472364,1.31387878794203,7.69304661459202));
#45943=CARTESIAN_POINT('Ctrl Pts',(24.7704586837593,1.87081935093645,8.30932110024717));
#45944=CARTESIAN_POINT('Ctrl Pts',(24.8232101202822,2.42775991393086,8.92559558590231));
#45945=CARTESIAN_POINT('Ctrl Pts',(24.8759615568051,2.65024268905857,9.84405377344627));
#45946=CARTESIAN_POINT('Ctrl Pts',(24.9287129933281,2.43714240994448,10.6469368095826));
#45947=CARTESIAN_POINT('Ctrl Pts',(24.981464429851,2.2240421308304,11.4498198457189));
#45948=CARTESIAN_POINT('Ctrl Pts',(25.034215866374,1.57535879747453,12.1371277304477));
#45949=CARTESIAN_POINT('Ctrl Pts',(25.0869673028969,0.786030030008762,12.3960024953926));
#45950=CARTESIAN_POINT('Ctrl Pts',(25.1397187394198,-0.00329873745700912,
12.6548772603375));
#45951=CARTESIAN_POINT('Ctrl Pts',(25.1924701759427,-0.933272939032685,
12.4853189054987));
#45952=CARTESIAN_POINT('Ctrl Pts',(25.2452216124657,-1.58046369528845,11.964796607642));
#45953=CARTESIAN_POINT('Ctrl Pts',(25.2926199741465,-2.16197926270129,11.4970955218905));
#45954=CARTESIAN_POINT('Ctrl Pts',(25.3400183358272,-2.51519159740436,10.7460461564513));
#45955=CARTESIAN_POINT('Ctrl Pts',(25.387416697508,-2.52031926711485,9.99879747833012));
#45956=CARTESIAN_POINT('Ctrl Pts',(8.,0.793799282532855,7.0307770462543));
#45957=CARTESIAN_POINT('Ctrl Pts',(8.,0.888651840235432,7.06547453556552));
#45958=CARTESIAN_POINT('Ctrl Pts',(8.00000000000001,0.981460615688964,7.10515936495498));
#45959=CARTESIAN_POINT('Ctrl Pts',(8.00000000000001,1.071984630131,7.14951198682703));
#45960=CARTESIAN_POINT('Ctrl Pts',(8.00000000000001,1.16377090416436,7.19448305809844));
#45961=CARTESIAN_POINT('Ctrl Pts',(8.,1.25320892391096,7.24425370524276));
#45962=CARTESIAN_POINT('Ctrl Pts',(8.,1.3400134543598,7.29853149073832));
#45963=CARTESIAN_POINT('Ctrl Pts',(8.,1.36448894626115,7.31383570922151));
#45964=CARTESIAN_POINT('Ctrl Pts',(8.,1.38875483117205,7.32949846326485));
#45965=CARTESIAN_POINT('Ctrl Pts',(8.,1.41280412179919,7.34551365083284));
#45966=CARTESIAN_POINT('Ctrl Pts',(8.,1.43214636521133,7.3583942659426));
#45967=CARTESIAN_POINT('Ctrl Pts',(8.00000000000001,1.45135061788146,7.37150448852873));
#45968=CARTESIAN_POINT('Ctrl Pts',(8.00000000000001,1.47039392887492,7.38482736395197));
#45969=CARTESIAN_POINT('Ctrl Pts',(8.00000000000001,1.55310526312923,7.44269297370535));
#45970=CARTESIAN_POINT('Ctrl Pts',(8.00000000000001,1.63286195332271,7.50461801758942));
#45971=CARTESIAN_POINT('Ctrl Pts',(8.00000000000001,1.70939770627191,7.570306093392));
#45972=CARTESIAN_POINT('Ctrl Pts',(8.00000000000001,1.76856435887146,7.62108685154987));
#45973=CARTESIAN_POINT('Ctrl Pts',(8.00000000000001,1.82580548371507,7.67411738544499));
#45974=CARTESIAN_POINT('Ctrl Pts',(8.00000000000001,1.8809803115492,7.72927264183758));
#45975=CARTESIAN_POINT('Ctrl Pts',(8.00000000000001,1.91054892908599,7.75883077088729));
#45976=CARTESIAN_POINT('Ctrl Pts',(8.00000000000001,1.93952383038483,7.78899926613622));
#45977=CARTESIAN_POINT('Ctrl Pts',(8.00000000000001,1.96788125663504,7.81975974016046));
#45978=CARTESIAN_POINT('Ctrl Pts',(8.00000000000001,1.97854463399386,7.8313267469601));
#45979=CARTESIAN_POINT('Ctrl Pts',(8.00000000000001,1.98911861632425,7.84297530088787));
#45980=CARTESIAN_POINT('Ctrl Pts',(8.00000000000001,1.99959529223268,7.85469662340685));
#45981=CARTESIAN_POINT('Ctrl Pts',(8.00000000000001,2.06523110597061,7.92813008153257));
#45982=CARTESIAN_POINT('Ctrl Pts',(8.,2.12713067340333,8.00450310115816));
#45983=CARTESIAN_POINT('Ctrl Pts',(8.,2.18504938463886,8.08353870982025));
#45984=CARTESIAN_POINT('Ctrl Pts',(8.,2.24239481491336,8.16179202190283));
#45985=CARTESIAN_POINT('Ctrl Pts',(8.00000000000001,2.29583822969202,8.24265625774018));
#45986=CARTESIAN_POINT('Ctrl Pts',(8.00000000000001,2.34509645146655,8.32588467382346));
#45987=CARTESIAN_POINT('Ctrl Pts',(8.00000000000001,2.39296142701126,8.40675901229807));
#45988=CARTESIAN_POINT('Ctrl Pts',(8.,2.43687482302416,8.48986637651382));
#45989=CARTESIAN_POINT('Ctrl Pts',(8.,2.47652901207894,8.57499049794785));
#45990=CARTESIAN_POINT('Ctrl Pts',(8.,2.49722179256097,8.61941089338518));
#45991=CARTESIAN_POINT('Ctrl Pts',(8.,2.51675394122296,8.66438057335268));
#45992=CARTESIAN_POINT('Ctrl Pts',(8.,2.53507605865623,8.70986902566855));
#45993=CARTESIAN_POINT('Ctrl Pts',(8.,2.54220474646394,8.72756746999938));
#45994=CARTESIAN_POINT('Ctrl Pts',(8.00000000000001,2.54915021624124,8.74534444465406));
#45995=CARTESIAN_POINT('Ctrl Pts',(8.00000000000001,2.55590938804843,8.76319814293423));
#45996=CARTESIAN_POINT('Ctrl Pts',(8.00000000000001,2.56088080950049,8.77632967164225));
#45997=CARTESIAN_POINT('Ctrl Pts',(8.00000000000001,2.565750374188,8.78950002479304));
#45998=CARTESIAN_POINT('Ctrl Pts',(8.00000000000001,2.57051357424907,8.80269860187458));
#45999=CARTESIAN_POINT('Ctrl Pts',(8.00000000000001,2.60204053185424,8.89005814477923));
#46000=CARTESIAN_POINT('Ctrl Pts',(8.00000000000001,2.62895893279742,8.97877679643224));
#46001=CARTESIAN_POINT('Ctrl Pts',(8.00000000000001,2.65101703259939,9.06863225769505));
#46002=CARTESIAN_POINT('Ctrl Pts',(8.00000000000001,2.65603223898398,9.08906210827427));
#46003=CARTESIAN_POINT('Ctrl Pts',(8.,2.66079598776046,9.10955076534661));
#46004=CARTESIAN_POINT('Ctrl Pts',(8.,2.66530494352163,9.13009567307715));
#46005=CARTESIAN_POINT('Ctrl Pts',(8.,2.68549215663049,9.22207804164026));
#46006=CARTESIAN_POINT('Ctrl Pts',(8.,2.70057625721049,9.31518827802502));
#46007=CARTESIAN_POINT('Ctrl Pts',(8.,2.71066780876488,9.40903345925902));
#46008=CARTESIAN_POINT('Ctrl Pts',(8.,2.7212185892897,9.50714918558466));
#46009=CARTESIAN_POINT('Ctrl Pts',(8.,2.72631209524207,9.60606952165998));
#46010=CARTESIAN_POINT('Ctrl Pts',(8.,2.72601695513705,9.70533038478544));
#46011=CARTESIAN_POINT('Ctrl Pts',(8.,2.72591332999743,9.74018136106902));
#46012=CARTESIAN_POINT('Ctrl Pts',(8.00000000000001,2.72514492076099,9.77507409305378));
#46013=CARTESIAN_POINT('Ctrl Pts',(8.00000000000001,2.72371312681726,9.80998762211471));
#46014=CARTESIAN_POINT('Ctrl Pts',(8.00000000000001,2.72312104730935,9.82442516405044));
#46015=CARTESIAN_POINT('Ctrl Pts',(8.,2.72241541659262,9.83886678055821));
#46016=CARTESIAN_POINT('Ctrl Pts',(8.,2.72159739125326,9.85329547547575));
#46017=CARTESIAN_POINT('Ctrl Pts',(8.,2.71633099801499,9.9461864627038));
#46018=CARTESIAN_POINT('Ctrl Pts',(8.,2.70640503210548,10.0386981093905));
#46019=CARTESIAN_POINT('Ctrl Pts',(8.,2.69194454036193,10.1304577877966));
#46020=CARTESIAN_POINT('Ctrl Pts',(8.,2.67751755146885,10.2220048724098));
#46021=CARTESIAN_POINT('Ctrl Pts',(8.,2.65857661117198,10.3128044168814));
#46022=CARTESIAN_POINT('Ctrl Pts',(8.,2.63519721280128,10.4024694307445));
#46023=CARTESIAN_POINT('Ctrl Pts',(8.,2.61221588141411,10.4906077722342));
#46024=CARTESIAN_POINT('Ctrl Pts',(8.,2.58494547647907,10.5776506751394));
#46025=CARTESIAN_POINT('Ctrl Pts',(8.,2.55341730266435,10.663201462517));
#46026=CARTESIAN_POINT('Ctrl Pts',(8.,2.53742523481517,10.7065954758949));
#46027=CARTESIAN_POINT('Ctrl Pts',(8.,2.52033710900699,10.7496050527093));
#46028=CARTESIAN_POINT('Ctrl Pts',(8.,2.50215350356533,10.792174520464));
#46029=CARTESIAN_POINT('Ctrl Pts',(8.,2.49664128219483,10.8050791300939));
#46030=CARTESIAN_POINT('Ctrl Pts',(8.00000000000001,2.49102837597118,10.8179432750348));
#46031=CARTESIAN_POINT('Ctrl Pts',(8.00000000000001,2.48531476150017,10.830765348423));
#46032=CARTESIAN_POINT('Ctrl Pts',(8.00000000000001,2.47974569525222,10.8432630373198));
#46033=CARTESIAN_POINT('Ctrl Pts',(8.,2.47408470333919,10.8557123142945));
#46034=CARTESIAN_POINT('Ctrl Pts',(8.,2.46833291255443,10.8681102233784));
#46035=CARTESIAN_POINT('Ctrl Pts',(8.,2.43083362022605,10.948939452812));
#46036=CARTESIAN_POINT('Ctrl Pts',(8.,2.38946742072689,11.0276121176187));
#46037=CARTESIAN_POINT('Ctrl Pts',(8.,2.34430545470983,11.1037797259104));
#46038=CARTESIAN_POINT('Ctrl Pts',(8.,2.29990596796576,11.1786613799419));
#46039=CARTESIAN_POINT('Ctrl Pts',(8.,2.25183734528232,11.2511225203992));
#46040=CARTESIAN_POINT('Ctrl Pts',(8.,2.20013104971758,11.3207978239273));
#46041=CARTESIAN_POINT('Ctrl Pts',(8.,2.15002363316517,11.3883186048915));
#46042=CARTESIAN_POINT('Ctrl Pts',(8.,2.09649959036919,11.4532236127033));
#46043=CARTESIAN_POINT('Ctrl Pts',(8.,2.03955998698964,11.5151401317574));
#46044=CARTESIAN_POINT('Ctrl Pts',(8.,2.01641826334308,11.5403046023203));
#46045=CARTESIAN_POINT('Ctrl Pts',(8.,1.99271206342713,11.5649749200134));
#46046=CARTESIAN_POINT('Ctrl Pts',(8.,1.9684403447054,11.5891238290966));
#46047=CARTESIAN_POINT('Ctrl Pts',(8.,1.95158317542738,11.6058957047499));
#46048=CARTESIAN_POINT('Ctrl Pts',(8.,1.93445320326802,11.622416041126));
#46049=CARTESIAN_POINT('Ctrl Pts',(8.,1.91705735205381,11.6386813803728));
#46050=CARTESIAN_POINT('Ctrl Pts',(25.7084234471775,-3.07694191359583,9.99853189658296));
#46051=CARTESIAN_POINT('Ctrl Pts',(25.6610250854967,-3.07068177740707,10.9108134505871));
#46052=CARTESIAN_POINT('Ctrl Pts',(25.560875287293,-2.15953918737736,12.8482119976726));
#46053=CARTESIAN_POINT('Ctrl Pts',(25.4079740525663,1.13133546731627,13.4482235802362));
#46054=CARTESIAN_POINT('Ctrl Pts',(25.2497197429975,3.5071784366143,10.9309157942814));
#46055=CARTESIAN_POINT('Ctrl Pts',(25.0914654334287,2.69232146419524,7.56700567779718));
#46056=CARTESIAN_POINT('Ctrl Pts',(24.93321112386,-0.572480320954722,6.41662868803847));
#46057=CARTESIAN_POINT('Ctrl Pts',(24.8055304617762,-2.7861876229203,8.119160065833));
#46058=CARTESIAN_POINT('Ctrl Pts',(24.7306012362154,-3.07065885845128,9.56900358366952));
#46059=CARTESIAN_POINT('Ctrl Pts',(24.7084234471775,-3.06905088107409,9.99873461494295));
#46060=CARTESIAN_POINT('Origin',(28.2084234471774,0.,10.));
#46061=CARTESIAN_POINT('Ctrl Pts',(25.7915765528226,-3.07002654794609,10.0000640341964));
#46062=CARTESIAN_POINT('Ctrl Pts',(25.7505300621955,-3.06421617930135,10.7929818643657));
#46063=CARTESIAN_POINT('Ctrl Pts',(25.6568828586135,-2.35442447610646,12.6045285619815));
#46064=CARTESIAN_POINT('Ctrl Pts',(25.5106349420764,0.701596196644071,13.5590880549712));
#46065=CARTESIAN_POINT('Ctrl Pts',(25.3528328032114,3.3594675732725,11.3600672948067));
#46066=CARTESIAN_POINT('Ctrl Pts',(25.1950306643464,2.97881274377391,7.93379586486837));
#46067=CARTESIAN_POINT('Ctrl Pts',(25.0372285254814,-0.0991962456131474,
6.3757557658597));
#46068=CARTESIAN_POINT('Ctrl Pts',(24.9027438216401,-2.64536456776374,7.84448501581014));
#46069=CARTESIAN_POINT('Ctrl Pts',(24.8208598307538,-3.06731791981827,9.43344524461191));
#46070=CARTESIAN_POINT('Ctrl Pts',(24.7915765528225,-3.06884999403827,10.0009308069803));
#46071=CARTESIAN_POINT('Ctrl Pts',(25.8262392198064,-3.0008944935354,9.33589572455155));
#46072=CARTESIAN_POINT('Ctrl Pts',(25.7736385068514,-3.22038097435984,10.3276914350471));
#46073=CARTESIAN_POINT('Ctrl Pts',(25.6684370809415,-2.59586341847174,12.5291142048513));
#46074=CARTESIAN_POINT('Ctrl Pts',(25.5106349420764,0.701596196644071,13.5590880549712));
#46075=CARTESIAN_POINT('Ctrl Pts',(25.3528328032114,3.3594675732725,11.3600672948067));
#46076=CARTESIAN_POINT('Ctrl Pts',(25.1950306643464,2.97881274377391,7.93379586486837));
#46077=CARTESIAN_POINT('Ctrl Pts',(25.0372285254814,-0.0991962456131474,
6.3757557658597));
#46078=CARTESIAN_POINT('Ctrl Pts',(24.8794263866164,-3.08682826374848,8.09913850334405));
#46079=CARTESIAN_POINT('Ctrl Pts',(24.7216242477514,-3.28078721105507,11.5425223969915));
#46080=CARTESIAN_POINT('Ctrl Pts',(24.5638221088864,-0.505048782495192,
13.5899960272459));
#46081=CARTESIAN_POINT('Ctrl Pts',(24.4060199700213,2.72774157840345,12.387916003312));
#46082=CARTESIAN_POINT('Ctrl Pts',(24.2482178311564,3.49161491002287,9.0245357108578));
#46083=CARTESIAN_POINT('Ctrl Pts',(24.0904156922914,1.09510149634942,6.54403898763965));
#46084=CARTESIAN_POINT('Ctrl Pts',(23.9326135534264,-2.29260925396287,7.19165511461472));
#46085=CARTESIAN_POINT('Ctrl Pts',(23.7748114145613,-3.60521723307181,10.3811773897178));
#46086=CARTESIAN_POINT('Ctrl Pts',(23.6170092756964,-1.65463280838614,13.2256900191163));
#46087=CARTESIAN_POINT('Ctrl Pts',(23.4592071368313,1.79360733424122,13.1505319563297));
#46088=CARTESIAN_POINT('Ctrl Pts',(23.3014049979663,3.61840100535183,10.2237352102483));
#46089=CARTESIAN_POINT('Ctrl Pts',(23.1436028591013,2.16807193309428,7.09442832744505));
#46090=CARTESIAN_POINT('Ctrl Pts',(22.9858007202363,-1.24464326464773,6.59504112130271));
#46091=CARTESIAN_POINT('Ctrl Pts',(22.8279985813713,-3.53079496446001,9.17758320677621));
#46092=CARTESIAN_POINT('Ctrl Pts',(22.6701964425063,-2.62111912833757,12.5045192826475));
#46093=CARTESIAN_POINT('Ctrl Pts',(22.5123943036413,0.661009511544134,13.5645404549472));
#46094=CARTESIAN_POINT('Ctrl Pts',(22.3545921647763,3.34483881058325,11.3981901341401));
#46095=CARTESIAN_POINT('Ctrl Pts',(22.1967900259113,3.0011550686756,7.96629634724844));
#46096=CARTESIAN_POINT('Ctrl Pts',(22.0389878870462,-0.0589633304184637,
6.37516819565949));
#46097=CARTESIAN_POINT('Ctrl Pts',(21.8811857481813,-3.06571226878003,8.06498305391951));
#46098=CARTESIAN_POINT('Ctrl Pts',(21.7233836093162,-3.29759390354424,11.5062392702711));
#46099=CARTESIAN_POINT('Ctrl Pts',(21.5655814704513,-0.544725276252224,
13.5841535492561));
#46100=CARTESIAN_POINT('Ctrl Pts',(21.4077793315862,2.70119039079158,12.4179439128307));
#46101=CARTESIAN_POINT('Ctrl Pts',(21.2499771927212,3.50217834240436,9.06318136752485));
#46102=CARTESIAN_POINT('Ctrl Pts',(21.0921750538562,1.13324057456603,6.55636121344182));
#46103=CARTESIAN_POINT('Ctrl Pts',(20.9343729149912,-2.26142692279634,7.16648088674201));
#46104=CARTESIAN_POINT('Ctrl Pts',(20.7765707761262,-3.60920969167029,10.3413029355054));
#46105=CARTESIAN_POINT('Ctrl Pts',(20.6187686372612,-1.69018948530375,13.2072015521334));
#46106=CARTESIAN_POINT('Ctrl Pts',(20.4609664983962,1.75867146489572,13.1701667102578));
#46107=CARTESIAN_POINT('Ctrl Pts',(20.3031643595312,3.61570659591804,10.2637197460999));
#46108=CARTESIAN_POINT('Ctrl Pts',(20.1453622206662,2.20005821053506,7.11857220071228));
#46109=CARTESIAN_POINT('Ctrl Pts',(19.9875600818011,-1.20692825766852,6.58149060655154));
#46110=CARTESIAN_POINT('Ctrl Pts',(19.8297579429362,-3.52148808405926,9.13860347918041));
#46111=CARTESIAN_POINT('Ctrl Pts',(19.6719558040711,-2.64864436976049,12.4753919477101));
#46112=CARTESIAN_POINT('Ctrl Pts',(19.5141536652062,0.621566094242422,13.5716295836412));
#46113=CARTESIAN_POINT('Ctrl Pts',(19.3563515263411,3.32917861036942,11.4350791171607));
#46114=CARTESIAN_POINT('Ctrl Pts',(19.1985493874761,3.02345260681924,7.99959588418488));
#46115=CARTESIAN_POINT('Ctrl Pts',(19.0407472486111,-0.0188902229263912,
6.37473787820383));
#46116=CARTESIAN_POINT('Ctrl Pts',(18.8829451097461,-3.04413495039173,8.03121237913899));
#46117=CARTESIAN_POINT('Ctrl Pts',(18.7251429708811,-3.31404264771403,11.4696950776895));
#46118=CARTESIAN_POINT('Ctrl Pts',(18.5673408320161,-0.584311835073177,
13.5779130749147));
#46119=CARTESIAN_POINT('Ctrl Pts',(18.4095386931511,2.6742969880911,12.4476555950008));
#46120=CARTESIAN_POINT('Ctrl Pts',(18.2517365542861,3.51232011417934,9.10195227978501));
#46121=CARTESIAN_POINT('Ctrl Pts',(18.0939344154211,1.17123790163294,6.56909865049566));
#46122=CARTESIAN_POINT('Ctrl Pts',(17.9361322765561,-2.22996655058651,7.14165581577071));
#46123=CARTESIAN_POINT('Ctrl Pts',(17.7783301376911,-3.6127619923839,10.3013852661271));
#46124=CARTESIAN_POINT('Ctrl Pts',(17.6205279988261,-1.72553916596101,13.1883219534713));
#46125=CARTESIAN_POINT('Ctrl Pts',(17.462725859961,1.72352045101636,13.1894136682438));
#46126=CARTESIAN_POINT('Ctrl Pts',(17.3049237210961,3.61257047634171,10.3036722669531));
#46127=CARTESIAN_POINT('Ctrl Pts',(17.147121582231,2.23177558030935,7.14306807022165));
#46128=CARTESIAN_POINT('Ctrl Pts',(16.989319443366,-1.1690657327204,6.56835788508897));
#46129=CARTESIAN_POINT('Ctrl Pts',(16.831517304501,-3.5117509007273,9.09972898330938));
#46130=CARTESIAN_POINT('Ctrl Pts',(16.673715165636,-2.67584594211482,12.4459621391836));
#46131=CARTESIAN_POINT('Ctrl Pts',(16.515913026771,0.582046717903019,13.5782822569538));
#46132=CARTESIAN_POINT('Ctrl Pts',(16.358110887906,3.3131115922785,11.4717927399475));
#46133=CARTESIAN_POINT('Ctrl Pts',(16.200308749041,3.04538068264102,8.03313986515331));
#46134=CARTESIAN_POINT('Ctrl Pts',(16.042506610176,0.0211851935724078,6.37475056308874));
#46135=CARTESIAN_POINT('Ctrl Pts',(15.884704471311,-3.02218564392591,7.99768228647392));
#46136=CARTESIAN_POINT('Ctrl Pts',(15.7269023324459,-3.33008642100386,11.4329712910236));
#46137=CARTESIAN_POINT('Ctrl Pts',(15.569100193581,-0.623826992014808,13.5712353851694));
#46138=CARTESIAN_POINT('Ctrl Pts',(15.4112980547159,2.6470767906288,12.4770681776581));
#46139=CARTESIAN_POINT('Ctrl Pts',(15.2534959158509,3.52203268603658,9.14083293199628));
#46140=CARTESIAN_POINT('Ctrl Pts',(15.0956937769859,1.20909210531671,6.58225533822185));
#46141=CARTESIAN_POINT('Ctrl Pts',(14.9378916381209,-2.19823368004202,7.11718002986987));
#46142=CARTESIAN_POINT('Ctrl Pts',(14.7800894992559,-3.61587281936424,10.2614307679579));
#46143=CARTESIAN_POINT('Ctrl Pts',(14.6222873603909,-1.76067798849733,13.1690527469692));
#46144=CARTESIAN_POINT('Ctrl Pts',(14.4644852215259,1.68815882569895,13.2082708849888));
#46145=CARTESIAN_POINT('Ctrl Pts',(14.3066830826609,3.60899290643803,10.3435876795407));
#46146=CARTESIAN_POINT('Ctrl Pts',(14.1488809437959,2.26322023068206,7.16791305223806));
#46147=CARTESIAN_POINT('Ctrl Pts',(13.9910788049309,-1.13106034981207,6.55564450479696));
#46148=CARTESIAN_POINT('Ctrl Pts',(13.8332766660659,-3.50158458705909,9.06096449911507));
#46149=CARTESIAN_POINT('Ctrl Pts',(13.6754745272009,-2.70272053038027,12.4162334380006));
#46150=CARTESIAN_POINT('Ctrl Pts',(13.5176723883359,0.542456216386849,13.5844976699054));
#46151=CARTESIAN_POINT('Ctrl Pts',(13.3598702494708,3.2966397172568,11.5083265120178));
#46152=CARTESIAN_POINT('Ctrl Pts',(13.2020681106059,3.06693661782036,8.06692419328139));
#46153=CARTESIAN_POINT('Ctrl Pts',(13.0442659717408,0.0612580212745303,
6.37520624764731));
#46154=CARTESIAN_POINT('Ctrl Pts',(12.8864638328758,-2.99986703121441,7.96439687383041));
#46155=CARTESIAN_POINT('Ctrl Pts',(12.7286616940108,-3.34572326306573,11.396072397554));
#46156=CARTESIAN_POINT('Ctrl Pts',(12.5708595551458,-0.663265918297566,
13.5641212961923));
#46157=CARTESIAN_POINT('Ctrl Pts',(12.4130574162808,2.61953312462283,12.5061780665257));
#46158=CARTESIAN_POINT('Ctrl Pts',(12.2552552774158,3.53131487113802,9.17981857309606));
#46159=CARTESIAN_POINT('Ctrl Pts',(12.0974531385508,1.2467985598852,6.59582966877859));
#46160=CARTESIAN_POINT('Ctrl Pts',(11.9396509996858,-2.1662321888693,7.09305652013331));
#46161=CARTESIAN_POINT('Ctrl Pts',(11.7818488608208,-3.61854179246299,10.2214443230196));
#46162=CARTESIAN_POINT('Ctrl Pts',(11.6240467219557,-1.7956016590295,13.1493962879665));
#46163=CARTESIAN_POINT('Ctrl Pts',(11.4662445830908,1.65259091012735,13.2267360548792));
#46164=CARTESIAN_POINT('Ctrl Pts',(11.3084424442257,3.60497432328288,10.3834611087496));
#46165=CARTESIAN_POINT('Ctrl Pts',(11.1506403053608,2.29438831935563,7.19310410595708));
#46166=CARTESIAN_POINT('Ctrl Pts',(10.9928381664957,-1.09291675350356,6.5433520284504));
#46167=CARTESIAN_POINT('Ctrl Pts',(10.8350360276307,-3.49099038466235,9.02231474579732));
#46168=CARTESIAN_POINT('Ctrl Pts',(10.6772338887657,-2.72926485187264,12.3862095111631));
#46169=CARTESIAN_POINT('Ctrl Pts',(10.5194317499007,0.502799430185017,13.5902749971079));
#46170=CARTESIAN_POINT('Ctrl Pts',(10.3616296110357,3.27976499314249,11.5446760958796));
#46171=CARTESIAN_POINT('Ctrl Pts',(10.2038274721707,3.08811778788391,8.10094449581088));
#46172=CARTESIAN_POINT('Ctrl Pts',(10.0460253333057,0.101323344801963,6.37610534685446));
#46173=CARTESIAN_POINT('Ctrl Pts',(9.88822319444067,-2.97718180384226,7.93135930212979));
#46174=CARTESIAN_POINT('Ctrl Pts',(9.73042105557568,-3.36095133188827,11.3590046522174));
#46175=CARTESIAN_POINT('Ctrl Pts',(9.57261891671066,-0.702623662064588,
13.5565683145601));
#46176=CARTESIAN_POINT('Ctrl Pts',(9.41481677784566,2.59166910069841,12.5349881811848));
#46177=CARTESIAN_POINT('Ctrl Pts',(9.25701463898065,3.54016602667422,9.21889196466343));
#46178=CARTESIAN_POINT('Ctrl Pts',(9.09921250011564,1.28435171110455,6.60984400954655));
#46179=CARTESIAN_POINT('Ctrl Pts',(8.94141036125063,-2.13396416447173,7.0692419593061));
#46180=CARTESIAN_POINT('Ctrl Pts',(8.78360822238564,-3.62077209706865,10.1815199452736));
#46181=CARTESIAN_POINT('Ctrl Pts',(8.62580608352061,-1.83029914535168,13.1291833116438));
#46182=CARTESIAN_POINT('Ctrl Pts',(8.46800394465562,1.61680800983869,13.245137596954));
#46183=CARTESIAN_POINT('Ctrl Pts',(8.31020180579059,3.60054044813756,10.4226504132617));
#46184=CARTESIAN_POINT('Ctrl Pts',(8.15239966692561,2.32522637585507,7.21986911759536));
#46185=CARTESIAN_POINT('Ctrl Pts',(7.99459752806058,-1.05453388826692,6.52907745913553));
#46186=CARTESIAN_POINT('Ctrl Pts',(7.83679538919558,-3.48026767237864,8.9887322426102));
#46187=CARTESIAN_POINT('Ctrl Pts',(7.73159396328557,-2.99617087576157,11.2252327859881));
#46188=CARTESIAN_POINT('Ctrl Pts',(7.67899325033057,-2.33606265769622,11.9973015569306));
#46189=CARTESIAN_POINT('Ctrl Pts',(25.9332414696963,-2.81993930255816,9.37594148965641));
#46190=CARTESIAN_POINT('Ctrl Pts',(25.8806407567413,-3.02619065694277,10.3079315046869));
#46191=CARTESIAN_POINT('Ctrl Pts',(25.7754393308313,-2.43933177044069,12.3766075622725));
#46192=CARTESIAN_POINT('Ctrl Pts',(25.6176371919662,0.659289653036446,13.3444735591669));
#46193=CARTESIAN_POINT('Ctrl Pts',(25.4598350531013,3.15689027586569,11.2780546690366));
#46194=CARTESIAN_POINT('Ctrl Pts',(25.3020329142362,2.79918909152747,8.05838883695592));
#46195=CARTESIAN_POINT('Ctrl Pts',(25.1442307753712,-0.0932146705834936,
6.59429920647375));
#46196=CARTESIAN_POINT('Ctrl Pts',(24.9864286365063,-2.90069123054593,8.21376124529306));
#46197=CARTESIAN_POINT('Ctrl Pts',(24.8286264976412,-3.08295437234279,11.449507652376));
#46198=CARTESIAN_POINT('Ctrl Pts',(24.6708243587762,-0.474594130028695,
13.3735177678079));
#46199=CARTESIAN_POINT('Ctrl Pts',(24.5130222199112,2.56325762226307,12.2439236712431));
#46200=CARTESIAN_POINT('Ctrl Pts',(24.3552200810462,3.28106907303217,9.0833566147961));
#46201=CARTESIAN_POINT('Ctrl Pts',(24.1974179421812,1.02906641886227,6.75243487971409));
#46202=CARTESIAN_POINT('Ctrl Pts',(24.0396158033162,-2.15436395867484,7.36099948382184));
#46203=CARTESIAN_POINT('Ctrl Pts',(23.8818136644512,-3.38782112856686,10.3581922339581));
#46204=CARTESIAN_POINT('Ctrl Pts',(23.7240115255861,-1.55485775915207,13.0311795640836));
#46205=CARTESIAN_POINT('Ctrl Pts',(23.5662093867212,1.68545206306958,12.9605535638652));
#46206=CARTESIAN_POINT('Ctrl Pts',(23.4084072478561,3.40020991387353,10.2102438836502));
#46207=CARTESIAN_POINT('Ctrl Pts',(23.2506051089912,2.03733629025491,7.26963551251533));
#46208=CARTESIAN_POINT('Ctrl Pts',(23.0928029701261,-1.16959075609135,6.80036156342144));
#46209=CARTESIAN_POINT('Ctrl Pts',(22.9350008312611,-3.31788655382721,9.22717528280597));
#46210=CARTESIAN_POINT('Ctrl Pts',(22.7771986923961,-2.46306455045614,12.3534957241472));
#46211=CARTESIAN_POINT('Ctrl Pts',(22.6193965535311,0.621150361994919,13.3495971771476));
#46212=CARTESIAN_POINT('Ctrl Pts',(22.4615944146661,3.1431436336748,11.3138786852401));
#46213=CARTESIAN_POINT('Ctrl Pts',(22.3037922758011,2.8201841649086,8.08892952667795));
#46214=CARTESIAN_POINT('Ctrl Pts',(22.1459901369361,-0.0554078169742211,
6.59374706700197));
#46215=CARTESIAN_POINT('Ctrl Pts',(21.988187998071,-2.88084853889101,8.18166538373033));
#46216=CARTESIAN_POINT('Ctrl Pts',(21.8303858592061,-3.09874761425726,11.4154124133468));
#46217=CARTESIAN_POINT('Ctrl Pts',(21.672583720341,-0.511878114645344,13.3680275936803));
#46218=CARTESIAN_POINT('Ctrl Pts',(21.5147815814761,2.5383074823506,12.2721408852797));
#46219=CARTESIAN_POINT('Ctrl Pts',(21.356979442611,3.29099552603032,9.11967192222973));
#46220=CARTESIAN_POINT('Ctrl Pts',(21.199177303746,1.06490569473753,6.76401407015525));
#46221=CARTESIAN_POINT('Ctrl Pts',(21.041375164881,-2.12506193509776,7.3373432724013));
#46222=CARTESIAN_POINT('Ctrl Pts',(20.883573026016,-3.39157284024481,10.3207222259841));
#46223=CARTESIAN_POINT('Ctrl Pts',(20.725770887151,-1.58827035360494,13.0138059593797));
#46224=CARTESIAN_POINT('Ctrl Pts',(20.567968748286,1.65262284123301,12.979004333933));
#46225=CARTESIAN_POINT('Ctrl Pts',(20.410166609421,3.39767797845365,10.2478173352944));
#46226=CARTESIAN_POINT('Ctrl Pts',(20.252364470556,2.0673937818102,7.29232350014334));
#46227=CARTESIAN_POINT('Ctrl Pts',(20.094562331691,-1.1341499797808,6.78762815036774));
#46228=CARTESIAN_POINT('Ctrl Pts',(19.936760192826,-3.30914088220069,9.1905460490601));
#46229=CARTESIAN_POINT('Ctrl Pts',(19.778958053961,-2.48893000832816,12.3261247796686));
#46230=CARTESIAN_POINT('Ctrl Pts',(19.621155915096,0.584085399226014,13.3562588284213));
#46231=CARTESIAN_POINT('Ctrl Pts',(19.4633537762309,3.12842775007275,11.3485432471817));
#46232=CARTESIAN_POINT('Ctrl Pts',(19.305551637366,2.84113715219189,8.12022108763298));
#46233=CARTESIAN_POINT('Ctrl Pts',(19.1477494985009,-0.0177511345963581,
6.59334269786856));
#46234=CARTESIAN_POINT('Ctrl Pts',(18.9899473596359,-2.86057234181109,8.14993109473996));
#46235=CARTESIAN_POINT('Ctrl Pts',(18.8321452207709,-3.11420449228548,11.3810718508368));
#46236=CARTESIAN_POINT('Ctrl Pts',(18.6743430819059,-0.549077587440111,
13.3621634225474));
#46237=CARTESIAN_POINT('Ctrl Pts',(18.5165409430409,2.51303576306224,12.300060940609));
#46238=CARTESIAN_POINT('Ctrl Pts',(18.3587388041759,3.3005257447326,9.15610493229186));
#46239=CARTESIAN_POINT('Ctrl Pts',(18.2009366653109,1.1006117671166,6.77598343443628));
#46240=CARTESIAN_POINT('Ctrl Pts',(18.0431345264459,-2.09549863646839,7.31401516357522));
#46241=CARTESIAN_POINT('Ctrl Pts',(17.8853323875809,-3.39491093574213,10.2832116087369));
#46242=CARTESIAN_POINT('Ctrl Pts',(17.7275302487159,-1.62148843375838,12.9960648084));
#46243=CARTESIAN_POINT('Ctrl Pts',(17.5697281098509,1.61959144816781,12.9970906923159));
#46244=CARTESIAN_POINT('Ctrl Pts',(17.4119259709859,3.39473096819725,10.2853607024581));
#46245=CARTESIAN_POINT('Ctrl Pts',(17.2541238321208,2.09719858094359,7.31534225849308));
#46246=CARTESIAN_POINT('Ctrl Pts',(17.0963216932558,-1.09857058089647,6.7752873374929));
#46247=CARTESIAN_POINT('Ctrl Pts',(16.9385195543908,-3.29999085508938,9.15401570152206));
#46248=CARTESIAN_POINT('Ctrl Pts',(16.7807174155258,-2.51449131451156,12.2984696008846));
#46249=CARTESIAN_POINT('Ctrl Pts',(16.6229152766608,0.546949057781108,13.3625103427554));
#46250=CARTESIAN_POINT('Ctrl Pts',(16.4651131377958,3.11332957988147,11.3830430231847));
#46251=CARTESIAN_POINT('Ctrl Pts',(16.3073109989308,2.86174295588559,8.1517423525428));
#46252=CARTESIAN_POINT('Ctrl Pts',(16.1495088600658,0.0199077175541609,
6.59335461784961));
#46253=CARTESIAN_POINT('Ctrl Pts',(15.9917067212008,-2.83994658769004,8.118422880663));
#46254=CARTESIAN_POINT('Ctrl Pts',(15.8339045823358,-3.12928081934688,11.3465625238408));
#46255=CARTESIAN_POINT('Ctrl Pts',(15.6761024434708,-0.586209963918693,
13.355888400282));
#46256=CARTESIAN_POINT('Ctrl Pts',(15.5183003046057,2.48745695487264,12.3276999322508));
#46257=CARTESIAN_POINT('Ctrl Pts',(15.3604981657408,3.30965264445138,9.19264106494028));
#46258=CARTESIAN_POINT('Ctrl Pts',(15.2026960268757,1.1361833465123,6.78834676839902));
#46259=CARTESIAN_POINT('Ctrl Pts',(15.0448938880107,-2.06567927126773,7.29101527778403));
#46260=CARTESIAN_POINT('Ctrl Pts',(14.8870917491457,-3.39783417855664,10.2456663834901));
#46261=CARTESIAN_POINT('Ctrl Pts',(14.7292896102807,-1.65450837062362,12.9779575430958));
#46262=CARTESIAN_POINT('Ctrl Pts',(14.5714874714157,1.58636214362221,13.0148108110173));
#46263=CARTESIAN_POINT('Ctrl Pts',(14.4136853325507,3.39136912725257,10.3228691990001));
#46264=CARTESIAN_POINT('Ctrl Pts',(14.2558831936857,2.12674710576918,7.33868907771994));
#46265=CARTESIAN_POINT('Ctrl Pts',(14.0980810548207,-1.06285693844658,6.76334057934094));
#46266=CARTESIAN_POINT('Ctrl Pts',(13.9402789159557,-3.2904375743803,9.11758873191071));
#46267=CARTESIAN_POINT('Ctrl Pts',(13.7824767770907,-2.53974535388318,12.2705335527961));
#46268=CARTESIAN_POINT('Ctrl Pts',(13.6246746382257,0.509745880037291,13.3683509637108));
#46269=CARTESIAN_POINT('Ctrl Pts',(13.4668724993607,3.09785096580137,11.4173737935446));
#46270=CARTESIAN_POINT('Ctrl Pts',(13.3090703604957,2.88199905917298,8.18348947157818));
#46271=CARTESIAN_POINT('Ctrl Pts',(13.1512682216306,0.0575641370135216,
6.59378282443903));
#46272=CARTESIAN_POINT('Ctrl Pts',(12.9934660827657,-2.81897379664414,8.08714459230016));
#46273=CARTESIAN_POINT('Ctrl Pts',(12.8356639439006,-3.1439747533033,11.3118886490544));
#46274=CARTESIAN_POINT('Ctrl Pts',(12.6778618050356,-0.623270706478959,
13.3492032938407));
#46275=CARTESIAN_POINT('Ctrl Pts',(12.5200596661706,2.46157418342764,12.3550544826649));
#46276=CARTESIAN_POINT('Ctrl Pts',(12.3622575273056,3.31837510991545,9.22927585560335));
#46277=CARTESIAN_POINT('Ctrl Pts',(12.2044553884406,1.17161608612606,6.80110256115527));
#46278=CARTESIAN_POINT('Ctrl Pts',(12.0466532495756,-2.03560748337488,7.26834642575728));
#46279=CARTESIAN_POINT('Ctrl Pts',(11.8888511107106,-3.40034221146311,10.2080911378779));
#46280=CARTESIAN_POINT('Ctrl Pts',(11.7310489718456,-1.6873261292404,12.9594863767785));
#46281=CARTESIAN_POINT('Ctrl Pts',(11.5732468329806,1.55293898821088,13.0321625234532));
#46282=CARTESIAN_POINT('Ctrl Pts',(11.4154446941155,3.38759286633963,10.3603382437786));
#46283=CARTESIAN_POINT('Ctrl Pts',(11.2576425552506,2.15603574568156,7.36236110038124));
#46284=CARTESIAN_POINT('Ctrl Pts',(11.0998404163855,-1.02701341692224,6.75178934445078));
#46285=CARTESIAN_POINT('Ctrl Pts',(10.9420382775205,-3.28048220681167,9.08126957485612));
#46286=CARTESIAN_POINT('Ctrl Pts',(10.7842361386555,-2.56468904170603,12.2423200812833));
#46287=CARTESIAN_POINT('Ctrl Pts',(10.6264339997905,0.472480414602034,13.3737799156707));
#46288=CARTESIAN_POINT('Ctrl Pts',(10.4686318609255,3.08199379459717,11.4515314823219));
#46289=CARTESIAN_POINT('Ctrl Pts',(10.3108297220605,2.90190299583755,8.21545833566004));
#46290=CARTESIAN_POINT('Ctrl Pts',(10.1530275831955,0.0952135048030617,
6.59462770758856));
#46291=CARTESIAN_POINT('Ctrl Pts',(9.99522544433049,-2.79765649795469,8.05609919996786));
#46292=CARTESIAN_POINT('Ctrl Pts',(9.83742330546549,-3.15828456321738,11.2770561042392));
#46293=CARTESIAN_POINT('Ctrl Pts',(9.67962116660047,-0.660255161863091,
13.3421057601546));
#46294=CARTESIAN_POINT('Ctrl Pts',(9.52181902773547,2.43539037178042,12.3821273353805));
#46295=CARTESIAN_POINT('Ctrl Pts',(9.36401688887045,3.32669253707703,9.26599310534422));
#46296=CARTESIAN_POINT('Ctrl Pts',(9.20621475000546,1.20690476664664,6.81427183132325));
#46297=CARTESIAN_POINT('Ctrl Pts',(9.04841261114043,-2.00528523432192,7.24596789289169));
#46298=CARTESIAN_POINT('Ctrl Pts',(8.89061047227545,-3.40243802776979,10.1705742167804));
#46299=CARTESIAN_POINT('Ctrl Pts',(8.73280833341042,-1.71993134264949,12.940492251368));
#46300=CARTESIAN_POINT('Ctrl Pts',(8.57500619454543,1.5193138117507,13.0494544448574));
#46301=CARTESIAN_POINT('Ctrl Pts',(8.41720405568041,3.38342635571692,10.3971644168652));
#46302=CARTESIAN_POINT('Ctrl Pts',(8.25940191681541,2.18501425449772,7.38751217064205));
#46303=CARTESIAN_POINT('Ctrl Pts',(8.10159977795039,-0.990945054486066,
6.73837553762593));
#46304=CARTESIAN_POINT('Ctrl Pts',(7.94379763908539,-3.27040607855591,9.04971211063347));
#46305=CARTESIAN_POINT('Ctrl Pts',(7.83859621317538,-2.81550052090843,11.1513507373997));
#46306=CARTESIAN_POINT('Ctrl Pts',(7.78599550022038,-2.19519710401918,11.8768634390787));
#46307=CARTESIAN_POINT('Ctrl Pts',(26.0402437195861,-2.63898411158091,9.41598725476127));
#46308=CARTESIAN_POINT('Ctrl Pts',(25.9876430066311,-2.8320003395257,10.2881715743267));
#46309=CARTESIAN_POINT('Ctrl Pts',(25.8824415807211,-2.28280012240964,12.2241009196938));
#46310=CARTESIAN_POINT('Ctrl Pts',(25.724639441856,0.61698310942882,13.1298590633625));
#46311=CARTESIAN_POINT('Ctrl Pts',(25.5668373029911,2.95431297845888,11.1960420432666));
#46312=CARTESIAN_POINT('Ctrl Pts',(25.409035164126,2.61956543928103,8.18298180904346));
#46313=CARTESIAN_POINT('Ctrl Pts',(25.251233025261,-0.0872330955538401,
6.81284264708782));
#46314=CARTESIAN_POINT('Ctrl Pts',(25.093430886396,-2.71455419734337,8.32838398724206));
#46315=CARTESIAN_POINT('Ctrl Pts',(24.935628747531,-2.88512153363051,11.3564929077605));
#46316=CARTESIAN_POINT('Ctrl Pts',(24.777826608666,-0.4441394775622,13.1570395083698));
#46317=CARTESIAN_POINT('Ctrl Pts',(24.620024469801,2.3987736661227,12.0999313391742));
#46318=CARTESIAN_POINT('Ctrl Pts',(24.462222330936,3.07052323604148,9.14217751873442));
#46319=CARTESIAN_POINT('Ctrl Pts',(24.304420192071,0.963031341375119,6.96083077178851));
#46320=CARTESIAN_POINT('Ctrl Pts',(24.146618053206,-2.0161186633868,7.53034385302897));
#46321=CARTESIAN_POINT('Ctrl Pts',(23.988815914341,-3.1704250240619,10.3352070781982));
#46322=CARTESIAN_POINT('Ctrl Pts',(23.8310137754759,-1.45508270991801,12.836669109051));
#46323=CARTESIAN_POINT('Ctrl Pts',(23.673211636611,1.57729679189794,12.7705751714006));
#46324=CARTESIAN_POINT('Ctrl Pts',(23.5154094977459,3.18201882239524,10.1967525570521));
#46325=CARTESIAN_POINT('Ctrl Pts',(23.357607358881,1.90660064741554,7.44484269758562));
#46326=CARTESIAN_POINT('Ctrl Pts',(23.1998052200159,-1.09453824753496,7.00568200554017));
#46327=CARTESIAN_POINT('Ctrl Pts',(23.0420030811509,-3.10497814319441,9.27676735883572));
#46328=CARTESIAN_POINT('Ctrl Pts',(22.8842009422859,-2.30500997257471,12.2024721656469));
#46329=CARTESIAN_POINT('Ctrl Pts',(22.7263988034209,0.581291212445702,13.1346538993481));
#46330=CARTESIAN_POINT('Ctrl Pts',(22.5685966645559,2.94144845676636,11.2295672363402));
#46331=CARTESIAN_POINT('Ctrl Pts',(22.4107945256909,2.63921326114159,8.21156270610747));
#46332=CARTESIAN_POINT('Ctrl Pts',(22.2529923868259,-0.0518523035299743,
6.81232593834445));
#46333=CARTESIAN_POINT('Ctrl Pts',(22.0951902479609,-2.69598480900199,8.29834771354115));
#46334=CARTESIAN_POINT('Ctrl Pts',(21.9373881090959,-2.89990132497028,11.3245855564225));
#46335=CARTESIAN_POINT('Ctrl Pts',(21.7795859702309,-0.479030953038463,
13.1519016381045));
#46336=CARTESIAN_POINT('Ctrl Pts',(21.6217838313659,2.37542457390961,12.1263378577287));
#46337=CARTESIAN_POINT('Ctrl Pts',(21.4639816925008,3.07981270965628,9.17616247693458));
#46338=CARTESIAN_POINT('Ctrl Pts',(21.3061795536359,0.996570814909022,6.97166692686871));
#46339=CARTESIAN_POINT('Ctrl Pts',(21.1483774147708,-1.98869694739918,7.50820565806059));
#46340=CARTESIAN_POINT('Ctrl Pts',(20.9905752759058,-3.17393598881932,10.3001415164628));
#46341=CARTESIAN_POINT('Ctrl Pts',(20.8327731370408,-1.48635122190613,12.8204103666259));
#46342=CARTESIAN_POINT('Ctrl Pts',(20.6749709981758,1.5465742175703,12.7878419576081));
#46343=CARTESIAN_POINT('Ctrl Pts',(20.5171688593108,3.17964936098926,10.231914924489));
#46344=CARTESIAN_POINT('Ctrl Pts',(20.3593667204458,1.93472935308535,7.46607479957437));
#46345=CARTESIAN_POINT('Ctrl Pts',(20.2015645815808,-1.06137170189308,6.99376569418397));
#46346=CARTESIAN_POINT('Ctrl Pts',(20.0437624427158,-3.09679368034212,9.24248861893978));
#46347=CARTESIAN_POINT('Ctrl Pts',(19.8859603038508,-2.32921564689582,12.1768576116271));
#46348=CARTESIAN_POINT('Ctrl Pts',(19.7281581649858,0.546604704209606,13.1408880732015));
#46349=CARTESIAN_POINT('Ctrl Pts',(19.5703560261207,2.92767688977609,11.2620073772027));
#46350=CARTESIAN_POINT('Ctrl Pts',(19.4125538872558,2.65882169756453,8.24084629108108));
#46351=CARTESIAN_POINT('Ctrl Pts',(19.2547517483908,-0.0166120462663256,
6.8119475175333));
#46352=CARTESIAN_POINT('Ctrl Pts',(19.0969496095257,-2.67700973323045,8.26864981034091));
#46353=CARTESIAN_POINT('Ctrl Pts',(18.9391474706607,-2.91436633685692,11.2924486239841));
#46354=CARTESIAN_POINT('Ctrl Pts',(18.7813453317957,-0.513843339807043,
13.1464137701801));
#46355=CARTESIAN_POINT('Ctrl Pts',(18.6235431929307,2.35177453803337,12.1524662862171));
#46356=CARTESIAN_POINT('Ctrl Pts',(18.4657410540657,3.08873137528585,9.21025758479872));
#46357=CARTESIAN_POINT('Ctrl Pts',(18.3079389152007,1.02998563260026,6.9828682183769));
#46358=CARTESIAN_POINT('Ctrl Pts',(18.1501367763357,-1.96103072235028,7.48637451137971));
#46359=CARTESIAN_POINT('Ctrl Pts',(17.9923346374707,-3.17705987910036,10.2650379513466));
#46360=CARTESIAN_POINT('Ctrl Pts',(17.8345324986057,-1.51743770155576,12.8038076633286));
#46361=CARTESIAN_POINT('Ctrl Pts',(17.6767303597407,1.51566244531925,12.8047677163879));
#46362=CARTESIAN_POINT('Ctrl Pts',(17.5189282208757,3.17689146005279,10.2670491379631));
#46363=CARTESIAN_POINT('Ctrl Pts',(17.3611260820106,1.96262158157783,7.48761644676452));
#46364=CARTESIAN_POINT('Ctrl Pts',(17.2033239431456,-1.02807542907254,6.98221678989685));
#46365=CARTESIAN_POINT('Ctrl Pts',(17.0455218042806,-3.08823080945147,9.20830241973473));
#46366=CARTESIAN_POINT('Ctrl Pts',(16.8877196654156,-2.3531366869083,12.1509770625856));
#46367=CARTESIAN_POINT('Ctrl Pts',(16.7299175265506,0.511851397659197,13.146738428557));
#46368=CARTESIAN_POINT('Ctrl Pts',(16.5721153876856,2.91354756748443,11.294293306422));
#46369=CARTESIAN_POINT('Ctrl Pts',(16.4143132488206,2.67810522913017,8.2703448399323));
#46370=CARTESIAN_POINT('Ctrl Pts',(16.2565111099556,0.0186302415359106,
6.81195867261049));
#46371=CARTESIAN_POINT('Ctrl Pts',(16.0987089710906,-2.65770753145417,8.23916347485209));
#46372=CARTESIAN_POINT('Ctrl Pts',(15.9409068322256,-2.92847521768991,11.260153756658));
#46373=CARTESIAN_POINT('Ctrl Pts',(15.7831046933606,-0.548592935822577,
13.1405414153946));
#46374=CARTESIAN_POINT('Ctrl Pts',(15.6253025544956,2.32783711911649,12.1783316868435));
#46375=CARTESIAN_POINT('Ctrl Pts',(15.4675004156306,3.09727260286618,9.24444919788427));
#46376=CARTESIAN_POINT('Ctrl Pts',(15.3096982767655,1.06327458770789,6.9944381985762));
#46377=CARTESIAN_POINT('Ctrl Pts',(15.1518961379006,-1.93312486249343,7.46485052569816));
#46378=CARTESIAN_POINT('Ctrl Pts',(14.9940939990355,-3.17979553774904,10.2299019990224));
#46379=CARTESIAN_POINT('Ctrl Pts',(14.8362918601705,-1.54833875274991,12.7868623392224));
#46380=CARTESIAN_POINT('Ctrl Pts',(14.6784897213055,1.48456546154546,12.8213507370459));
#46381=CARTESIAN_POINT('Ctrl Pts',(14.5206875824405,3.17374534806711,10.3021507184595));
#46382=CARTESIAN_POINT('Ctrl Pts',(14.3628854435755,1.9902739808563,7.50946510320182));
#46383=CARTESIAN_POINT('Ctrl Pts',(14.2050833047105,-0.994653527081089,
6.97103665388494));
#46384=CARTESIAN_POINT('Ctrl Pts',(14.0472811658455,-3.0792905617015,9.17421296470632));
#46385=CARTESIAN_POINT('Ctrl Pts',(13.8894790269805,-2.37677017738608,12.1248336675916));
#46386=CARTESIAN_POINT('Ctrl Pts',(13.7316768881155,0.477035543687735,13.1522042575162));
#46387=CARTESIAN_POINT('Ctrl Pts',(13.5738747492505,2.89906221434594,11.3264210750714));
#46388=CARTESIAN_POINT('Ctrl Pts',(13.4160726103855,2.69706150052561,8.30005474987497));
#46389=CARTESIAN_POINT('Ctrl Pts',(13.2582704715205,0.0538702527525129,
6.81235940123075));
#46390=CARTESIAN_POINT('Ctrl Pts',(13.1004683326554,-2.63808056207387,8.20989231076991));
#46391=CARTESIAN_POINT('Ctrl Pts',(12.9426661937904,-2.94222624354086,11.2277049005549));
#46392=CARTESIAN_POINT('Ctrl Pts',(12.7848640549254,-0.583275494660355,
13.1342852914891));
#46393=CARTESIAN_POINT('Ctrl Pts',(12.6270619160604,2.30361524223244,12.2039308988041));
#46394=CARTESIAN_POINT('Ctrl Pts',(12.4692597771954,3.10543534869288,9.27873313811066));
#46395=CARTESIAN_POINT('Ctrl Pts',(12.3114576383304,1.09643361236692,7.00637545353194));
#46396=CARTESIAN_POINT('Ctrl Pts',(12.1536554994654,-1.90498277788045,7.44363633138125));
#46397=CARTESIAN_POINT('Ctrl Pts',(11.9958533606004,-3.18214263046322,10.1947379527362));
#46398=CARTESIAN_POINT('Ctrl Pts',(11.8380512217354,-1.5790505994513,12.7695764655905));
#46399=CARTESIAN_POINT('Ctrl Pts',(11.6802490828704,1.45328706629441,12.8375889920273));
#46400=CARTESIAN_POINT('Ctrl Pts',(11.5224469440054,3.17021140939637,10.3372153788076));
#46401=CARTESIAN_POINT('Ctrl Pts',(11.3646448051404,2.0176831720075,7.53161809480538));
#46402=CARTESIAN_POINT('Ctrl Pts',(11.2068426662754,-0.961110080340932,
6.96022666045117));
#46403=CARTESIAN_POINT('Ctrl Pts',(11.0490405274104,-3.06997402896098,9.14022440391494));
#46404=CARTESIAN_POINT('Ctrl Pts',(10.8912383885453,-2.40011323153943,12.0984306514035));
#46405=CARTESIAN_POINT('Ctrl Pts',(10.7334362496803,0.442161399019054,13.1572848342334));
#46406=CARTESIAN_POINT('Ctrl Pts',(10.5756341108153,2.88422259605183,11.3583868687642));
#46407=CARTESIAN_POINT('Ctrl Pts',(10.4178319719503,2.71568820379119,8.32997217550921));
#46408=CARTESIAN_POINT('Ctrl Pts',(10.2600298330853,0.0891036648041555,
6.81315006832269));
#46409=CARTESIAN_POINT('Ctrl Pts',(10.1022276942203,-2.61813119206713,8.1808390978059));
#46410=CARTESIAN_POINT('Ctrl Pts',(9.9444255553553,-2.9556177945465,11.195107556261));
#46411=CARTESIAN_POINT('Ctrl Pts',(9.78662341649027,-0.61788666166159,13.1276432057492));
#46412=CARTESIAN_POINT('Ctrl Pts',(9.62882127762529,2.27911164286243,12.2292664895762));
#46413=CARTESIAN_POINT('Ctrl Pts',(9.47101913876025,3.11321904747985,9.31309424602498));
#46414=CARTESIAN_POINT('Ctrl Pts',(9.31321699989528,1.12945782218873,7.01869965309997));
#46415=CARTESIAN_POINT('Ctrl Pts',(9.15541486103024,-1.87660630417212,7.42269382647725));
#46416=CARTESIAN_POINT('Ctrl Pts',(8.99761272216525,-3.18410395847092,10.1596284882871));
#46417=CARTESIAN_POINT('Ctrl Pts',(8.83981058330023,-1.6095635399473,12.7518011910921));
#46418=CARTESIAN_POINT('Ctrl Pts',(8.68200844443524,1.42181961366271,12.8537712927609));
#46419=CARTESIAN_POINT('Ctrl Pts',(8.52420630557022,3.16631226329628,10.3716784204688));
#46420=CARTESIAN_POINT('Ctrl Pts',(8.36640416670522,2.04480213314037,7.55515522368873));
#46421=CARTESIAN_POINT('Ctrl Pts',(8.20860202784021,-0.927356220705207,
6.94767361611631));
#46422=CARTESIAN_POINT('Ctrl Pts',(8.0507998889752,-3.06054448473317,9.11069197865678));
#46423=CARTESIAN_POINT('Ctrl Pts',(7.94559846306519,-2.63483016605528,11.0774686888113));
#46424=CARTESIAN_POINT('Ctrl Pts',(7.89299775011019,-2.05433155034215,11.7564253212268));
#46425=CARTESIAN_POINT('Ctrl Pts',(26.1472459694759,-2.45802892060367,9.45603301986612));
#46426=CARTESIAN_POINT('Ctrl Pts',(26.0946452565209,-2.63781002210864,10.2684116439665));
#46427=CARTESIAN_POINT('Ctrl Pts',(25.9894438306109,-2.12626847437859,12.071594277115));
#46428=CARTESIAN_POINT('Ctrl Pts',(25.8316416917459,0.574676565821197,12.9152445675582));
#46429=CARTESIAN_POINT('Ctrl Pts',(25.6738395528808,2.75173568105207,11.1140294174966));
#46430=CARTESIAN_POINT('Ctrl Pts',(25.5160374140159,2.43994178703459,8.307574781131));
#46431=CARTESIAN_POINT('Ctrl Pts',(25.3582352751508,-0.0812515205241886,
7.0313860877019));
#46432=CARTESIAN_POINT('Ctrl Pts',(25.2004331362858,-2.52841716414082,8.44300672919104));
#46433=CARTESIAN_POINT('Ctrl Pts',(25.0426309974208,-2.68728869491822,11.263478163145));
#46434=CARTESIAN_POINT('Ctrl Pts',(24.8848288585558,-0.413684825095704,
12.9405612489317));
#46435=CARTESIAN_POINT('Ctrl Pts',(24.7270267196908,2.23428970998233,11.9559390071053));
#46436=CARTESIAN_POINT('Ctrl Pts',(24.5692245808258,2.85997739905078,9.2009984226727));
#46437=CARTESIAN_POINT('Ctrl Pts',(24.4114224419608,0.896996263887967,7.16922666386296));
#46438=CARTESIAN_POINT('Ctrl Pts',(24.2536203030958,-1.87787336809876,7.69968822223608));
#46439=CARTESIAN_POINT('Ctrl Pts',(24.0958181642307,-2.95302891955695,10.3122219224385));
#46440=CARTESIAN_POINT('Ctrl Pts',(23.9380160253658,-1.35530766068394,12.6421586540183));
#46441=CARTESIAN_POINT('Ctrl Pts',(23.7802138865008,1.4691415207263,12.5805967789361));
#46442=CARTESIAN_POINT('Ctrl Pts',(23.6224117476358,2.96382773091694,10.183261230454));
#46443=CARTESIAN_POINT('Ctrl Pts',(23.4646096087708,1.77586500457617,7.62004988265589));
#46444=CARTESIAN_POINT('Ctrl Pts',(23.3068074699057,-1.01948573897858,7.2110024476589));
#46445=CARTESIAN_POINT('Ctrl Pts',(23.1490053310407,-2.8920697325616,9.32635943486548));
#46446=CARTESIAN_POINT('Ctrl Pts',(22.9912031921758,-2.14695539469329,12.0514486071466));
#46447=CARTESIAN_POINT('Ctrl Pts',(22.8334010533107,0.541432062896488,12.9197106215485));
#46448=CARTESIAN_POINT('Ctrl Pts',(22.6755989144457,2.73975327985792,11.1452557874403));
#46449=CARTESIAN_POINT('Ctrl Pts',(22.5177967755807,2.45824235737459,8.33419588553699));
#46450=CARTESIAN_POINT('Ctrl Pts',(22.3599946367157,-0.0482967900857281,
7.03090480968693));
#46451=CARTESIAN_POINT('Ctrl Pts',(22.2021924978507,-2.51112107911298,8.41503004335198));
#46452=CARTESIAN_POINT('Ctrl Pts',(22.0443903589857,-2.7010550356833,11.2337586994981));
#46453=CARTESIAN_POINT('Ctrl Pts',(21.8865882201206,-0.446183791431585,
12.9357756825288));
#46454=CARTESIAN_POINT('Ctrl Pts',(21.7287860812557,2.21254166546862,11.9805348301777));
#46455=CARTESIAN_POINT('Ctrl Pts',(21.5709839423906,2.86862989328224,9.23265303163944));
#46456=CARTESIAN_POINT('Ctrl Pts',(21.4131818035257,0.928235935080519,7.17931978358216));
#46457=CARTESIAN_POINT('Ctrl Pts',(21.2553796646606,-1.85233195970059,7.67906804371988));
#46458=CARTESIAN_POINT('Ctrl Pts',(21.0975775257957,-2.95629913739384,10.2795608069415));
#46459=CARTESIAN_POINT('Ctrl Pts',(20.9397753869306,-1.38443209020732,12.6270147738721));
#46460=CARTESIAN_POINT('Ctrl Pts',(20.7819732480656,1.44052559390759,12.5966795812833));
#46461=CARTESIAN_POINT('Ctrl Pts',(20.6241711092006,2.96162074352487,10.2160125136836));
#46462=CARTESIAN_POINT('Ctrl Pts',(20.4663689703356,1.8020649243605,7.63982609900542));
#46463=CARTESIAN_POINT('Ctrl Pts',(20.3085668314706,-0.988593424005365,
7.19990323800016));
#46464=CARTESIAN_POINT('Ctrl Pts',(20.1507646926056,-2.88444647848355,9.29443118881948));
#46465=CARTESIAN_POINT('Ctrl Pts',(19.9929625537406,-2.16950128546349,12.0275904435855));
#46466=CARTESIAN_POINT('Ctrl Pts',(19.8351604148756,0.509124009193201,12.9255173179817));
#46467=CARTESIAN_POINT('Ctrl Pts',(19.6773582760106,2.72692602947942,11.1754715072237));
#46468=CARTESIAN_POINT('Ctrl Pts',(19.5195561371456,2.47650624293718,8.36147149452918));
#46469=CARTESIAN_POINT('Ctrl Pts',(19.3617539982806,-0.0154729579362931,
7.03055233719803));
#46470=CARTESIAN_POINT('Ctrl Pts',(19.2039518594155,-2.49344712464981,8.38736852594188));
#46471=CARTESIAN_POINT('Ctrl Pts',(19.0461497205505,-2.71452818142837,11.2038253971314));
#46472=CARTESIAN_POINT('Ctrl Pts',(18.8883475816855,-0.478609092173977,
12.9306641178128));
#46473=CARTESIAN_POINT('Ctrl Pts',(18.7305454428205,2.19051331300451,12.0048716318252));
#46474=CARTESIAN_POINT('Ctrl Pts',(18.5727433039555,2.87693700583911,9.26441023730558));
#46475=CARTESIAN_POINT('Ctrl Pts',(18.4149411650905,0.959359498083921,7.1897530023175));
#46476=CARTESIAN_POINT('Ctrl Pts',(18.2571390262255,-1.82656280823216,7.65873385918423));
#46477=CARTESIAN_POINT('Ctrl Pts',(18.0993368873605,-2.95920882245859,10.2468642939564));
#46478=CARTESIAN_POINT('Ctrl Pts',(17.9415347484955,-1.41338696935313,12.6115505182573));
#46479=CARTESIAN_POINT('Ctrl Pts',(17.7837326096305,1.4117334424707,12.61244474046));
#46480=CARTESIAN_POINT('Ctrl Pts',(17.6259304707655,2.95905195190833,10.2487375734681));
#46481=CARTESIAN_POINT('Ctrl Pts',(17.4681283319004,1.82804458221207,7.65989063503597));
#46482=CARTESIAN_POINT('Ctrl Pts',(17.3103261930355,-0.95758027724861,7.18914624230078));
#46483=CARTESIAN_POINT('Ctrl Pts',(17.1525240541704,-2.87647076381356,9.26258913794742));
#46484=CARTESIAN_POINT('Ctrl Pts',(16.9947219153054,-2.19178205930505,12.0034845242866));
#46485=CARTESIAN_POINT('Ctrl Pts',(16.8369197764404,0.476753737537289,12.9309665143586));
#46486=CARTESIAN_POINT('Ctrl Pts',(16.6791176375754,2.7137655550874,11.2055435896593));
#46487=CARTESIAN_POINT('Ctrl Pts',(16.5213154987104,2.49446750237474,8.38894732732178));
#46488=CARTESIAN_POINT('Ctrl Pts',(16.3635133598454,0.0173527655176627,
7.03056272737136));
#46489=CARTESIAN_POINT('Ctrl Pts',(16.2057112209804,-2.47546847521831,8.35990406904119));
#46490=CARTESIAN_POINT('Ctrl Pts',(16.0479090821154,-2.72766961603293,11.1737449894752));
#46491=CARTESIAN_POINT('Ctrl Pts',(15.8901069432504,-0.51097590772646,12.9251944305072));
#46492=CARTESIAN_POINT('Ctrl Pts',(15.7323048043854,2.16821728336033,12.0289634414362));
#46493=CARTESIAN_POINT('Ctrl Pts',(15.5745026655204,2.88489256128098,9.29625733082825));
#46494=CARTESIAN_POINT('Ctrl Pts',(15.4167005266553,0.990365828903469,7.20052962875338));
#46495=CARTESIAN_POINT('Ctrl Pts',(15.2588983877904,-1.80057045371914,7.63868577361231));
#46496=CARTESIAN_POINT('Ctrl Pts',(15.1010962489253,-2.96175689694143,10.2141376145547));
#46497=CARTESIAN_POINT('Ctrl Pts',(14.9432941100604,-1.44216913487621,12.595767135349));
#46498=CARTESIAN_POINT('Ctrl Pts',(14.7854919711953,1.38276877946872,12.6278906630745));
#46499=CARTESIAN_POINT('Ctrl Pts',(14.6276898323303,2.95612156888165,10.2814322379189));
#46500=CARTESIAN_POINT('Ctrl Pts',(14.4698876934653,1.85380085594341,7.6802411286837));
#46501=CARTESIAN_POINT('Ctrl Pts',(14.3120855546003,-0.926450115715597,
7.17873272842893));
#46502=CARTESIAN_POINT('Ctrl Pts',(14.1542834157353,-2.8681435490227,9.23083719750194));
#46503=CARTESIAN_POINT('Ctrl Pts',(13.9964812768703,-2.21379500088899,11.9791337823871));
#46504=CARTESIAN_POINT('Ctrl Pts',(13.8386791380053,0.444325207338179,12.9360575513216));
#46505=CARTESIAN_POINT('Ctrl Pts',(13.6808769991403,2.70027346289051,11.2354683565983));
#46506=CARTESIAN_POINT('Ctrl Pts',(13.5230748602753,2.51212394187823,8.41662002817174));
#46507=CARTESIAN_POINT('Ctrl Pts',(13.3652727214103,0.0501763684915025,
7.03093597802249));
#46508=CARTESIAN_POINT('Ctrl Pts',(13.2074705825453,-2.45718732750359,8.33264002923965));
#46509=CARTESIAN_POINT('Ctrl Pts',(13.0496684436802,-2.74047773377842,11.1435211520554));
#46510=CARTESIAN_POINT('Ctrl Pts',(12.8918663048152,-0.543280282841749,
12.9193672891375));
#46511=CARTESIAN_POINT('Ctrl Pts',(12.7340641659502,2.14565630103725,12.0528073149434));
#46512=CARTESIAN_POINT('Ctrl Pts',(12.5762620270852,2.8924955874703,9.32819042061796));
#46513=CARTESIAN_POINT('Ctrl Pts',(12.4184598882202,1.02125113860777,7.21164834590862));
#46514=CARTESIAN_POINT('Ctrl Pts',(12.2606577493552,-1.77435807238603,7.61892623700522));
#46515=CARTESIAN_POINT('Ctrl Pts',(12.1028556104902,-2.96394304946334,10.1813847675946));
#46516=CARTESIAN_POINT('Ctrl Pts',(11.9450534716252,-1.4707750696622,12.5796665544024));
#46517=CARTESIAN_POINT('Ctrl Pts',(11.7872513327602,1.35363514437794,12.6430154606013));
#46518=CARTESIAN_POINT('Ctrl Pts',(11.6294491938952,2.95282995245311,10.3140925138367));
#46519=CARTESIAN_POINT('Ctrl Pts',(11.4716470550302,1.87933059833343,7.70087508922953));
#46520=CARTESIAN_POINT('Ctrl Pts',(11.3138449161652,-0.895206743759622,
7.16866397645156));
#46521=CARTESIAN_POINT('Ctrl Pts',(11.1560427773002,-2.85946585111029,9.19917923297374));
#46522=CARTESIAN_POINT('Ctrl Pts',(10.9982406384351,-2.23553742137283,11.9545412215237));
#46523=CARTESIAN_POINT('Ctrl Pts',(10.8404384995701,0.411842383436077,12.9407897527962));
#46524=CARTESIAN_POINT('Ctrl Pts',(10.6826363607051,2.6864513975065,11.2652422552064));
#46525=CARTESIAN_POINT('Ctrl Pts',(10.5248342218401,2.52947341174483,8.44448601535835));
#46526=CARTESIAN_POINT('Ctrl Pts',(10.3670320829751,0.0829938248052507,
7.03167242905681));
#46527=CARTESIAN_POINT('Ctrl Pts',(10.2092299441101,-2.43860588617956,8.30557899564397));
#46528=CARTESIAN_POINT('Ctrl Pts',(10.0514278052451,-2.75295102587562,11.1131590082828));
#46529=CARTESIAN_POINT('Ctrl Pts',(9.8936256663801,-0.575518161460093,12.9131806513437));
#46530=CARTESIAN_POINT('Ctrl Pts',(9.73582352751509,2.12283291394444,12.0764056437719));
#46531=CARTESIAN_POINT('Ctrl Pts',(9.57802138865008,2.89974555788266,9.36019538670575));
#46532=CARTESIAN_POINT('Ctrl Pts',(9.42021924978507,1.05201087773083,7.22312747487668));
#46533=CARTESIAN_POINT('Ctrl Pts',(9.26241711092007,-1.74792737402231,7.59941976006281));
#46534=CARTESIAN_POINT('Ctrl Pts',(9.10461497205506,-2.96576988917206,10.1486827597939));
#46535=CARTESIAN_POINT('Ctrl Pts',(8.94681283319005,-1.49919573724511,12.5631101308161));
#46536=CARTESIAN_POINT('Ctrl Pts',(8.78901069432504,1.32432541557472,12.6580881406643));
#46537=CARTESIAN_POINT('Ctrl Pts',(8.63120855546003,2.94919817087565,10.3461924240723));
#46538=CARTESIAN_POINT('Ctrl Pts',(8.47340641659503,1.90459001178303,7.72279827673542));
#46539=CARTESIAN_POINT('Ctrl Pts',(8.31560427773002,-0.863767386924347,
7.1569716946067));
#46540=CARTESIAN_POINT('Ctrl Pts',(8.15780213886501,-2.85068289091044,9.17167184668006));
#46541=CARTESIAN_POINT('Ctrl Pts',(8.05260071295501,-2.45415981120213,11.0035866402229));
#46542=CARTESIAN_POINT('Ctrl Pts',(8.,-1.91346599666512,11.6359872033749));
#46543=CARTESIAN_POINT('Ctrl Pts',(25.8262392198064,-3.00089449353543,9.33589572455167));
#46544=CARTESIAN_POINT('Ctrl Pts',(25.8247009270193,-3.01413331869119,9.41774832515779));
#46545=CARTESIAN_POINT('Ctrl Pts',(25.8236428523257,-3.02293576180228,9.50001791442205));
#46546=CARTESIAN_POINT('Ctrl Pts',(25.8230736514177,-3.02740143036249,9.58247963833164));
#46547=CARTESIAN_POINT('Ctrl Pts',(25.8224963555106,-3.03193060827776,9.66611410733683));
#46548=CARTESIAN_POINT('Ctrl Pts',(25.8224219374901,-3.03199837110086,9.74994735780831));
#46549=CARTESIAN_POINT('Ctrl Pts',(25.8228594276208,-3.02765701722773,9.83373247955964));
#46550=CARTESIAN_POINT('Ctrl Pts',(25.8231188569373,-3.02508261751192,9.88341661034674));
#46551=CARTESIAN_POINT('Ctrl Pts',(25.8235582950085,-3.02095683206533,9.93308349902347));
#46552=CARTESIAN_POINT('Ctrl Pts',(25.8241796248454,-3.01528316277101,9.98267714040271));
#46553=CARTESIAN_POINT('Ctrl Pts',(25.8252586009475,-3.00543049963359,10.0687994392043));
#46554=CARTESIAN_POINT('Ctrl Pts',(25.8268799435765,-2.99097538638735,10.1541420483801));
#46555=CARTESIAN_POINT('Ctrl Pts',(25.8289948543176,-2.97214067508313,10.2384343398583));
#46556=CARTESIAN_POINT('Ctrl Pts',(25.8311660717319,-2.95280451475119,10.3249708009935));
#46557=CARTESIAN_POINT('Ctrl Pts',(25.8338574882923,-2.92885232911599,10.4104015543961));
#46558=CARTESIAN_POINT('Ctrl Pts',(25.8370163033174,-2.9004704184457,10.4944373216573));
#46559=CARTESIAN_POINT('Ctrl Pts',(25.8395515325628,-2.87769141765036,10.5618834788776));
#46560=CARTESIAN_POINT('Ctrl Pts',(25.842387835885,-2.85205786037235,10.6284313817431));
#46561=CARTESIAN_POINT('Ctrl Pts',(25.8454979160497,-2.82364278082183,10.693924553429));
#46562=CARTESIAN_POINT('Ctrl Pts',(25.8494069505495,-2.7879280981151,10.7762423890014));
#46563=CARTESIAN_POINT('Ctrl Pts',(25.8537216893179,-2.74802249289677,10.8564504017753));
#46564=CARTESIAN_POINT('Ctrl Pts',(25.8583471798576,-2.70422623397282,10.934271696085));
#46565=CARTESIAN_POINT('Ctrl Pts',(25.8630134592934,-2.66004376713455,11.0127792407847));
#46566=CARTESIAN_POINT('Ctrl Pts',(25.8679959952607,-2.61190187709947,11.0888588190426));
#46567=CARTESIAN_POINT('Ctrl Pts',(25.8731973010912,-2.56005798819279,11.1622409925269));
#46568=CARTESIAN_POINT('Ctrl Pts',(25.8783373476878,-2.50882469920387,11.2347588954087));
#46569=CARTESIAN_POINT('Ctrl Pts',(25.8836910412979,-2.45397610829872,11.3046435898681));
#46570=CARTESIAN_POINT('Ctrl Pts',(25.8891642993397,-2.39571031021884,11.3716340572743));
#46571=CARTESIAN_POINT('Ctrl Pts',(25.8901970757974,-2.38471584511528,11.3842748239066));
#46572=CARTESIAN_POINT('Ctrl Pts',(25.8912341094429,-2.37359956143892,11.3968125106867));
#46573=CARTESIAN_POINT('Ctrl Pts',(25.8922747681696,-2.36236258457764,11.409245313078));
#46574=CARTESIAN_POINT('Ctrl Pts',(25.8980643682246,-2.2998467951173,11.4784139574821));
#46575=CARTESIAN_POINT('Ctrl Pts',(25.9039451254502,-2.23378997666101,11.5441355297943));
#46576=CARTESIAN_POINT('Ctrl Pts',(25.9098076340753,-2.1644479552529,11.606113861888));
#46577=CARTESIAN_POINT('Ctrl Pts',(25.9152817910467,-2.09969937505019,11.6639865475251));
#46578=CARTESIAN_POINT('Ctrl Pts',(25.9207400370331,-2.03208631420079,11.7185964264391));
#46579=CARTESIAN_POINT('Ctrl Pts',(25.9260932999764,-1.96176778668457,11.7697004547667));
#46580=CARTESIAN_POINT('Ctrl Pts',(25.9264730750774,-1.95677919819684,11.7733259141783));
#46581=CARTESIAN_POINT('Ctrl Pts',(25.9268523218122,-1.95177697185848,11.7769337248518));
#46582=CARTESIAN_POINT('Ctrl Pts',(25.9272310083782,-1.94676115438266,11.7805237977182));
#46583=CARTESIAN_POINT('Ctrl Pts',(25.9290252763024,-1.92299553600559,11.7975340462171));
#46584=CARTESIAN_POINT('Ctrl Pts',(25.9308060613756,-1.89893491844326,11.814139212597));
#46585=CARTESIAN_POINT('Ctrl Pts',(25.9325705627918,-1.87458502252745,11.830329187418));
#46586=CARTESIAN_POINT('Ctrl Pts',(25.9384088208045,-1.79401780187663,11.8838974358511));
#46587=CARTESIAN_POINT('Ctrl Pts',(25.944068810366,-1.71028733025863,11.9329202536286));
#46588=CARTESIAN_POINT('Ctrl Pts',(25.9494490780203,-1.62397669191922,11.9774031117903));
#46589=CARTESIAN_POINT('Ctrl Pts',(25.9530493859837,-1.56622029418781,12.0071696585063));
#46590=CARTESIAN_POINT('Ctrl Pts',(25.9565244380966,-1.50730751226311,12.0349033850039));
#46591=CARTESIAN_POINT('Ctrl Pts',(25.9598438343188,-1.44740009951426,12.0606038454663));
#46592=CARTESIAN_POINT('Ctrl Pts',(8.,-1.91346599666512,11.6359872033749));
#46593=CARTESIAN_POINT('Ctrl Pts',(8.,-1.97562899072746,11.5775692532266));
#46594=CARTESIAN_POINT('Ctrl Pts',(8.00000000000001,-2.0344185889114,11.5158993410469));
#46595=CARTESIAN_POINT('Ctrl Pts',(8.00000000000001,-2.08982174948349,11.4513534699324));
#46596=CARTESIAN_POINT('Ctrl Pts',(8.00000000000001,-2.1465762488304,11.3852332601432));
#46597=CARTESIAN_POINT('Ctrl Pts',(8.00000000000001,-2.19977756879385,11.316094593968));
#46598=CARTESIAN_POINT('Ctrl Pts',(8.00000000000001,-2.24938282561102,11.2442953918663));
#46599=CARTESIAN_POINT('Ctrl Pts',(8.00000000000001,-2.26237822312376,11.2254857085327));
#46600=CARTESIAN_POINT('Ctrl Pts',(8.,-2.27512664525496,11.2064932102818));
#46601=CARTESIAN_POINT('Ctrl Pts',(8.,-2.28762694073546,11.1873238938734));
#46602=CARTESIAN_POINT('Ctrl Pts',(8.,-2.2977159200289,11.1718523526915));
#46603=CARTESIAN_POINT('Ctrl Pts',(8.00000000000001,-2.30764363777327,11.1562648370275));
#46604=CARTESIAN_POINT('Ctrl Pts',(8.00000000000001,-2.31740083565843,11.1405787745481));
#46605=CARTESIAN_POINT('Ctrl Pts',(8.00000000000001,-2.36487425058001,11.0642586095444));
#46606=CARTESIAN_POINT('Ctrl Pts',(8.,-2.40836451010314,10.9855325134811));
#46607=CARTESIAN_POINT('Ctrl Pts',(8.,-2.44783576857742,10.9047923278186));
#46608=CARTESIAN_POINT('Ctrl Pts',(8.,-2.47963039280521,10.8397550332795));
#46609=CARTESIAN_POINT('Ctrl Pts',(8.00000000000001,-2.50881677888913,10.7734098051544));
#46610=CARTESIAN_POINT('Ctrl Pts',(8.00000000000001,-2.53535914135491,10.7059437471017));
#46611=CARTESIAN_POINT('Ctrl Pts',(8.00000000000001,-2.5456178511057,10.6798678953954));
#46612=CARTESIAN_POINT('Ctrl Pts',(8.,-2.55548141093818,10.6536244660234));
#46613=CARTESIAN_POINT('Ctrl Pts',(8.,-2.56494707540061,10.6272237735826));
#46614=CARTESIAN_POINT('Ctrl Pts',(8.,-2.57037504020302,10.6120846325433));
#46615=CARTESIAN_POINT('Ctrl Pts',(8.00000000000001,-2.57567218840733,10.5968934250601));
#46616=CARTESIAN_POINT('Ctrl Pts',(8.00000000000001,-2.58083326929062,10.5816666265579));
#46617=CARTESIAN_POINT('Ctrl Pts',(8.00000000000001,-2.61045215866775,10.4942816638723));
#46618=CARTESIAN_POINT('Ctrl Pts',(8.00000000000001,-2.63563451227559,10.4056131148661));
#46619=CARTESIAN_POINT('Ctrl Pts',(8.00000000000001,-2.65634683466178,10.3160581348443));
#46620=CARTESIAN_POINT('Ctrl Pts',(8.00000000000001,-2.6773791473997,10.2251195953634));
#46621=CARTESIAN_POINT('Ctrl Pts',(8.00000000000001,-2.6938027464082,10.133266219799));
#46622=CARTESIAN_POINT('Ctrl Pts',(8.00000000000001,-2.70554079647472,10.0408806216262));
#46623=CARTESIAN_POINT('Ctrl Pts',(8.00000000000001,-2.71718716742871,9.94921659386775));
#46624=CARTESIAN_POINT('Ctrl Pts',(8.00000000000001,-2.72422124186341,9.85702769697448));
#46625=CARTESIAN_POINT('Ctrl Pts',(8.00000000000001,-2.726521063454,9.76466836326314));
#46626=CARTESIAN_POINT('Ctrl Pts',(8.00000000000001,-2.72766371249266,9.71878032381365));
#46627=CARTESIAN_POINT('Ctrl Pts',(8.,-2.72763693803085,9.67284999779573));
#46628=CARTESIAN_POINT('Ctrl Pts',(8.,-2.72642101212846,9.62692015028946));
#46629=CARTESIAN_POINT('Ctrl Pts',(8.,-2.72605450623643,9.61307591874715));
#46630=CARTESIAN_POINT('Ctrl Pts',(8.00000000000001,-2.72557993734327,9.59923172991306));
#46631=CARTESIAN_POINT('Ctrl Pts',(8.00000000000001,-2.72499670497433,9.58538875478852));
#46632=CARTESIAN_POINT('Ctrl Pts',(8.00000000000001,-2.72437261249071,9.57057596800533));
#46633=CARTESIAN_POINT('Ctrl Pts',(8.00000000000001,-2.72362445980719,9.5557737118897));
#46634=CARTESIAN_POINT('Ctrl Pts',(8.00000000000001,-2.72275224759148,9.54098749246186));
#46635=CARTESIAN_POINT('Ctrl Pts',(8.,-2.71711692851713,9.44545447552171));
#46636=CARTESIAN_POINT('Ctrl Pts',(8.,-2.70630452088264,9.3505388335816));
#46637=CARTESIAN_POINT('Ctrl Pts',(8.,-2.69024345035316,9.25663514051171));
#46638=CARTESIAN_POINT('Ctrl Pts',(8.,-2.68799188729149,9.24347100638487));
#46639=CARTESIAN_POINT('Ctrl Pts',(8.00000000000001,-2.68563709640445,9.23032672963803));
#46640=CARTESIAN_POINT('Ctrl Pts',(8.00000000000001,-2.68317880266814,9.21720337142564));
#46641=CARTESIAN_POINT('Ctrl Pts',(8.00000000000001,-2.66632395667961,9.12722544150852));
#46642=CARTESIAN_POINT('Ctrl Pts',(8.,-2.64460792115915,9.03823106363511));
#46643=CARTESIAN_POINT('Ctrl Pts',(8.,-2.6183336817708,8.95045339427309));
#46644=CARTESIAN_POINT('Ctrl Pts',(8.,-2.59146203306373,8.86067988416082));
#46645=CARTESIAN_POINT('Ctrl Pts',(8.00000000000001,-2.55982233228106,8.77217834086338));
#46646=CARTESIAN_POINT('Ctrl Pts',(8.00000000000001,-2.52368444078896,8.68520171010531));
#46647=CARTESIAN_POINT('Ctrl Pts',(8.00000000000001,-2.51182298835605,8.65665358164747));
#46648=CARTESIAN_POINT('Ctrl Pts',(8.00000000000001,-2.49947651817337,8.62826981102031));
#46649=CARTESIAN_POINT('Ctrl Pts',(8.00000000000001,-2.48665340280304,8.60005962686124));
#46650=CARTESIAN_POINT('Ctrl Pts',(8.00000000000001,-2.47908107936455,8.58340091074254));
#46651=CARTESIAN_POINT('Ctrl Pts',(8.,-2.47134253183697,8.56680273025821));
#46652=CARTESIAN_POINT('Ctrl Pts',(8.,-2.46343939564924,8.55026701909029));
#46653=CARTESIAN_POINT('Ctrl Pts',(8.,-2.45734242320857,8.53751033960472));
#46654=CARTESIAN_POINT('Ctrl Pts',(8.,-2.45114811205187,8.52479227107978));
#46655=CARTESIAN_POINT('Ctrl Pts',(8.,-2.44486281855001,8.51212450604301));
#46656=CARTESIAN_POINT('Ctrl Pts',(8.,-2.40201686213332,8.42577014430926));
#46657=CARTESIAN_POINT('Ctrl Pts',(8.00000000000001,-2.35488188271061,8.34161485601582));
#46658=CARTESIAN_POINT('Ctrl Pts',(8.00000000000001,-2.30380034208708,8.25990966013367));
#46659=CARTESIAN_POINT('Ctrl Pts',(8.00000000000001,-2.25170750980348,8.17658689786312));
#46660=CARTESIAN_POINT('Ctrl Pts',(8.,-2.19550998965609,8.09581142569263));
#46661=CARTESIAN_POINT('Ctrl Pts',(8.,-2.1355160195268,8.01785657644985));
#46662=CARTESIAN_POINT('Ctrl Pts',(8.,-2.07504255195389,7.93927867874322));
#46663=CARTESIAN_POINT('Ctrl Pts',(8.,-2.01071124548655,7.86356583221357));
#46664=CARTESIAN_POINT('Ctrl Pts',(8.,-1.94278853690603,7.79101737230827));
#46665=CARTESIAN_POINT('Ctrl Pts',(8.,-1.90599124384239,7.7517140671804));
#46666=CARTESIAN_POINT('Ctrl Pts',(8.,-1.86813908204872,7.71333990439387));
#46667=CARTESIAN_POINT('Ctrl Pts',(8.,-1.82926920156819,7.67594618621562));
#46668=CARTESIAN_POINT('Ctrl Pts',(8.,-1.81677270980972,7.66392427399833));
#46669=CARTESIAN_POINT('Ctrl Pts',(8.00000000000001,-1.80417100132353,7.65200372369101));
#46670=CARTESIAN_POINT('Ctrl Pts',(8.00000000000001,-1.79146523890468,7.64018631111872));
#46671=CARTESIAN_POINT('Ctrl Pts',(8.00000000000001,-1.78112922343272,7.63057295969917));
#46672=CARTESIAN_POINT('Ctrl Pts',(8.,-1.77072739635744,7.62103074875285));
#46673=CARTESIAN_POINT('Ctrl Pts',(8.,-1.76026664533577,7.61156594719198));
#46674=CARTESIAN_POINT('Ctrl Pts',(8.,-1.68459529142931,7.54309912802346));
#46675=CARTESIAN_POINT('Ctrl Pts',(8.,-1.6057511040431,7.47859424872941));
#46676=CARTESIAN_POINT('Ctrl Pts',(8.,-1.52406119076726,7.41833464906689));
#46677=CARTESIAN_POINT('Ctrl Pts',(8.,-1.44227612341757,7.35800485779604));
#46678=CARTESIAN_POINT('Ctrl Pts',(8.,-1.35763812210306,7.30192940135854));
#46679=CARTESIAN_POINT('Ctrl Pts',(8.,-1.2704302700998,7.25041854115382));
#46680=CARTESIAN_POINT('Ctrl Pts',(8.,-1.18495691856711,7.19993219432963));
#46681=CARTESIAN_POINT('Ctrl Pts',(8.,-1.09701426053311,7.15382999685364));
#46682=CARTESIAN_POINT('Ctrl Pts',(8.,-1.00683484042521,7.11244002002564));
#46683=CARTESIAN_POINT('Ctrl Pts',(8.,-0.96920880645403,7.09517066220173));
#46684=CARTESIAN_POINT('Ctrl Pts',(8.,-0.931193028712579,7.07872212712715));
#46685=CARTESIAN_POINT('Ctrl Pts',(8.,-0.892803010639351,7.06312058236777));
#46686=CARTESIAN_POINT('Ctrl Pts',(8.,-0.860663869165804,7.05005936803672));
#46687=CARTESIAN_POINT('Ctrl Pts',(8.,-0.828262419601745,7.03759180517012));
#46688=CARTESIAN_POINT('Ctrl Pts',(8.,-0.795613156383193,7.02571472931219));
#46689=CARTESIAN_POINT('Ctrl Pts',(25.112583302492,-2.51369118594155,10.0007624228313));
#46690=CARTESIAN_POINT('Ctrl Pts',(25.0892658674683,-2.5146904428337,10.3708906137259));
#46691=CARTESIAN_POINT('Ctrl Pts',(25.0659484324445,-2.43811651330385,10.7406256886329));
#46692=CARTESIAN_POINT('Ctrl Pts',(25.0426309974208,-2.28187612815157,11.0729134384505));
#46693=CARTESIAN_POINT('Ctrl Pts',(24.9900302844658,-1.92942073831072,11.8225058584072));
#46694=CARTESIAN_POINT('Ctrl Pts',(24.9374295715108,-1.17155278170321,12.3815335536695));
#46695=CARTESIAN_POINT('Ctrl Pts',(24.8848288585558,-0.351289714219785,
12.4969436943295));
#46696=CARTESIAN_POINT('Ctrl Pts',(24.8322281456008,0.468973353263639,12.6123538349896));
#46697=CARTESIAN_POINT('Ctrl Pts',(24.7796274326458,1.35163153162298,12.2841464210474));
#46698=CARTESIAN_POINT('Ctrl Pts',(24.7270267196908,1.89724190231406,11.6608859500042));
#46699=CARTESIAN_POINT('Ctrl Pts',(24.6744260067358,2.44285227300514,11.0376254789611));
#46700=CARTESIAN_POINT('Ctrl Pts',(24.6218252937808,2.65141483602796,10.1193119508169));
#46701=CARTESIAN_POINT('Ctrl Pts',(24.5692245808258,2.42853259501223,9.32152656027651));
#46702=CARTESIAN_POINT('Ctrl Pts',(24.5166238678708,2.20565035399651,8.52374116973612));
#46703=CARTESIAN_POINT('Ctrl Pts',(24.4640231549158,1.55132330894224,7.84648391679955));
#46704=CARTESIAN_POINT('Ctrl Pts',(24.4114224419608,0.761681514417321,7.59626555006011));
#46705=CARTESIAN_POINT('Ctrl Pts',(24.3588217290058,-0.0279602801076025,
7.34604718332067));
#46706=CARTESIAN_POINT('Ctrl Pts',(24.3062210160508,-0.95291682410319,7.52286770277837));
#46707=CARTESIAN_POINT('Ctrl Pts',(24.2536203030958,-1.59458768801068,8.04670024587429));
#46708=CARTESIAN_POINT('Ctrl Pts',(24.2066079695612,-2.16808646737625,8.51488002612498));
#46709=CARTESIAN_POINT('Ctrl Pts',(24.1595956360266,-2.51529544719306,9.26025447871382));
#46710=CARTESIAN_POINT('Ctrl Pts',(24.112583302492,-2.52041830912221,10.0014523913097));
#46711=CARTESIAN_POINT('Origin',(8.,0.,10.));
#46712=CARTESIAN_POINT('',(8.,0.,20.));
#46713=CARTESIAN_POINT('Origin',(17.,0.,10.));
#46714=CARTESIAN_POINT('Origin',(8.,0.,10.));
#46715=CARTESIAN_POINT('',(8.,0.,20.));
#46716=CARTESIAN_POINT('Origin',(0.,0.,20.));
#46717=CARTESIAN_POINT('',(8.,9.79717439317883E-16,-5.));
#46718=CARTESIAN_POINT('Origin',(0.,0.,-5.));
#46719=CARTESIAN_POINT('',(8.,9.79717439317883E-16,20.));
#46720=CARTESIAN_POINT('',(8.,9.79717439317883E-16,40.));
#46721=CARTESIAN_POINT('',(8.,9.79717439317883E-16,20.));
#46722=CARTESIAN_POINT('Origin',(0.,0.,40.));
#46723=CARTESIAN_POINT('Origin',(0.,0.,40.));
#46724=CARTESIAN_POINT('Origin',(0.,0.,220.));
#46725=CARTESIAN_POINT('',(-12.,-1.46957615897682E-15,265.));
#46726=CARTESIAN_POINT('Origin',(0.,0.,265.));
#46727=CARTESIAN_POINT('',(-12.,-1.46957615897682E-15,220.));
#46728=CARTESIAN_POINT('Origin',(0.,0.,265.));
#46729=CARTESIAN_POINT('Origin',(0.,0.,41.));
#46730=CARTESIAN_POINT('',(-26.,-3.18408167778312E-15,41.));
#46731=CARTESIAN_POINT('Origin',(0.,0.,41.));
#46732=CARTESIAN_POINT('',(-20.,-2.44929359829471E-15,41.));
#46733=CARTESIAN_POINT('Origin',(0.,0.,41.));
#46734=CARTESIAN_POINT('Origin',(0.,0.,37.));
#46735=CARTESIAN_POINT('',(-26.,-3.18408167778312E-15,37.));
#46736=CARTESIAN_POINT('Origin',(0.,0.,37.));
#46737=CARTESIAN_POINT('',(-20.,2.44929359829471E-15,37.));
#46738=CARTESIAN_POINT('Origin',(0.,0.,37.));
#46739=CARTESIAN_POINT('Origin',(0.,0.,37.));
#46740=CARTESIAN_POINT('',(-26.,-3.18408167778312E-15,37.));
#46741=CARTESIAN_POINT('Origin',(0.,0.,20.));
#46742=CARTESIAN_POINT('',(-20.,-2.44929359829471E-15,20.));
#46743=CARTESIAN_POINT('',(-20.,-2.44929359829471E-15,20.));
#46744=CARTESIAN_POINT('Origin',(0.,0.,20.));
#46745=CARTESIAN_POINT('Origin',(0.,0.,20.));
#46746=CARTESIAN_POINT('',(-26.,-3.18408167778312E-15,20.));
#46747=CARTESIAN_POINT('Origin',(0.,0.,20.));
#46748=CARTESIAN_POINT('Origin',(0.,0.,0.));
#46749=CARTESIAN_POINT('',(-26.,-3.18408167778312E-15,-5.));
#46750=CARTESIAN_POINT('',(-26.,-3.18408167778312E-15,0.));
#46751=CARTESIAN_POINT('Origin',(0.,0.,-5.));
#46752=CARTESIAN_POINT('Origin',(0.,0.,-5.));
#46753=CARTESIAN_POINT('Origin',(0.,0.,20.));
#46754=CARTESIAN_POINT('',(-20.,-2.44929359829471E-15,20.));
#46755=CARTESIAN_POINT('',(0.,0.,0.));
#46756=CARTESIAN_POINT('Origin',(0.,0.,59.));
#46757=CARTESIAN_POINT('',(-20.,-2.44929359829471E-15,161.));
#46758=CARTESIAN_POINT('Origin',(0.,0.,161.));
#46759=CARTESIAN_POINT('',(-20.,-2.44929359829471E-15,59.));
#46760=CARTESIAN_POINT('',(-20.,-2.44929359829471E-15,59.));
#46761=CARTESIAN_POINT('Origin',(0.,0.,59.));
#46762=CARTESIAN_POINT('Origin',(0.,0.,59.));
#46763=CARTESIAN_POINT('',(-27.,-3.30654635769785E-15,161.));
#46764=CARTESIAN_POINT('Origin',(0.,0.,161.));
#46765=CARTESIAN_POINT('',(-27.,-3.30654635769785E-15,59.));
#46766=CARTESIAN_POINT('',(-27.,-3.30654635769785E-15,59.));
#46767=CARTESIAN_POINT('Origin',(0.,0.,59.));
#46768=CARTESIAN_POINT('Origin',(0.,0.,161.));
#46769=CARTESIAN_POINT('Origin',(0.,0.,59.));
#46770=CARTESIAN_POINT('',(0.,0.,0.));
#46771=CARTESIAN_POINT('Origin',(0.,0.,179.));
#46772=CARTESIAN_POINT('',(-20.,-2.44929359829471E-15,181.));
#46773=CARTESIAN_POINT('Origin',(0.,0.,181.));
#46774=CARTESIAN_POINT('',(-20.,-2.44929359829471E-15,179.));
#46775=CARTESIAN_POINT('',(-20.,-2.44929359829471E-15,179.));
#46776=CARTESIAN_POINT('Origin',(0.,0.,179.));
#46777=CARTESIAN_POINT('Origin',(0.,0.,179.));
#46778=CARTESIAN_POINT('',(-27.5,-3.36777869765522E-15,181.));
#46779=CARTESIAN_POINT('Origin',(0.,0.,181.));
#46780=CARTESIAN_POINT('',(-27.5,-3.36777869765522E-15,179.));
#46781=CARTESIAN_POINT('',(-27.5,-3.36777869765522E-15,179.));
#46782=CARTESIAN_POINT('Origin',(0.,0.,179.));
#46783=CARTESIAN_POINT('Origin',(0.,0.,181.));
#46784=CARTESIAN_POINT('Origin',(0.,0.,179.));
#46785=CARTESIAN_POINT('',(0.,0.,0.));
#46786=CARTESIAN_POINT('Origin',(-1.,0.,1.));
#46787=CARTESIAN_POINT('',(-1.,18.9736659610103,0.));
#46788=CARTESIAN_POINT('',(-1.,18.9736659610103,1.));
#46789=CARTESIAN_POINT('',(-1.,18.9736659610103,0.));
#46790=CARTESIAN_POINT('',(-1.,26.9814751264641,0.));
#46791=CARTESIAN_POINT('',(-1.,0.,0.));
#46792=CARTESIAN_POINT('',(-1.,26.9814751264641,1.));
#46793=CARTESIAN_POINT('',(-1.,26.9814751264641,0.));
#46794=CARTESIAN_POINT('',(-1.,0.,1.));
#46795=CARTESIAN_POINT('Origin',(1.,54.,1.));
#46796=CARTESIAN_POINT('',(1.,18.9736659610103,1.));
#46797=CARTESIAN_POINT('',(1.,18.9736659610103,0.));
#46798=CARTESIAN_POINT('',(1.,18.9736659610103,0.));
#46799=CARTESIAN_POINT('',(1.,26.9814751264641,1.));
#46800=CARTESIAN_POINT('',(1.,27.,1.));
#46801=CARTESIAN_POINT('',(1.,26.9814751264641,0.));
#46802=CARTESIAN_POINT('',(1.,26.9814751264641,0.));
#46803=CARTESIAN_POINT('',(1.,27.,0.));
#46804=CARTESIAN_POINT('Origin',(0.,0.,0.));
#46805=CARTESIAN_POINT('Origin',(0.,0.,0.));
#46806=CARTESIAN_POINT('Origin',(0.,0.,0.));
#46807=CARTESIAN_POINT('Origin',(0.,0.,0.));
#46808=CARTESIAN_POINT('Origin',(0.,0.,1.));
#46809=CARTESIAN_POINT('Origin',(0.,0.,0.));
#46810=CARTESIAN_POINT('Origin',(0.,0.,1.));
#46811=CARTESIAN_POINT('Origin',(0.,0.,1.));
#46812=CARTESIAN_POINT('',(0.,0.,0.));
#46813=CARTESIAN_POINT('Origin',(-46.,3.,80.));
#46814=CARTESIAN_POINT('',(-46.,3.,80.));
#46815=CARTESIAN_POINT('',(-54.,3.,80.));
#46816=CARTESIAN_POINT('',(-46.,3.,80.));
#46817=CARTESIAN_POINT('',(-54.,3.,140.));
#46818=CARTESIAN_POINT('',(-54.,3.,80.));
#46819=CARTESIAN_POINT('',(-46.,3.,140.));
#46820=CARTESIAN_POINT('',(-46.,3.,140.));
#46821=CARTESIAN_POINT('',(-46.,3.,80.));
#46822=CARTESIAN_POINT('Origin',(-46.,-3.,80.));
#46823=CARTESIAN_POINT('',(-46.,-3.,80.));
#46824=CARTESIAN_POINT('',(-46.,-3.,80.));
#46825=CARTESIAN_POINT('',(-46.,-3.,140.));
#46826=CARTESIAN_POINT('',(-46.,-3.,140.));
#46827=CARTESIAN_POINT('',(-46.,-3.,80.));
#46828=CARTESIAN_POINT('Origin',(-54.,-3.,80.));
#46829=CARTESIAN_POINT('',(-54.,-3.,80.));
#46830=CARTESIAN_POINT('',(-54.,-3.,80.));
#46831=CARTESIAN_POINT('',(-54.,-3.,140.));
#46832=CARTESIAN_POINT('',(-54.,-3.,140.));
#46833=CARTESIAN_POINT('',(-54.,-3.,80.));
#46834=CARTESIAN_POINT('Origin',(-54.,3.,80.));
#46835=CARTESIAN_POINT('',(-54.,3.,80.));
#46836=CARTESIAN_POINT('',(-54.,3.,140.));
#46837=CARTESIAN_POINT('Origin',(-50.,0.,140.));
#46838=CARTESIAN_POINT('Origin',(-50.,0.,80.));
#46839=CARTESIAN_POINT('',(0.,0.,0.));
#46840=CARTESIAN_POINT('Origin',(0.,0.,-10.));
#46841=CARTESIAN_POINT('',(-5.90914966774444,0.00356580792582911,-7.6866248077951));
#46842=CARTESIAN_POINT('',(-5.90684818604763,7.69732782816217E-5,-7.93837519220449));
#46843=CARTESIAN_POINT('',(-5.91675,-7.2459289488551E-16,-10.));
#46844=CARTESIAN_POINT('',(-1.76006007606278,-5.64890423809343,-9.08325));
#46845=CARTESIAN_POINT('Ctrl Pts',(-5.90914966774444,0.00356580792582911,
-7.6866248077951));
#46846=CARTESIAN_POINT('Ctrl Pts',(-5.91328542926688,0.757557195719996,
-7.72201370069112));
#46847=CARTESIAN_POINT('Ctrl Pts',(-5.77952731968195,1.51013660070763,-7.75740259358713));
#46848=CARTESIAN_POINT('Ctrl Pts',(-5.50114206197789,2.20475331667403,-7.79279148648315));
#46849=CARTESIAN_POINT('Ctrl Pts',(-4.77121527592137,4.02603994373196,-7.88558124505991));
#46850=CARTESIAN_POINT('Ctrl Pts',(-3.04699187872556,5.44883910826404,-7.97837100363666));
#46851=CARTESIAN_POINT('Ctrl Pts',(-1.1202364612261,5.81970068129217,-8.07116076221342));
#46852=CARTESIAN_POINT('Ctrl Pts',(0.806518956273354,6.1905622543203,-8.16395052079018));
#46853=CARTESIAN_POINT('Ctrl Pts',(2.93580639407646,5.50948623584449,-8.25674027936694));
#46854=CARTESIAN_POINT('Ctrl Pts',(4.28964970625473,4.08933490559468,-8.34953003794369));
#46855=CARTESIAN_POINT('Ctrl Pts',(5.64349301843301,2.66918357534486,-8.44231979652045));
#46856=CARTESIAN_POINT('Ctrl Pts',(6.22189220498645,0.509956933321043,-8.53510955509721));
#46857=CARTESIAN_POINT('Ctrl Pts',(5.7594588630459,-1.39690584090804,-8.62789931367396));
#46858=CARTESIAN_POINT('Ctrl Pts',(5.29702552110535,-3.30376861513711,-8.72068907225072));
#46859=CARTESIAN_POINT('Ctrl Pts',(3.79375965067081,-4.95826752157145,-8.81347883082748));
#46860=CARTESIAN_POINT('Ctrl Pts',(1.93957562617669,-5.60028674616276,-8.90626858940423));
#46861=CARTESIAN_POINT('Ctrl Pts',(0.76072388940282,-6.0084692501395,-8.96526239293616));
#46862=CARTESIAN_POINT('Ctrl Pts',(-0.559974320405811,-6.00739201583435,
-9.02425619646808));
#46863=CARTESIAN_POINT('Ctrl Pts',(-1.76205604469195,-5.64092543727167,
-9.08325));
#46864=CARTESIAN_POINT('',(3.34982837776095,-4.87714879843208,-9.08325));
#46865=CARTESIAN_POINT('Origin',(0.,0.,-9.08325));
#46866=CARTESIAN_POINT('Ctrl Pts',(3.3444648754246,-4.86859341898359,-9.08325));
#46867=CARTESIAN_POINT('Ctrl Pts',(4.33259176949258,-4.18349695521928,-9.02678881114205));
#46868=CARTESIAN_POINT('Ctrl Pts',(5.12344724565752,-3.20972013684931,-8.9703276222841));
#46869=CARTESIAN_POINT('Ctrl Pts',(5.54426475499171,-2.09385801960084,-8.91386643342615));
#46870=CARTESIAN_POINT('Ctrl Pts',(6.23598258217496,-0.259662193480346,
-8.82105848221044));
#46871=CARTESIAN_POINT('Ctrl Pts',(5.9278923803199,1.95843484105861,-8.72825053099474));
#46872=CARTESIAN_POINT('Ctrl Pts',(4.75815453645331,3.53476303607018,-8.63544257977903));
#46873=CARTESIAN_POINT('Ctrl Pts',(3.58841669258673,5.11109123108174,-8.54263462856332));
#46874=CARTESIAN_POINT('Ctrl Pts',(1.55703120670862,6.04565058656591,-8.4498266773476));
#46875=CARTESIAN_POINT('Ctrl Pts',(-0.40117185096479,5.91244101960478,-8.35701872613189));
#46876=CARTESIAN_POINT('Ctrl Pts',(-2.3593749086382,5.77923145264365,-8.26421077491618));
#46877=CARTESIAN_POINT('Ctrl Pts',(-4.24439553810691,4.57825296323722,-8.17140282370047));
#46878=CARTESIAN_POINT('Ctrl Pts',(-5.19107535624382,2.85949434106974,-8.07859487248476));
#46879=CARTESIAN_POINT('Ctrl Pts',(-5.66784176719644,1.99389399353369,-8.03185497905801));
#46880=CARTESIAN_POINT('Ctrl Pts',(-5.90661436346097,0.996967727442935,
-7.98511508563125));
#46881=CARTESIAN_POINT('Ctrl Pts',(-5.90684818604763,7.69732782816216E-5,
-7.93837519220449));
#46882=CARTESIAN_POINT('Origin',(0.,0.,-10.));
#46883=CARTESIAN_POINT('',(-5.91124449814648,-0.00463389484992694,-5.93662480779511));
#46884=CARTESIAN_POINT('',(-5.9180539583466,-0.00537329958833666,-6.18837519220452));
#46885=CARTESIAN_POINT('',(-5.91675,-7.2459289488551E-16,-10.));
#46886=CARTESIAN_POINT('Ctrl Pts',(-5.91124449814648,-0.00463389484992693,
-5.93662480779511));
#46887=CARTESIAN_POINT('Ctrl Pts',(-5.90163171584489,1.31481634025305,-5.99860848256392));
#46888=CARTESIAN_POINT('Ctrl Pts',(-5.46550912136613,2.64003051865407,-6.06059215733273));
#46889=CARTESIAN_POINT('Ctrl Pts',(-4.65401854734394,3.66929885831296,-6.12257583210154));
#46890=CARTESIAN_POINT('Ctrl Pts',(-3.43921457304457,5.21011684149748,-6.21536559067829));
#46891=CARTESIAN_POINT('Ctrl Pts',(-1.38320399826394,6.0877147140118,-6.30815534925505));
#46892=CARTESIAN_POINT('Ctrl Pts',(0.56981453680638,5.89906436771486,-6.4009451078318));
#46893=CARTESIAN_POINT('Ctrl Pts',(2.5228330718767,5.71041402141791,-6.49373486640856));
#46894=CARTESIAN_POINT('Ctrl Pts',(4.3728595672367,4.4555154563097,-6.58652462498532));
#46895=CARTESIAN_POINT('Ctrl Pts',(5.27028709003435,2.71066883561754,-6.67931438356208));
#46896=CARTESIAN_POINT('Ctrl Pts',(6.167714612832,0.965822214925369,-6.77210414213884));
#46897=CARTESIAN_POINT('Ctrl Pts',(6.1125431630673,-1.26897246135075,-6.86489390071559));
#46898=CARTESIAN_POINT('Ctrl Pts',(5.13011480377032,-2.96741404802536,-6.95768365929235));
#46899=CARTESIAN_POINT('Ctrl Pts',(4.14768644447333,-4.66585563469996,-7.0504734178691));
#46900=CARTESIAN_POINT('Ctrl Pts',(2.23800117564407,-5.82794413177304,-7.14326317644586));
#46901=CARTESIAN_POINT('Ctrl Pts',(0.278051023782169,-5.91999652376047,
-7.23605293502262));
#46902=CARTESIAN_POINT('Ctrl Pts',(-1.68189912807974,-6.01204891574791,
-7.32884269359937));
#46903=CARTESIAN_POINT('Ctrl Pts',(-3.69211416297429,-5.0340652026497,-7.42163245217613));
#46904=CARTESIAN_POINT('Ctrl Pts',(-4.82940659296296,-3.4351863013087,-7.51442221075289));
#46905=CARTESIAN_POINT('Ctrl Pts',(-5.53294943017705,-2.44610049633029,
-7.57182307643363));
#46906=CARTESIAN_POINT('Ctrl Pts',(-5.90244145304175,-1.21940995744712,
-7.62922394211437));
#46907=CARTESIAN_POINT('Ctrl Pts',(-5.90914966774444,0.00356580792582911,
-7.6866248077951));
#46908=CARTESIAN_POINT('Ctrl Pts',(-5.90684818604763,7.69732782816216E-5,
-7.93837519220449));
#46909=CARTESIAN_POINT('Ctrl Pts',(-5.90707864768639,-0.982484549761922,
-7.89230713441554));
#46910=CARTESIAN_POINT('Ctrl Pts',(-5.67557852724961,-1.96501157443031,
-7.84623907662659));
#46911=CARTESIAN_POINT('Ctrl Pts',(-5.21182602918055,-2.82172617607135,
-7.80017101883763));
#46912=CARTESIAN_POINT('Ctrl Pts',(-4.27755787717527,-4.54764931611639,
-7.70736306762192));
#46913=CARTESIAN_POINT('Ctrl Pts',(-2.40068256635962,-5.76295684127793,
-7.61455511640621));
#46914=CARTESIAN_POINT('Ctrl Pts',(-0.443673941101387,-5.90981951500856,
-7.5217471651905));
#46915=CARTESIAN_POINT('Ctrl Pts',(1.51333468415685,-6.05668218873918,-7.42893921397479));
#46916=CARTESIAN_POINT('Ctrl Pts',(3.55047662385768,-5.13510001103889,-7.33613126275908));
#46917=CARTESIAN_POINT('Ctrl Pts',(4.73200308253274,-3.56819310617019,-7.24332331154337));
#46918=CARTESIAN_POINT('Ctrl Pts',(5.91352954120779,-2.00128620130149,-7.15051536032766));
#46919=CARTESIAN_POINT('Ctrl Pts',(6.23944051885709,0.210945430735604,-7.05770740911195));
#46920=CARTESIAN_POINT('Ctrl Pts',(5.55994672995165,2.0520574898606,-6.96489945789624));
#46921=CARTESIAN_POINT('Ctrl Pts',(4.88045294104622,3.8931695489856,-6.87209150668053));
#46922=CARTESIAN_POINT('Ctrl Pts',(3.19555438558608,5.3631620351985,-6.77928355546483));
#46923=CARTESIAN_POINT('Ctrl Pts',(1.2793340040228,5.78678727197991,-6.68647560424912));
#46924=CARTESIAN_POINT('Ctrl Pts',(-0.63688637754048,6.21041250876132,-6.59366765303341));
#46925=CARTESIAN_POINT('Ctrl Pts',(-2.78442858520689,5.58767049611123,-6.50085970181769));
#46926=CARTESIAN_POINT('Ctrl Pts',(-4.17672173121847,4.20461291148561,-6.40805175060198));
#46927=CARTESIAN_POINT('Ctrl Pts',(-5.27524171285711,3.11337979235374,-6.33482623113616));
#46928=CARTESIAN_POINT('Ctrl Pts',(-5.90360270323821,1.54883366893403,-6.26160071167034));
#46929=CARTESIAN_POINT('Ctrl Pts',(-5.9180539583466,-0.00537329958833666,
-6.18837519220452));
#46930=CARTESIAN_POINT('Origin',(0.,0.,-10.));
#46931=CARTESIAN_POINT('',(-5.92596791550767,-0.00164632128292097,-4.1866248077951));
#46932=CARTESIAN_POINT('',(-5.92512149738253,0.00261993485437684,-4.43837519220451));
#46933=CARTESIAN_POINT('',(-5.91675,-7.2459289488551E-16,-10.));
#46934=CARTESIAN_POINT('Ctrl Pts',(-5.92596791550767,-0.00164632128292097,
-4.1866248077951));
#46935=CARTESIAN_POINT('Ctrl Pts',(-5.91906177124303,1.87187930368298,-4.27520326443671));
#46936=CARTESIAN_POINT('Ctrl Pts',(-4.95561321993308,3.75151790639186,-4.36378172107832));
#46937=CARTESIAN_POINT('Ctrl Pts',(-3.42759171092563,4.83479689493213,-4.45236017771992));
#46938=CARTESIAN_POINT('Ctrl Pts',(-1.82692319290707,5.96957841663579,-4.54514993629668));
#46939=CARTESIAN_POINT('Ctrl Pts',(0.39327761073488,6.2304773245562,-4.63793969487344));
#46940=CARTESIAN_POINT('Ctrl Pts',(2.21340809258917,5.49767866152403,-4.73072945345019));
#46941=CARTESIAN_POINT('Ctrl Pts',(4.03353857444347,4.76487999849185,-4.82351921202695));
#46942=CARTESIAN_POINT('Ctrl Pts',(5.45359873451011,3.03838376450709,-4.91630897060371));
#46943=CARTESIAN_POINT('Ctrl Pts',(5.82144160499229,1.11106428290431,-5.00909872918046));
#46944=CARTESIAN_POINT('Ctrl Pts',(6.18928447547447,-0.816255198698479,
-5.10188848775722));
#46945=CARTESIAN_POINT('Ctrl Pts',(5.50491005637218,-2.94439792791929,-5.19467824633398));
#46946=CARTESIAN_POINT('Ctrl Pts',(4.08260983745286,-4.29603799551428,-5.28746800491073));
#46947=CARTESIAN_POINT('Ctrl Pts',(2.66030961853354,-5.64767806310926,-5.38025776348749));
#46948=CARTESIAN_POINT('Ctrl Pts',(0.500083599797188,-6.22281546907843,
-5.47304752206424));
#46949=CARTESIAN_POINT('Ctrl Pts',(-1.40600855129438,-5.75732457831857,
-5.565837280641));
#46950=CARTESIAN_POINT('Ctrl Pts',(-3.31210070238594,-5.29183368755872,
-5.65862703921776));
#46951=CARTESIAN_POINT('Ctrl Pts',(-4.96405898583272,-3.78571450006987,
-5.75141679779452));
#46952=CARTESIAN_POINT('Ctrl Pts',(-5.60323944064706,-1.93063585939808,
-5.84420655637127));
#46953=CARTESIAN_POINT('Ctrl Pts',(-5.81544655230931,-1.31475207058976,
-5.87501264017922));
#46954=CARTESIAN_POINT('Ctrl Pts',(-5.91602208157172,-0.66040486478031,
-5.90581872398716));
#46955=CARTESIAN_POINT('Ctrl Pts',(-5.91124449814648,-0.00463389484992693,
-5.93662480779511));
#46956=CARTESIAN_POINT('Ctrl Pts',(-5.9180539583466,-0.00537329958833666,
-6.18837519220452));
#46957=CARTESIAN_POINT('Ctrl Pts',(-5.92191860442798,-0.421009161352276,
-6.16879276045463));
#46958=CARTESIAN_POINT('Ctrl Pts',(-5.88187836580504,-0.835905599423084,
-6.14921032870475));
#46959=CARTESIAN_POINT('Ctrl Pts',(-5.79518393962897,-1.24081253117895,
-6.12962789695486));
#46960=CARTESIAN_POINT('Ctrl Pts',(-5.38430891767115,-3.1598072326167,-6.03681994573915));
#46961=CARTESIAN_POINT('Ctrl Pts',(-3.92551478939875,-4.85442347889104,
-5.94401199452343));
#46962=CARTESIAN_POINT('Ctrl Pts',(-2.08898215973251,-5.5461589296916,-5.85120404330772));
#46963=CARTESIAN_POINT('Ctrl Pts',(-0.252449530066264,-6.23789438049217,
-5.75839609209201));
#46964=CARTESIAN_POINT('Ctrl Pts',(1.96182160099383,-5.92674903581894,-5.66558814087631));
#46965=CARTESIAN_POINT('Ctrl Pts',(3.53658941057065,-4.75565854394093,-5.5727801896606));
#46966=CARTESIAN_POINT('Ctrl Pts',(5.11135722014747,-3.58456805206292,-5.47997223844489));
#46967=CARTESIAN_POINT('Ctrl Pts',(6.04662170824101,-1.55353241298013,-5.38716428722918));
#46968=CARTESIAN_POINT('Ctrl Pts',(5.91271741582685,0.404379920195457,-5.29435633601347));
#46969=CARTESIAN_POINT('Ctrl Pts',(5.7788131234127,2.36229225337103,-5.20154838479775));
#46970=CARTESIAN_POINT('Ctrl Pts',(4.57574005049085,4.24708128063941,-5.10874043358204));
#46971=CARTESIAN_POINT('Ctrl Pts',(2.85619526042756,5.19286940926132,-5.01593248236633));
#46972=CARTESIAN_POINT('Ctrl Pts',(1.13665047036426,6.13865753788323,-4.92312453115062));
#46973=CARTESIAN_POINT('Ctrl Pts',(-1.09936603684048,6.14544476785868,-4.83031657993492));
#46974=CARTESIAN_POINT('Ctrl Pts',(-2.82462024052683,5.21011217386649,-4.73750862871921));
#46975=CARTESIAN_POINT('Ctrl Pts',(-4.54987444421319,4.27477957987429,-4.6447006775035));
#46976=CARTESIAN_POINT('Ctrl Pts',(-5.76436634438116,2.39732716191442,-4.55189272628778));
#46977=CARTESIAN_POINT('Ctrl Pts',(-5.91015356810031,0.440264092825153,
-4.45908477507207));
#46978=CARTESIAN_POINT('Ctrl Pts',(-5.92099743995646,0.294694813198242,
-4.45218158078288));
#46979=CARTESIAN_POINT('Ctrl Pts',(-5.92592858883168,0.148685079125095,
-4.4452783864937));
#46980=CARTESIAN_POINT('Ctrl Pts',(-5.92512149738253,0.00261993485437684,
-4.43837519220451));
#46981=CARTESIAN_POINT('Origin',(0.,0.,-10.));
#46982=CARTESIAN_POINT('',(-5.91623372814898,0.00546481507842006,-2.4366248077951));
#46983=CARTESIAN_POINT('',(-5.90999536725745,0.0040860534926895,-2.6883751922045));
#46984=CARTESIAN_POINT('',(-5.91675,-7.2459289488551E-16,-10.));
#46985=CARTESIAN_POINT('Ctrl Pts',(-5.91623372814898,0.00546481507842006,
-2.4366248077951));
#46986=CARTESIAN_POINT('Ctrl Pts',(-5.92059929034551,0.480925655459938,
-2.45900828773275));
#46987=CARTESIAN_POINT('Ctrl Pts',(-5.86811878257571,0.955434629522007,
-2.48139176767039));
#46988=CARTESIAN_POINT('Ctrl Pts',(-5.75510650687943,1.41506011009764,-2.50377524760804));
#46989=CARTESIAN_POINT('Ctrl Pts',(-5.28661895234013,3.32041787828841,-2.5965650061848));
#46990=CARTESIAN_POINT('Ctrl Pts',(-3.77790412893443,4.97000555564954,-2.68935476476155));
#46991=CARTESIAN_POINT('Ctrl Pts',(-1.92182261689083,5.60626826399261,-2.78214452333831));
#46992=CARTESIAN_POINT('Ctrl Pts',(-0.0657411048472262,6.24253097233568,
-2.87493428191507));
#46993=CARTESIAN_POINT('Ctrl Pts',(2.13770709583431,5.86546871166071,-2.96772404049182));
#46994=CARTESIAN_POINT('Ctrl Pts',(3.67661279380201,4.64824315028558,-3.06051379906858));
#46995=CARTESIAN_POINT('Ctrl Pts',(5.21551849176971,3.43101758891044,-3.15330355764534));
#46996=CARTESIAN_POINT('Ctrl Pts',(6.08988168702359,1.37362872683514,-3.24609331622209));
#46997=CARTESIAN_POINT('Ctrl Pts',(5.89816076077324,-0.579090377210239,
-3.33888307479885));
#46998=CARTESIAN_POINT('Ctrl Pts',(5.7064398345229,-2.53180948125562,-3.4316728333756));
#46999=CARTESIAN_POINT('Ctrl Pts',(4.44863478676834,-4.37985882727109,-3.52446259195236));
#47000=CARTESIAN_POINT('Ctrl Pts',(2.70237866321106,-5.27454221436282,-3.61725235052912));
#47001=CARTESIAN_POINT('Ctrl Pts',(0.956122539653778,-6.16922560145455,
-3.71004210910587));
#47002=CARTESIAN_POINT('Ctrl Pts',(-1.27858465970622,-6.11054302962255,
-3.80283186768263));
#47003=CARTESIAN_POINT('Ctrl Pts',(-2.9754783984976,-5.12544381703233,-3.89562162625939));
#47004=CARTESIAN_POINT('Ctrl Pts',(-4.67237213728899,-4.14034460444212,
-3.98841138483614));
#47005=CARTESIAN_POINT('Ctrl Pts',(-5.83145241551177,-2.2288287510937,-4.0812011434129));
#47006=CARTESIAN_POINT('Ctrl Pts',(-5.92042443842556,-0.268738756676046,
-4.17399090198966));
#47007=CARTESIAN_POINT('Ctrl Pts',(-5.92446247083364,-0.179779253890741,
-4.17820220392481));
#47008=CARTESIAN_POINT('Ctrl Pts',(-5.92629625560083,-0.0907196963349705,
-4.18241350585995));
#47009=CARTESIAN_POINT('Ctrl Pts',(-5.92596791550767,-0.00164632128292097,
-4.1866248077951));
#47010=CARTESIAN_POINT('Ctrl Pts',(-5.92512149738253,0.00261993485437684,
-4.43837519220451));
#47011=CARTESIAN_POINT('Ctrl Pts',(-5.91507788686657,-1.8150444953158,-4.35247043527799));
#47012=CARTESIAN_POINT('Ctrl Pts',(-5.01642065476797,-3.64128964946244,
-4.26656567835147));
#47013=CARTESIAN_POINT('Ctrl Pts',(-3.56539308202037,-4.73410171351781,
-4.18066092142495));
#47014=CARTESIAN_POINT('Ctrl Pts',(-1.99776282495092,-5.91473073055283,
-4.08785297020924));
#47015=CARTESIAN_POINT('Ctrl Pts',(0.214580236458331,-6.23931504440418,
-3.99504501899353));
#47016=CARTESIAN_POINT('Ctrl Pts',(2.05527741171376,-5.55873927088791,-3.90223706777781));
#47017=CARTESIAN_POINT('Ctrl Pts',(3.89597458696917,-4.87816349737166,-3.80942911656211));
#47018=CARTESIAN_POINT('Ctrl Pts',(5.36502587607076,-3.19242763648782,-3.7166211653464));
#47019=CARTESIAN_POINT('Ctrl Pts',(5.78754354247752,-1.27596516977657,-3.62381321413069));
#47020=CARTESIAN_POINT('Ctrl Pts',(6.21006120888429,0.640497296934686,-3.53100526291498));
#47021=CARTESIAN_POINT('Ctrl Pts',(5.5860452525962,2.78768636947335,-3.43819731169927));
#47022=CARTESIAN_POINT('Ctrl Pts',(4.20217097506051,4.17917532158192,-3.34538936048356));
#47023=CARTESIAN_POINT('Ctrl Pts',(2.81829669752482,5.5706642736905,-3.25258140926785));
#47024=CARTESIAN_POINT('Ctrl Pts',(0.674564098741514,6.20645310536897,-3.15977345805214));
#47025=CARTESIAN_POINT('Ctrl Pts',(-1.24418798567351,5.7944580097669,-3.06696550683643));
#47026=CARTESIAN_POINT('Ctrl Pts',(-3.1629400700885,5.38246291416483,-2.97415755562072));
#47027=CARTESIAN_POINT('Ctrl Pts',(-4.85671164013523,3.92268389128225,-2.88134960440501));
#47028=CARTESIAN_POINT('Ctrl Pts',(-5.5473776410707,2.08574894203492,-2.7885416531893));
#47029=CARTESIAN_POINT('Ctrl Pts',(-5.79585336658777,1.42488863673007,-2.75515283286103));
#47030=CARTESIAN_POINT('Ctrl Pts',(-5.91449808653743,0.715213396403952,
-2.72176401253277));
#47031=CARTESIAN_POINT('Ctrl Pts',(-5.90999536725745,0.0040860534926895,
-2.6883751922045));
#47032=CARTESIAN_POINT('Origin',(0.,0.,-10.));
#47033=CARTESIAN_POINT('',(-5.90707267146128,-0.000907514317987079,-0.6866248077951));
#47034=CARTESIAN_POINT('',(-5.91020249175295,-0.00419241645486733,-0.93837519220451));
#47035=CARTESIAN_POINT('',(-5.91675,-7.2459289488551E-16,-10.));
#47036=CARTESIAN_POINT('Ctrl Pts',(-5.90707267146128,-0.000907514317987079,
-0.6866248077951));
#47037=CARTESIAN_POINT('Ctrl Pts',(-5.90564731739626,1.04354150490343,-0.735603069605543));
#47038=CARTESIAN_POINT('Ctrl Pts',(-5.64214242329099,2.0886625894451,-0.784581331415985));
#47039=CARTESIAN_POINT('Ctrl Pts',(-5.1207586220131,2.98353433950782,-0.833559593226428));
#47040=CARTESIAN_POINT('Ctrl Pts',(-4.13299230981434,4.6788769379619,-0.926349351803184));
#47041=CARTESIAN_POINT('Ctrl Pts',(-2.21965620168432,5.83494997235119,-1.01913911037994));
#47042=CARTESIAN_POINT('Ctrl Pts',(-0.259428722982098,5.92083970038001,
-1.1119288689567));
#47043=CARTESIAN_POINT('Ctrl Pts',(1.70079875572013,6.00672942840883,-1.20471862753345));
#47044=CARTESIAN_POINT('Ctrl Pts',(3.70791760499457,5.02243585007718,-1.29750838611021));
#47045=CARTESIAN_POINT('Ctrl Pts',(4.84018071389265,3.41998489423038,-1.39029814468697));
#47046=CARTESIAN_POINT('Ctrl Pts',(5.97244382279073,1.81753393838358,-1.48308790326372));
#47047=CARTESIAN_POINT('Ctrl Pts',(6.22985119131246,-0.403074394978366,
-1.57587766184048));
#47048=CARTESIAN_POINT('Ctrl Pts',(5.49419133515994,-2.22205031281952,-1.66866742041724));
#47049=CARTESIAN_POINT('Ctrl Pts',(4.75853147900741,-4.04102623066067,-1.76145717899399));
#47050=CARTESIAN_POINT('Ctrl Pts',(3.02980439818064,-5.45836973298102,-1.85424693757075));
#47051=CARTESIAN_POINT('Ctrl Pts',(1.10190886608084,-5.8231815076133,-1.9470366961475));
#47052=CARTESIAN_POINT('Ctrl Pts',(-0.825986666018957,-6.18799328224558,
-2.03982645472426));
#47053=CARTESIAN_POINT('Ctrl Pts',(-2.95305064939178,-5.50027332918978,
-2.13261621330102));
#47054=CARTESIAN_POINT('Ctrl Pts',(-4.30245249824173,-4.07584942315166,
-2.22540597187777));
#47055=CARTESIAN_POINT('Ctrl Pts',(-5.32634095342796,-2.99503632516554,
-2.29581225051688));
#47056=CARTESIAN_POINT('Ctrl Pts',(-5.90250203900672,-1.49007691941227,
-2.36621852915599));
#47057=CARTESIAN_POINT('Ctrl Pts',(-5.91623372814898,0.00546481507842006,
-2.4366248077951));
#47058=CARTESIAN_POINT('Ctrl Pts',(-5.90999536725745,0.0040860534926895,
-2.6883751922045));
#47059=CARTESIAN_POINT('Ctrl Pts',(-5.90198227594078,-1.26144439204732,
-2.62895606131706));
#47060=CARTESIAN_POINT('Ctrl Pts',(-5.50395911021358,-2.53157367164205,
-2.56953693042961));
#47061=CARTESIAN_POINT('Ctrl Pts',(-4.75359485550615,-3.53936198776295,
-2.51011779954216));
#47062=CARTESIAN_POINT('Ctrl Pts',(-3.58158563718193,-5.1134470927013,-2.41730984832646));
#47063=CARTESIAN_POINT('Ctrl Pts',(-1.55000676870931,-6.0475264269659,-2.32450189711075));
#47064=CARTESIAN_POINT('Ctrl Pts',(0.407826753663942,-5.91248041723304,
-2.23169394589504));
#47065=CARTESIAN_POINT('Ctrl Pts',(2.36566027603722,-5.77743440750018,-2.13888599467933));
#47066=CARTESIAN_POINT('Ctrl Pts',(4.24974845231112,-4.57326305376982,-2.04607804346362));
#47067=CARTESIAN_POINT('Ctrl Pts',(5.19453406473041,-2.85316722089178,-1.95327009224791));
#47068=CARTESIAN_POINT('Ctrl Pts',(6.13931967714968,-1.13307138801377,-1.8604621410322));
#47069=CARTESIAN_POINT('Ctrl Pts',(6.14480272571436,1.10294892401191,-1.76765418981649));
#47070=CARTESIAN_POINT('Ctrl Pts',(5.20846427759294,2.82765754785667,-1.67484623860078));
#47071=CARTESIAN_POINT('Ctrl Pts',(4.2721258294715,4.55236617170145,-1.58203828738507));
#47072=CARTESIAN_POINT('Ctrl Pts',(2.39396588466393,5.7657631073653,-1.48923033616936));
#47073=CARTESIAN_POINT('Ctrl Pts',(0.436818208133945,5.91040922390592,-1.39642238495365));
#47074=CARTESIAN_POINT('Ctrl Pts',(-1.52032946839601,6.05505534044654,-1.30361443373794));
#47075=CARTESIAN_POINT('Ctrl Pts',(-3.55646487664837,5.13095063786397,-1.21080648252223));
#47076=CARTESIAN_POINT('Ctrl Pts',(-4.73617972739577,3.56263230349625,-1.11799853130652));
#47077=CARTESIAN_POINT('Ctrl Pts',(-5.49726509383871,2.55084192596966,-1.05812408493918));
#47078=CARTESIAN_POINT('Ctrl Pts',(-5.90189954520199,1.27092330637285,-0.998249638571847));
#47079=CARTESIAN_POINT('Ctrl Pts',(-5.91020249175295,-0.00419241645486733,
-0.93837519220451));
#47080=CARTESIAN_POINT('Origin',(0.,0.,-10.));
#47081=CARTESIAN_POINT('',(-5.91957494766717,-0.0051333472841536,1.0633751922049));
#47082=CARTESIAN_POINT('',(-5.92528955248489,-0.00246218369985553,0.811624807795514));
#47083=CARTESIAN_POINT('',(-5.91675,-7.2459289488551E-16,-10.));
#47084=CARTESIAN_POINT('Ctrl Pts',(-5.91957494766717,-0.0051333472841536,
1.0633751922049));
#47085=CARTESIAN_POINT('Ctrl Pts',(-5.904918870215,1.59783527582977,0.987802148521663));
#47086=CARTESIAN_POINT('Ctrl Pts',(-5.23093422272582,3.21165545437413,0.912229104838426));
#47087=CARTESIAN_POINT('Ctrl Pts',(-4.0690788967531,4.308856339207,0.836656061155188));
#47088=CARTESIAN_POINT('Ctrl Pts',(-2.64253485480606,5.65601665261946,0.743866302578431));
#47089=CARTESIAN_POINT('Ctrl Pts',(-0.480510622894167,6.2243573463337,0.651076544001675));
#47090=CARTESIAN_POINT('Ctrl Pts',(1.4241081059804,5.75287424879129,0.558286785424919));
#47091=CARTESIAN_POINT('Ctrl Pts',(3.32872683485496,5.28139115124888,0.465497026848162));
#47092=CARTESIAN_POINT('Ctrl Pts',(4.97594006069217,3.77008426244976,0.372707268271405));
#47093=CARTESIAN_POINT('Ctrl Pts',(5.60928334562095,1.91300453958267,0.279917509694649));
#47094=CARTESIAN_POINT('Ctrl Pts',(6.24262663054972,0.0559248167155829,
0.187127751117892));
#47095=CARTESIAN_POINT('Ctrl Pts',(5.8620999745701,-2.1469277402195,0.0943379925411347));
#47096=CARTESIAN_POINT('Ctrl Pts',(4.64245603167641,-3.6839174819585,0.00154823396437833));
#47097=CARTESIAN_POINT('Ctrl Pts',(3.42281208878272,-5.2209072236975,-0.0912415246123782));
#47098=CARTESIAN_POINT('Ctrl Pts',(1.36405085897497,-6.09203415024043,-0.184031283189133));
#47099=CARTESIAN_POINT('Ctrl Pts',(-0.588364355247926,-5.89724286471199,
-0.27682104176589));
#47100=CARTESIAN_POINT('Ctrl Pts',(-2.54077956947082,-5.70245157918356,
-0.369610800342646));
#47101=CARTESIAN_POINT('Ctrl Pts',(-4.38684876810885,-4.44174208158375,
-0.462400558919404));
#47102=CARTESIAN_POINT('Ctrl Pts',(-5.27878510929411,-2.69408125152443,
-0.55519031749616));
#47103=CARTESIAN_POINT('Ctrl Pts',(-5.69992066053354,-1.86890789210222,
-0.599001814262474));
#47104=CARTESIAN_POINT('Ctrl Pts',(-5.90834766352312,-0.935176578526429,
-0.642813311028787));
#47105=CARTESIAN_POINT('Ctrl Pts',(-5.90707267146128,-0.000907514317987079,
-0.6866248077951));
#47106=CARTESIAN_POINT('Ctrl Pts',(-5.91020249175295,-0.00419241645486733,
-0.93837519220451));
#47107=CARTESIAN_POINT('Ctrl Pts',(-5.91476946726725,-0.705560569111268,
-0.905441687356137));
#47108=CARTESIAN_POINT('Ctrl Pts',(-5.79942752644688,-1.40547561965529,
-0.872508182507763));
#47109=CARTESIAN_POINT('Ctrl Pts',(-5.55753998903547,-2.05851806168967,
-0.839574677659389));
#47110=CARTESIAN_POINT('Ctrl Pts',(-4.87589110668532,-3.8988181263549,-0.74676672644368));
#47111=CARTESIAN_POINT('Ctrl Pts',(-3.18929904874264,-5.36688628953246,
-0.653958775227971));
#47112=CARTESIAN_POINT('Ctrl Pts',(-1.27259057030329,-5.78828649780727,
-0.561150824012261));
#47113=CARTESIAN_POINT('Ctrl Pts',(0.644117908136064,-6.20968670608207,
-0.468342872796551));
#47114=CARTESIAN_POINT('Ctrl Pts',(2.79094280707207,-5.58441895945409,-0.375534921580841));
#47115=CARTESIAN_POINT('Ctrl Pts',(4.18162466770078,-4.19973361996379,-0.28272697036513));
#47116=CARTESIAN_POINT('Ctrl Pts',(5.57230652832947,-2.8150482804735,-0.189919019149421));
#47117=CARTESIAN_POINT('Ctrl Pts',(6.2068453506509,-0.670945348120922,-0.0971110679337112));
#47118=CARTESIAN_POINT('Ctrl Pts',(5.79373160551071,1.24756620004122,-0.00430311671800236));
#47119=CARTESIAN_POINT('Ctrl Pts',(5.3806178603705,3.16607774820339,0.088504834497708));
#47120=CARTESIAN_POINT('Ctrl Pts',(3.91985154776864,4.85899791217512,0.181312785713418));
#47121=CARTESIAN_POINT('Ctrl Pts',(2.08251422334955,5.54859278103609,0.274120736929129));
#47122=CARTESIAN_POINT('Ctrl Pts',(0.245176898930466,6.23818764989705,0.366928688144839));
#47123=CARTESIAN_POINT('Ctrl Pts',(-1.96873143730581,5.92445722364727,0.459736639360548));
#47124=CARTESIAN_POINT('Ctrl Pts',(-3.54213294235917,4.75153044385172,0.552544590576258));
#47125=CARTESIAN_POINT('Ctrl Pts',(-5.00622159123967,3.66009333847765,0.638904662982677));
#47126=CARTESIAN_POINT('Ctrl Pts',(-5.91571084630785,1.82469886427711,0.725264735389096));
#47127=CARTESIAN_POINT('Ctrl Pts',(-5.92528955248489,-0.00246218369985553,
0.811624807795514));
#47128=CARTESIAN_POINT('Origin',(0.,0.,-10.));
#47129=CARTESIAN_POINT('',(-5.92405509285564,0.0034173886458154,2.81337519220491));
#47130=CARTESIAN_POINT('',(-5.91775768435869,0.00540196786531037,2.5616248077955));
#47131=CARTESIAN_POINT('',(-5.91675,-7.2459289488551E-16,-10.));
#47132=CARTESIAN_POINT('Ctrl Pts',(-5.92405509285564,0.0034173886458154,
2.81337519220491));
#47133=CARTESIAN_POINT('Ctrl Pts',(-5.92541887861536,0.20194281602732,2.80399712522563));
#47134=CARTESIAN_POINT('Ctrl Pts',(-5.91630780139426,0.40034155480686,2.79461905824635));
#47135=CARTESIAN_POINT('Ctrl Pts',(-5.89631038710755,0.597636878725663,
2.78524099126707));
#47136=CARTESIAN_POINT('Ctrl Pts',(-5.69844922361589,2.54974337521345,2.69245123269031));
#47137=CARTESIAN_POINT('Ctrl Pts',(-4.43483839204534,4.39382786076265,2.59966147411355));
#47138=CARTESIAN_POINT('Ctrl Pts',(-2.68577717751512,5.28301495101653,2.5068717155368));
#47139=CARTESIAN_POINT('Ctrl Pts',(-0.936715962984878,6.17220204127042,
2.41408195696004));
#47140=CARTESIAN_POINT('Ctrl Pts',(1.29779563450503,6.10649173622901,2.32129219838329));
#47141=CARTESIAN_POINT('Ctrl Pts',(2.99158290180955,5.11606076601189,2.22850243980653));
#47142=CARTESIAN_POINT('Ctrl Pts',(4.68537016911407,4.12562979579476,2.13571268122977));
#47143=CARTESIAN_POINT('Ctrl Pts',(5.83843310623318,2.21047816040193,2.04292292265302));
#47144=CARTESIAN_POINT('Ctrl Pts',(5.92124032471242,0.250118045980118,1.95013316407626));
#47145=CARTESIAN_POINT('Ctrl Pts',(6.00404754319166,-1.71024206844168,1.85734340549951));
#47146=CARTESIAN_POINT('Ctrl Pts',(5.01659904303105,-3.71581066189244,1.76455364692275));
#47147=CARTESIAN_POINT('Ctrl Pts',(3.41236961600884,-4.84555256123232,1.67176388834599));
#47148=CARTESIAN_POINT('Ctrl Pts',(1.80814018898661,-5.97529446057221,1.57897412976924));
#47149=CARTESIAN_POINT('Ctrl Pts',(-0.412870164897221,-6.2292096658012,
1.48618437119248));
#47150=CARTESIAN_POINT('Ctrl Pts',(-2.23068702915303,-5.4906904299818,1.39339461261573));
#47151=CARTESIAN_POINT('Ctrl Pts',(-4.04850389340885,-4.7521711941624,1.30060485403897));
#47152=CARTESIAN_POINT('Ctrl Pts',(-5.46312726803664,-3.02121751729461,
1.20781509546221));
#47153=CARTESIAN_POINT('Ctrl Pts',(-5.82490702935946,-1.09275071230537,
1.11502533688545));
#47154=CARTESIAN_POINT('Ctrl Pts',(-5.89203360777153,-0.734932525553136,
1.09780862199194));
#47155=CARTESIAN_POINT('Ctrl Pts',(-5.92291383008679,-0.370314533886649,
1.08059190709842));
#47156=CARTESIAN_POINT('Ctrl Pts',(-5.91957494766717,-0.0051333472841536,
1.0633751922049));
#47157=CARTESIAN_POINT('Ctrl Pts',(-5.92528955248489,-0.00246218369985553,
0.811624807795514));
#47158=CARTESIAN_POINT('Ctrl Pts',(-5.92600472484242,-0.138883016546891,
0.818072686604806));
#47159=CARTESIAN_POINT('Ctrl Pts',(-5.92170332485837,-0.275257951967435,
0.824520565414098));
#47160=CARTESIAN_POINT('Ctrl Pts',(-5.91224163087656,-0.411273921283423,
0.830968444223389));
#47161=CARTESIAN_POINT('Ctrl Pts',(-5.77605414047018,-2.36902837328162,
0.923776395439099));
#47162=CARTESIAN_POINT('Ctrl Pts',(-4.57078448578703,-4.25241414393666,
1.01658434665481));
#47163=CARTESIAN_POINT('Ctrl Pts',(-2.85013809380902,-5.19619670397703,
1.10939229787052));
#47164=CARTESIAN_POINT('Ctrl Pts',(-1.129491701831,-6.13997926401741,1.20220024908623));
#47165=CARTESIAN_POINT('Ctrl Pts',(1.1065314274419,-6.14415861344309,1.29500820030194));
#47166=CARTESIAN_POINT('Ctrl Pts',(2.83069383164873,-5.20681474335945,1.38781615151765));
#47167=CARTESIAN_POINT('Ctrl Pts',(4.55485623585553,-4.26947087327583,1.48062410273336));
#47168=CARTESIAN_POINT('Ctrl Pts',(5.7671579149963,-2.3906037836829,1.57343205394907));
#47169=CARTESIAN_POINT('Ctrl Pts',(5.91066290352019,-0.433372104721073,
1.66624000516478));
#47170=CARTESIAN_POINT('Ctrl Pts',(6.05416789204407,1.5238595742408,1.75904795638049));
#47171=CARTESIAN_POINT('Ctrl Pts',(5.12887618995105,3.55945584257158,1.8518559075962));
#47172=CARTESIAN_POINT('Ctrl Pts',(3.55987029641463,4.73825609406093,1.94466385881191));
#47173=CARTESIAN_POINT('Ctrl Pts',(1.99086440287824,5.91705634555026,2.03747181002762));
#47174=CARTESIAN_POINT('Ctrl Pts',(-0.221855682101526,6.23906058019818,
2.13027976124333));
#47175=CARTESIAN_POINT('Ctrl Pts',(-2.06175800263737,5.55633883764849,2.22308771245903));
#47176=CARTESIAN_POINT('Ctrl Pts',(-3.90166032317325,4.87361709509879,2.31589566367475));
#47177=CARTESIAN_POINT('Ctrl Pts',(-5.36874487926518,3.18616937535148,2.40870361489046));
#47178=CARTESIAN_POINT('Ctrl Pts',(-5.78902749036571,1.26921552779285,2.50151156610617));
#47179=CARTESIAN_POINT('Ctrl Pts',(-5.87976881819363,0.855334646409641,
2.52154931333595));
#47180=CARTESIAN_POINT('Ctrl Pts',(-5.92171327919293,0.430755294309258,
2.54158706056572));
#47181=CARTESIAN_POINT('Ctrl Pts',(-5.91775768435869,0.00540196786531037,
2.5616248077955));
#47182=CARTESIAN_POINT('Origin',(0.,0.,-10.));
#47183=CARTESIAN_POINT('',(-5.90893794266972,0.00341325037688023,4.5633751922049));
#47184=CARTESIAN_POINT('',(-5.90693841009768,-4.21682523413384E-5,4.31162480779551));
#47185=CARTESIAN_POINT('',(-5.91675,-7.2459289488551E-16,-10.));
#47186=CARTESIAN_POINT('Ctrl Pts',(-5.90893794266972,0.00341325037688023,
4.5633751922049));
#47187=CARTESIAN_POINT('Ctrl Pts',(-5.91294750478057,0.769920258362169,
4.52740234335283));
#47188=CARTESIAN_POINT('Ctrl Pts',(-5.77459382265735,1.53503581594222,4.49142949450076));
#47189=CARTESIAN_POINT('Ctrl Pts',(-5.48717594814371,2.23931822973835,4.45545664564868));
#47190=CARTESIAN_POINT('Ctrl Pts',(-4.74579915876471,4.05597154554143,4.36266688707193));
#47191=CARTESIAN_POINT('Ctrl Pts',(-3.01262316590221,5.46787129455723,4.26987712849517));
#47192=CARTESIAN_POINT('Ctrl Pts',(-1.0835898565008,5.8266181480181,4.17708736991841));
#47193=CARTESIAN_POINT('Ctrl Pts',(0.845443452900566,6.18536500147897,4.08429761134166));
#47194=CARTESIAN_POINT('Ctrl Pts',(2.97033407884086,5.49095895938497,3.9915078527649));
#47195=CARTESIAN_POINT('Ctrl Pts',(4.31524952575888,4.06229830888417,3.89871809418815));
#47196=CARTESIAN_POINT('Ctrl Pts',(5.6601649726769,2.63363765838336,3.80592833561139));
#47197=CARTESIAN_POINT('Ctrl Pts',(6.22510524057266,0.470722399475758,3.71313857703463));
#47198=CARTESIAN_POINT('Ctrl Pts',(5.75062776579904,-1.43315258055328,3.62034881845788));
#47199=CARTESIAN_POINT('Ctrl Pts',(5.27615029102541,-3.33702756058232,3.52755905988112));
#47200=CARTESIAN_POINT('Ctrl Pts',(3.76225507358237,-4.98186226173277,3.43476930130436));
#47201=CARTESIAN_POINT('Ctrl Pts',(1.90418173193351,-5.61228455726329,3.34197954272761));
#47202=CARTESIAN_POINT('Ctrl Pts',(0.046108390284639,-6.24270685279381,
3.24918978415085));
#47203=CARTESIAN_POINT('Ctrl Pts',(-2.15614307557003,-5.85871674270441,
3.1564000255741));
#47204=CARTESIAN_POINT('Ctrl Pts',(-3.691213060791,-4.63665743394649,3.06361026699734));
#47205=CARTESIAN_POINT('Ctrl Pts',(-5.07113673072789,-3.53810910555936,
2.98019857539986));
#47206=CARTESIAN_POINT('Ctrl Pts',(-5.91192512220749,-1.76233473912115,
2.89678688380238));
#47207=CARTESIAN_POINT('Ctrl Pts',(-5.92405509285564,0.0034173886458154,
2.81337519220491));
#47208=CARTESIAN_POINT('Ctrl Pts',(-5.91775768435869,0.00540196786531037,
2.5616248077955));
#47209=CARTESIAN_POINT('Ctrl Pts',(-5.90339232483635,-1.53933497169563,
2.63439501178143));
#47210=CARTESIAN_POINT('Ctrl Pts',(-5.28365457365082,-3.09427980078845,
2.70716521576736));
#47211=CARTESIAN_POINT('Ctrl Pts',(-4.19729483461209,-4.18407258679137,
2.77993541975329));
#47212=CARTESIAN_POINT('Ctrl Pts',(-2.81179890164883,-5.5739468784471,2.872743370969));
#47213=CARTESIAN_POINT('Ctrl Pts',(-0.66732636961311,-6.20723548638865,
2.96555132218472));
#47214=CARTESIAN_POINT('Ctrl Pts',(1.25094398893609,-5.79300323465687,3.05835927340043));
#47215=CARTESIAN_POINT('Ctrl Pts',(3.16921434748529,-5.37877098292509,3.15116722461614));
#47216=CARTESIAN_POINT('Ctrl Pts',(4.86128253254801,-3.91701787152002,3.24397517583184));
#47217=CARTESIAN_POINT('Ctrl Pts',(5.54980603553847,-2.07927879518383,3.33678312704755));
#47218=CARTESIAN_POINT('Ctrl Pts',(6.23832953852894,-0.241539718847621,
3.42959107826326));
#47219=CARTESIAN_POINT('Ctrl Pts',(5.9233083594471,1.9721853224197,3.52239902947898));
#47220=CARTESIAN_POINT('Ctrl Pts',(4.74946441657433,3.54490269202056,3.61520698069469));
#47221=CARTESIAN_POINT('Ctrl Pts',(3.57562047370158,5.11762006162138,3.7080149319104));
#47222=CARTESIAN_POINT('Ctrl Pts',(1.5429537670379,6.04932975955577,3.8008228831261));
#47223=CARTESIAN_POINT('Ctrl Pts',(-0.414720948889979,5.91200083514474,
3.89363083434181));
#47224=CARTESIAN_POINT('Ctrl Pts',(-2.37239566481789,5.77467191073371,3.98643878555752));
#47225=CARTESIAN_POINT('Ctrl Pts',(-4.25507839001002,4.56830436397723,4.07924673677324));
#47226=CARTESIAN_POINT('Ctrl Pts',(-5.19785757693449,2.84710799761883,4.17205468798895));
#47227=CARTESIAN_POINT('Ctrl Pts',(-5.67046005817503,1.98429549101611,4.2185780612578));
#47228=CARTESIAN_POINT('Ctrl Pts',(-5.90687591097582,0.992112598863517,
4.26510143452666));
#47229=CARTESIAN_POINT('Ctrl Pts',(-5.90693872189066,-4.21669123174065E-5,
4.31162480779551));
#47230=CARTESIAN_POINT('Origin',(0.,0.,-10.));
#47231=CARTESIAN_POINT('',(-5.91154939285259,-0.00474152141923923,6.31337519220491));
#47232=CARTESIAN_POINT('',(-5.91791297517326,-0.00538731180401663,6.0616248077955));
#47233=CARTESIAN_POINT('',(-5.91675,-7.2459289488551E-16,-10.));
#47234=CARTESIAN_POINT('Ctrl Pts',(-5.91154939285259,-0.00474152141923923,
6.31337519220491));
#47235=CARTESIAN_POINT('Ctrl Pts',(-5.90158645275689,1.3269665387579,6.25080756148004));
#47236=CARTESIAN_POINT('Ctrl Pts',(-5.45650196275694,2.66470719166618,6.18823993075516));
#47237=CARTESIAN_POINT('Ctrl Pts',(-4.63084737129029,3.69849951246977,6.12567230003029));
#47238=CARTESIAN_POINT('Ctrl Pts',(-3.40637571841808,5.23164594545016,6.03288254145354));
#47239=CARTESIAN_POINT('Ctrl Pts',(-1.34488502739145,6.09629388207883,5.94009278287678));
#47240=CARTESIAN_POINT('Ctrl Pts',(0.606907924444632,5.89536332986964,5.84730302430003));
#47241=CARTESIAN_POINT('Ctrl Pts',(2.55870087628076,5.69443277766045,5.75451326572327));
#47242=CARTESIAN_POINT('Ctrl Pts',(4.40079608892635,4.42792373661338,5.66172350714651));
#47243=CARTESIAN_POINT('Ctrl Pts',(5.28723172958268,2.677466462464,5.56893374856975));
#47244=CARTESIAN_POINT('Ctrl Pts',(6.17366737023899,0.927009188314677,5.476143989993));
#47245=CARTESIAN_POINT('Ctrl Pts',(6.10444343890609,-1.30739631893691,5.38335423141625));
#47246=CARTESIAN_POINT('Ctrl Pts',(5.11135025967902,-2.99962406691314,5.29056447283949));
#47247=CARTESIAN_POINT('Ctrl Pts',(4.11825708045197,-4.69185181488935,5.19777471426274));
#47248=CARTESIAN_POINT('Ctrl Pts',(2.20129465333077,-5.84190180359021,5.10498495568598));
#47249=CARTESIAN_POINT('Ctrl Pts',(0.240806750516323,-5.9216263077664,5.01219519710923));
#47250=CARTESIAN_POINT('Ctrl Pts',(-1.71968115229822,-6.00135081194258,
4.91940543853247));
#47251=CARTESIAN_POINT('Ctrl Pts',(-3.72369453080605,-5.01074983159395,
4.82661567995571));
#47252=CARTESIAN_POINT('Ctrl Pts',(-4.85091242711216,-3.40474590012443,
4.73382592137895));
#47253=CARTESIAN_POINT('Ctrl Pts',(-5.54112908934749,-2.42135956750124,
4.67700901165427));
#47254=CARTESIAN_POINT('Ctrl Pts',(-5.90260508509081,-1.20723758395451,
4.62019210192958));
#47255=CARTESIAN_POINT('Ctrl Pts',(-5.90893794266972,0.00341325037688023,
4.5633751922049));
#47256=CARTESIAN_POINT('Ctrl Pts',(-5.90693872189066,-4.21669123174065E-5,
4.31162480779551));
#47257=CARTESIAN_POINT('Ctrl Pts',(-5.90700121040943,-0.987104397471501,
4.35790938574237));
#47258=CARTESIAN_POINT('Ctrl Pts',(-5.67313073749119,-1.97413878964724,
4.40419396368922));
#47259=CARTESIAN_POINT('Ctrl Pts',(-5.20516343906184,-2.83372915305156,
4.45047854163608));
#47260=CARTESIAN_POINT('Ctrl Pts',(-4.26681446560791,-4.55734475140324,
4.54328649285178));
#47261=CARTESIAN_POINT('Ctrl Pts',(-2.38724087004325,-5.76855076214631,
4.6360944440675));
#47262=CARTESIAN_POINT('Ctrl Pts',(-0.429925854017753,-5.91091457392572,
4.72890239528321));
#47263=CARTESIAN_POINT('Ctrl Pts',(1.52738916200774,-6.05327838570513,4.82171034649892));
#47264=CARTESIAN_POINT('Ctrl Pts',(3.56244559849406,-5.12679999852089,4.91451829771462));
#47265=CARTESIAN_POINT('Ctrl Pts',(4.74033085001728,-3.55710707915503,5.00732624893033));
#47266=CARTESIAN_POINT('Ctrl Pts',(5.9182161015405,-1.98741415978915,5.10013420014604));
#47267=CARTESIAN_POINT('Ctrl Pts',(6.23893016810059,0.22549329175838,5.19294215136175));
#47268=CARTESIAN_POINT('Ctrl Pts',(5.55513579742875,2.06499724269212,5.28575010257746));
#47269=CARTESIAN_POINT('Ctrl Pts',(4.87134142675691,3.90450119362583,5.37855805379317));
#47270=CARTESIAN_POINT('Ctrl Pts',(3.18303861885318,5.37060164394576,5.47136600500888));
#47271=CARTESIAN_POINT('Ctrl Pts',(1.26584005382931,5.7897665150092,5.56417395622459));
#47272=CARTESIAN_POINT('Ctrl Pts',(-0.651358511194623,6.20893138607266,
5.6569819074403));
#47273=CARTESIAN_POINT('Ctrl Pts',(-2.79745283333869,5.58116067787958,5.74978985865602));
#47274=CARTESIAN_POINT('Ctrl Pts',(-4.18651908354902,4.19485462242498,5.84259780987173));
#47275=CARTESIAN_POINT('Ctrl Pts',(-5.27925236309908,3.10429269839319,5.91560680917965));
#47276=CARTESIAN_POINT('Ctrl Pts',(-5.90350202906922,1.54431438983364,5.98861580848757));
#47277=CARTESIAN_POINT('Ctrl Pts',(-5.91791297517326,-0.00538731180401663,
6.0616248077955));
#47278=CARTESIAN_POINT('Origin',(0.,0.,-10.));
#47279=CARTESIAN_POINT('',(-5.92610585757929,-0.00142481640334258,8.06337519220491));
#47280=CARTESIAN_POINT('',(-5.92520251234299,0.00254533425411539,7.81162480779552));
#47281=CARTESIAN_POINT('',(-5.91675,-7.2459289488551E-16,-10.));
#47282=CARTESIAN_POINT('Ctrl Pts',(-5.92610585757929,-0.00142481640334258,
8.06337519220491));
#47283=CARTESIAN_POINT('Ctrl Pts',(-5.92000527951757,1.88433477380826,7.97421277960724));
#47284=CARTESIAN_POINT('Ctrl Pts',(-4.94203695946198,3.77553572286442,7.88505036700958));
#47285=CARTESIAN_POINT('Ctrl Pts',(-3.39711376542502,4.85626029828357,7.79588795441191));
#47286=CARTESIAN_POINT('Ctrl Pts',(-1.78933930062697,5.98095140431731,7.70309819583515));
#47287=CARTESIAN_POINT('Ctrl Pts',(0.43245861786239,6.22788040808508,7.6103084372584));
#47288=CARTESIAN_POINT('Ctrl Pts',(2.24794389322745,5.48364789832706,7.51751867868164));
#47289=CARTESIAN_POINT('Ctrl Pts',(4.0634291685925,4.73941538856904,7.42472892010489));
#47290=CARTESIAN_POINT('Ctrl Pts',(5.47260180083323,3.00402136528525,7.33193916152813));
#47291=CARTESIAN_POINT('Ctrl Pts',(5.82831485936943,1.07442632133564,7.23914940295137));
#47292=CARTESIAN_POINT('Ctrl Pts',(6.18402791790564,-0.855168722614004,
7.14635964437462));
#47293=CARTESIAN_POINT('Ctrl Pts',(5.48628140273722,-2.97896478722948,7.05356988579786));
#47294=CARTESIAN_POINT('Ctrl Pts',(4.05550767628976,-4.32163204212022,6.9607801272211));
#47295=CARTESIAN_POINT('Ctrl Pts',(2.6247339498423,-5.66429929701095,6.86799036864435));
#47296=CARTESIAN_POINT('Ctrl Pts',(0.460933012115797,-6.22583774217698,
6.77520061006759));
#47297=CARTESIAN_POINT('Ctrl Pts',(-1.44219351141203,-5.74836706339865,
6.68241085149083));
#47298=CARTESIAN_POINT('Ctrl Pts',(-3.34532003493986,-5.27089638462031,
6.58962109291407));
#47299=CARTESIAN_POINT('Ctrl Pts',(-4.987772144269,-3.75441658189762,6.49683133433732));
#47300=CARTESIAN_POINT('Ctrl Pts',(-5.61527189157466,-1.8953542158702,6.40404157576057));
#47301=CARTESIAN_POINT('Ctrl Pts',(-5.81965196412772,-1.28984751585831,
6.37381944790868));
#47302=CARTESIAN_POINT('Ctrl Pts',(-5.91636180537109,-0.647998278783763,
6.34359732005679));
#47303=CARTESIAN_POINT('Ctrl Pts',(-5.91154939285259,-0.00474152141923923,
6.31337519220491));
#47304=CARTESIAN_POINT('Ctrl Pts',(-5.91791297517326,-0.00538731180401663,
6.0616248077955));
#47305=CARTESIAN_POINT('Ctrl Pts',(-5.92182100886177,-0.425643304256778,
6.08142375970328));
#47306=CARTESIAN_POINT('Ctrl Pts',(-5.880880678592,-0.84514354114256,6.10122271161106));
#47307=CARTESIAN_POINT('Ctrl Pts',(-5.79227289452576,-1.25432135258176,
6.12102166351885));
#47308=CARTESIAN_POINT('Ctrl Pts',(-5.37692227701563,-3.17234986941806,
6.21382961473456));
#47309=CARTESIAN_POINT('Ctrl Pts',(-3.9141828637187,-4.86356550037465,6.30663756595028));
#47310=CARTESIAN_POINT('Ctrl Pts',(-2.07604266018777,-5.55101740343884,
6.39944551716599));
#47311=CARTESIAN_POINT('Ctrl Pts',(-0.237902456656868,-6.23846930650301,
6.4922534683817));
#47312=CARTESIAN_POINT('Ctrl Pts',(1.97563853710807,-5.92215748167482,6.58506141959739));
#47313=CARTESIAN_POINT('Ctrl Pts',(3.54767123662648,-4.74739677476125,6.6778693708131));
#47314=CARTESIAN_POINT('Ctrl Pts',(5.11970393614489,-3.57263606784768,6.77067732202881));
#47315=CARTESIAN_POINT('Ctrl Pts',(6.05022834141679,-1.53942647884874,6.86348527324453));
#47316=CARTESIAN_POINT('Ctrl Pts',(5.91175802968461,0.418167835515719,6.95629322446024));
#47317=CARTESIAN_POINT('Ctrl Pts',(5.77328771795243,2.37576214988019,7.04910117567596));
#47318=CARTESIAN_POINT('Ctrl Pts',(4.56582268921612,4.25774118961017,7.14190912689166));
#47319=CARTESIAN_POINT('Ctrl Pts',(2.84407693358168,5.19951668293015,7.23471707810737));
#47320=CARTESIAN_POINT('Ctrl Pts',(1.12233117794723,6.14129217625015,7.32752502932308));
#47321=CARTESIAN_POINT('Ctrl Pts',(-1.11369530458533,6.14286412316017,7.42033298053879));
#47322=CARTESIAN_POINT('Ctrl Pts',(-2.83676351115532,5.2035103653186,7.5131409317545));
#47323=CARTESIAN_POINT('Ctrl Pts',(-4.55983171772526,4.26415660747706,7.60594888297021));
#47324=CARTESIAN_POINT('Ctrl Pts',(-5.76994164833263,2.38387714488395,7.69875683418592));
#47325=CARTESIAN_POINT('Ctrl Pts',(-5.91116423497235,0.426479457165389,
7.79156478540163));
#47326=CARTESIAN_POINT('Ctrl Pts',(-5.92133911120299,0.285451880199395,
7.79825145953293));
#47327=CARTESIAN_POINT('Ctrl Pts',(-5.92596540705868,0.144023983524415,
7.80493813366422));
#47328=CARTESIAN_POINT('Ctrl Pts',(-5.92520251234299,0.00254533425411539,
7.81162480779552));
#47329=CARTESIAN_POINT('Origin',(0.,0.,-10.));
#47330=CARTESIAN_POINT('',(-5.91585872307276,0.00546062239083878,9.81337519220492));
#47331=CARTESIAN_POINT('',(-5.91009314746035,0.00413707980402536,9.5616248077955));
#47332=CARTESIAN_POINT('',(-5.91675,-7.2459289488551E-16,-10.));
#47333=CARTESIAN_POINT('Ctrl Pts',(-5.91585872307276,0.00546062239083878,
9.81337519220492));
#47334=CARTESIAN_POINT('Ctrl Pts',(-5.92031005889638,0.493404501843675,
9.79040775631121));
#47335=CARTESIAN_POINT('Ctrl Pts',(-5.86501686991171,0.9803530671637,9.7674403204175));
#47336=CARTESIAN_POINT('Ctrl Pts',(-5.74609214718014,1.45123087620132,9.7444728845238));
#47337=CARTESIAN_POINT('Ctrl Pts',(-5.2656294450248,3.35360423742296,9.65168312594704));
#47338=CARTESIAN_POINT('Ctrl Pts',(-3.74656880677743,4.99366969368778,9.55889336737027));
#47339=CARTESIAN_POINT('Ctrl Pts',(-1.88652201322028,5.61824534116842,9.46610360879351));
#47340=CARTESIAN_POINT('Ctrl Pts',(-0.0264752196631479,6.24282098864905,
9.37331385021676));
#47341=CARTESIAN_POINT('Ctrl Pts',(2.17455772920379,5.85190682734555,9.28052409164001));
#47342=CARTESIAN_POINT('Ctrl Pts',(3.70577681897754,4.6250258580741,9.18773433306326));
#47343=CARTESIAN_POINT('Ctrl Pts',(5.23699590875136,3.3981448888026,9.0949445744865));
#47344=CARTESIAN_POINT('Ctrl Pts',(6.09840113943194,1.33529711156315,9.00215481590974));
#47345=CARTESIAN_POINT('Ctrl Pts',(5.89440169534027,-0.616177469480281,
8.90936505733298));
#47346=CARTESIAN_POINT('Ctrl Pts',(5.6904022512486,-2.56765205052362,8.81657529875622));
#47347=CARTESIAN_POINT('Ctrl Pts',(4.42099813238473,-4.40775343537091,8.72378554017947));
#47348=CARTESIAN_POINT('Ctrl Pts',(2.66914912692053,-5.29143543456638,8.63099578160272));
#47349=CARTESIAN_POINT('Ctrl Pts',(0.917300121456278,-6.17511743376187,
8.53820602302596));
#47350=CARTESIAN_POINT('Ctrl Pts',(-1.31699377060835,-6.10238004730551,
8.44541626444921));
#47351=CARTESIAN_POINT('Ctrl Pts',(-3.00765781493459,-5.10662711466074,
8.35262650587245));
#47352=CARTESIAN_POINT('Ctrl Pts',(-4.69832185926076,-4.11087418201601,
8.25983674729569));
#47353=CARTESIAN_POINT('Ctrl Pts',(-5.84535605584862,-2.19210570318293,
8.16704698871894));
#47354=CARTESIAN_POINT('Ctrl Pts',(-5.92199764858924,-0.231494859616551,
8.07425723014218));
#47355=CARTESIAN_POINT('Ctrl Pts',(-5.924993728949,-0.154850475914561,8.07062988416309));
#47356=CARTESIAN_POINT('Ctrl Pts',(-5.9263540440814,-0.0781421490528213,
8.067002538184));
#47357=CARTESIAN_POINT('Ctrl Pts',(-5.92610585757929,-0.00142481640334258,
8.06337519220491));
#47358=CARTESIAN_POINT('Ctrl Pts',(-5.92520251234299,0.00254533425411539,
7.81162480779552));
#47359=CARTESIAN_POINT('Ctrl Pts',(-5.91537678046098,-1.81963437961978,
7.89774608487994));
#47360=CARTESIAN_POINT('Ctrl Pts',(-5.01157857549601,-3.65023306152754,
7.98386736196435));
#47361=CARTESIAN_POINT('Ctrl Pts',(-3.55434265269086,-4.74240399454357,
8.06998863904876));
#47362=CARTESIAN_POINT('Ctrl Pts',(-1.98396324109763,-5.91937384568984,
8.16279659026447));
#47363=CARTESIAN_POINT('Ctrl Pts',(0.229130824760936,-6.23879763513836,
8.25560454148017));
#47364=CARTESIAN_POINT('Ctrl Pts',(2.06823578077075,-5.55393086879374,8.34841249269589));
#47365=CARTESIAN_POINT('Ctrl Pts',(3.90734073678059,-4.86906410244912,8.44122044391159));
#47366=CARTESIAN_POINT('Ctrl Pts',(5.37245658294166,-3.1799067803114,8.53402839512731));
#47367=CARTESIAN_POINT('Ctrl Pts',(5.79050357147695,-1.26246414955556,8.62683634634302));
#47368=CARTESIAN_POINT('Ctrl Pts',(6.20855056001223,0.654978481200288,8.71964429755873));
#47369=CARTESIAN_POINT('Ctrl Pts',(5.57952869092166,2.80070642057423,8.81245224877443));
#47370=CARTESIAN_POINT('Ctrl Pts',(4.19241298423735,4.18896415713938,8.90526019999014));
#47371=CARTESIAN_POINT('Ctrl Pts',(2.80529727755305,5.57722189370453,8.99806815120585));
#47372=CARTESIAN_POINT('Ctrl Pts',(0.660087733274977,6.20800942746091,9.09087610242157));
#47373=CARTESIAN_POINT('Ctrl Pts',(-1.25769828983296,5.79154058536687,9.18368405363728));
#47374=CARTESIAN_POINT('Ctrl Pts',(-3.17548431294089,5.37507174327283,9.27649200485299));
#47375=CARTESIAN_POINT('Ctrl Pts',(-4.86584681487867,3.91134652532842,9.3692999560687));
#47376=CARTESIAN_POINT('Ctrl Pts',(-5.55222688432391,2.07280581946095,9.46210790728441));
#47377=CARTESIAN_POINT('Ctrl Pts',(-5.79755937358089,1.41565712291544,9.49528020745477));
#47378=CARTESIAN_POINT('Ctrl Pts',(-5.91462723191149,0.710623554415929,
9.52845250762514));
#47379=CARTESIAN_POINT('Ctrl Pts',(-5.91009314746035,0.00413707980402536,
9.5616248077955));
#47380=CARTESIAN_POINT('Origin',(0.,0.,-10.));
#47381=CARTESIAN_POINT('',(-5.90713571469763,-0.00111013332615595,11.5633751922049));
#47382=CARTESIAN_POINT('',(-5.91010328083002,-0.00414228348423679,11.3116248077955));
#47383=CARTESIAN_POINT('',(-5.91675,-7.2459289488551E-16,-10.));
#47384=CARTESIAN_POINT('Ctrl Pts',(-5.90713571469763,-0.00111013332615595,
11.5633751922049));
#47385=CARTESIAN_POINT('Ctrl Pts',(-5.90537029125798,1.05576347433266,11.5138129744384));
#47386=CARTESIAN_POINT('Ctrl Pts',(-5.63517675792205,2.11347947535037,11.4642507566719));
#47387=CARTESIAN_POINT('Ctrl Pts',(-5.10189134263591,3.01568412600891,11.4146885389054));
#47388=CARTESIAN_POINT('Ctrl Pts',(-4.10348111874248,4.70478028622991,11.3218987803286));
#47389=CARTESIAN_POINT('Ctrl Pts',(-2.18291133267984,5.8487958544671,11.2291090217519));
#47390=CARTESIAN_POINT('Ctrl Pts',(-0.222182396306169,5.92235434626272,
11.1363192631751));
#47391=CARTESIAN_POINT('Ctrl Pts',(1.73854654006744,5.99591283805835,11.0435295045984));
#47392=CARTESIAN_POINT('Ctrl Pts',(3.73943462675207,4.99901425341247,10.9507397460216));
#47393=CARTESIAN_POINT('Ctrl Pts',(4.86159616152291,3.38947323078248,10.8579499874449));
#47394=CARTESIAN_POINT('Ctrl Pts',(5.98375769629379,1.77993220815245,10.7651602288681));
#47395=CARTESIAN_POINT('Ctrl Pts',(6.22719267915082,-0.442251252461718,
10.6723704702913));
#47396=CARTESIAN_POINT('Ctrl Pts',(5.48010628925558,-2.25656399829182,10.5795807117146));
#47397=CARTESIAN_POINT('Ctrl Pts',(4.73301989936036,-4.07087674412186,10.4867909531378));
#47398=CARTESIAN_POINT('Ctrl Pts',(2.99541213671292,-5.47731877516786,10.3940011945611));
#47399=CARTESIAN_POINT('Ctrl Pts',(1.06526012946797,-5.82999715921811,10.3012114359843));
#47400=CARTESIAN_POINT('Ctrl Pts',(-0.864891877777048,-6.18267554326837,
10.2084216774076));
#47401=CARTESIAN_POINT('Ctrl Pts',(-2.98758812961958,-5.48159028032283,
10.1156319188308));
#47402=CARTESIAN_POINT('Ctrl Pts',(-4.3280038725092,-4.0487070157608,10.0228421602541));
#47403=CARTESIAN_POINT('Ctrl Pts',(-5.33663825161536,-2.97049279039852,
9.953019837571));
#47404=CARTESIAN_POINT('Ctrl Pts',(-5.90232640681047,-1.4779167628797,9.88319751488796));
#47405=CARTESIAN_POINT('Ctrl Pts',(-5.91585872307276,0.00546062239083878,
9.81337519220492));
#47406=CARTESIAN_POINT('Ctrl Pts',(-5.91009314746035,0.00413707980402536,
9.5616248077955));
#47407=CARTESIAN_POINT('Ctrl Pts',(-5.90194197685264,-1.26595214077577,
9.62126045884084));
#47408=CARTESIAN_POINT('Ctrl Pts',(-5.50078291561905,-2.54073703934775,
9.68089610988619));
#47409=CARTESIAN_POINT('Ctrl Pts',(-4.74532751911606,-3.55043857523549,
9.74053176093154));
#47410=CARTESIAN_POINT('Ctrl Pts',(-3.56965044751031,-5.12178607027405,
9.83333971214725));
#47411=CARTESIAN_POINT('Ctrl Pts',(-1.53589866734621,-6.05112486656059,
9.92614766336295));
#47412=CARTESIAN_POINT('Ctrl Pts',(0.421614579989387,-5.91151321457888,
10.0189556145787));
#47413=CARTESIAN_POINT('Ctrl Pts',(2.37912782732493,-5.77190156259718,10.1117635657944));
#47414=CARTESIAN_POINT('Ctrl Pts',(4.26040254183193,-4.56333946234723,10.2045715170101));
#47415=CARTESIAN_POINT('Ctrl Pts',(5.20117402139986,-2.84104490272778,10.2973794682258));
#47416=CARTESIAN_POINT('Ctrl Pts',(6.1419455009678,-1.11875034310833,10.3901874194415));
#47417=CARTESIAN_POINT('Ctrl Pts',(6.14221374559667,1.11727667588066,10.4829953706572));
#47418=CARTESIAN_POINT('Ctrl Pts',(5.20185552269185,2.83979690492835,10.5758033218729));
#47419=CARTESIAN_POINT('Ctrl Pts',(4.26149729978703,4.56231713397607,10.6686112730886));
#47420=CARTESIAN_POINT('Ctrl Pts',(2.38051260934848,5.77133057308248,10.7614192243043));
#47421=CARTESIAN_POINT('Ctrl Pts',(0.423032915335419,5.91141188657525,10.8542271755201));
#47422=CARTESIAN_POINT('Ctrl Pts',(-1.53444677867767,6.05149320006802,10.9470351267358));
#47423=CARTESIAN_POINT('Ctrl Pts',(-3.56842147626521,5.12264238794716,11.0398430779515));
#47424=CARTESIAN_POINT('Ctrl Pts',(-4.74447552693495,3.55157701796197,11.1326510291672));
#47425=CARTESIAN_POINT('Ctrl Pts',(-5.50045542794686,2.54167969036188,11.1923089553766));
#47426=CARTESIAN_POINT('Ctrl Pts',(-5.9019379291562,1.26641587263688,11.2519668815861));
#47427=CARTESIAN_POINT('Ctrl Pts',(-5.91010328083002,-0.00414228348423679,
11.3116248077955));
#47428=CARTESIAN_POINT('Origin',(0.,0.,-10.));
#47429=CARTESIAN_POINT('',(-5.91994540799989,-0.00505429986354111,13.3133751922049));
#47430=CARTESIAN_POINT('',(-5.92521073655459,-0.00253761243528721,13.0616248077955));
#47431=CARTESIAN_POINT('',(-5.91675,-7.2459289488551E-16,-10.));
#47432=CARTESIAN_POINT('Ctrl Pts',(-5.91994540799989,-0.00505429986354111,
13.3133751922049));
#47433=CARTESIAN_POINT('Ctrl Pts',(-5.90529546049876,1.610039595349,13.2372181925656));
#47434=CARTESIAN_POINT('Ctrl Pts',(-5.21966076773228,3.23607223700127,13.1610611929263));
#47435=CARTESIAN_POINT('Ctrl Pts',(-4.04189634411325,4.33436500117022,13.084904193287));
#47436=CARTESIAN_POINT('Ctrl Pts',(-2.606907084485,5.67252591765216,12.9921144347103));
#47437=CARTESIAN_POINT('Ctrl Pts',(-0.441350842398215,6.22725656027499,
12.8993246761335));
#47438=CARTESIAN_POINT('Ctrl Pts',(1.46026465257464,5.74380302276866,12.8065349175568));
#47439=CARTESIAN_POINT('Ctrl Pts',(3.36188014754744,5.26034948526234,12.71374515898));
#47440=CARTESIAN_POINT('Ctrl Pts',(4.99955489540633,3.73871176762691,12.6209554004032));
#47441=CARTESIAN_POINT('Ctrl Pts',(5.62120489869217,1.87768514582304,12.5281656418265));
#47442=CARTESIAN_POINT('Ctrl Pts',(6.24285490197803,0.0166585240191056,
12.4353758832497));
#47443=CARTESIAN_POINT('Ctrl Pts',(5.84848016069077,-2.18375700195329,12.342586124673));
#47444=CARTESIAN_POINT('Ctrl Pts',(4.61919290869249,-3.71304496232006,12.2497963660962));
#47445=CARTESIAN_POINT('Ctrl Pts',(3.38990565669422,-5.24233292268681,12.1570066075195));
#47446=CARTESIAN_POINT('Ctrl Pts',(1.32570589398494,-6.10049331744795,12.0642168489427));
#47447=CARTESIAN_POINT('Ctrl Pts',(-0.625445490911942,-5.89342548589725,
11.9714270903659));
#47448=CARTESIAN_POINT('Ctrl Pts',(-2.57659687580883,-5.68635765434655,
11.8786373317892));
#47449=CARTESIAN_POINT('Ctrl Pts',(-4.41469988289332,-4.41406159648403,
11.7858475732124));
#47450=CARTESIAN_POINT('Ctrl Pts',(-5.29562605557344,-2.66082519145039,
11.6930578146357));
#47451=CARTESIAN_POINT('Ctrl Pts',(-5.70601910610445,-1.84405295913638,
11.6498302738254));
#47452=CARTESIAN_POINT('Ctrl Pts',(-5.90867549474026,-0.922901955104379,
11.6066027330152));
#47453=CARTESIAN_POINT('Ctrl Pts',(-5.90713571469763,-0.00111013332615595,
11.5633751922049));
#47454=CARTESIAN_POINT('Ctrl Pts',(-5.91010328083002,-0.00414228348423679,
11.3116248077955));
#47455=CARTESIAN_POINT('Ctrl Pts',(-5.91464050881247,-0.710151314027206,
11.3447748328018));
#47456=CARTESIAN_POINT('Ctrl Pts',(-5.7977342302467,-1.41470738975629,11.377924857808));
#47457=CARTESIAN_POINT('Ctrl Pts',(-5.55272405215304,-2.07147361577248,
11.4110748828143));
#47458=CARTESIAN_POINT('Ctrl Pts',(-4.86678512294952,-3.91017895167227,
11.50388283403));
#47459=CARTESIAN_POINT('Ctrl Pts',(-3.17677386079062,-5.37430969562241,
11.5966907852457));
#47460=CARTESIAN_POINT('Ctrl Pts',(-1.25908781611912,-5.79123865951843,
11.6894987364614));
#47461=CARTESIAN_POINT('Ctrl Pts',(0.658598228552384,-6.20816762341444,
11.7823066876772));
#47462=CARTESIAN_POINT('Ctrl Pts',(2.80395905573648,-5.57789480725632,11.8751146388929));
#47463=CARTESIAN_POINT('Ctrl Pts',(4.19140780673151,-4.18996992087897,11.9679225901086));
#47464=CARTESIAN_POINT('Ctrl Pts',(5.57885655772655,-2.80204503450161,12.0607305413243));
#47465=CARTESIAN_POINT('Ctrl Pts',(6.2083932325325,-0.656468077904998,12.15353849254));
#47466=CARTESIAN_POINT('Ctrl Pts',(5.79080630742918,1.26107479954157,12.2463464437557));
#47467=CARTESIAN_POINT('Ctrl Pts',(5.37321938232585,3.17861767698814,12.3391543949714));
#47468=CARTESIAN_POINT('Ctrl Pts',(3.90850885731324,4.86812647528467,12.4319623461871));
#47469=CARTESIAN_POINT('Ctrl Pts',(2.06956827410354,5.5534344777826,12.5247702974028));
#47470=CARTESIAN_POINT('Ctrl Pts',(0.230627690893864,6.2387424802805,12.6175782486185));
#47471=CARTESIAN_POINT('Ctrl Pts',(-1.9825429505129,5.91984968697983,12.7103861998343));
#47472=CARTESIAN_POINT('Ctrl Pts',(-3.55320470690695,4.74325665034211,12.80319415105));
#47473=CARTESIAN_POINT('Ctrl Pts',(-5.01107961206679,3.65115298466299,12.8893377032985));
#47474=CARTESIAN_POINT('Ctrl Pts',(-5.91540774870406,1.8201067002357,12.975481255547));
#47475=CARTESIAN_POINT('Ctrl Pts',(-5.92521073655459,-0.00253761243528721,
13.0616248077955));
#47476=CARTESIAN_POINT('Origin',(0.,0.,-10.));
#47477=CARTESIAN_POINT('',(-5.92377318385666,0.00359036632908968,15.0633751922049));
#47478=CARTESIAN_POINT('',(-5.91789849188119,0.00538873909439685,14.8116248077955));
#47479=CARTESIAN_POINT('',(-5.91675,-7.2459289488551E-16,-10.));
#47480=CARTESIAN_POINT('Ctrl Pts',(-5.92377318385666,0.00359036632908968,
15.0633751922049));
#47481=CARTESIAN_POINT('Ctrl Pts',(-5.92527934221041,0.214504010083895,
15.0534131692696));
#47482=CARTESIAN_POINT('Ctrl Pts',(-5.91499513265657,0.425269163136507,
15.0434511463342));
#47483=CARTESIAN_POINT('Ctrl Pts',(-5.89243470395443,0.634711965822937,
15.0334891233989));
#47484=CARTESIAN_POINT('Ctrl Pts',(-5.68229899695524,2.58553533001874,14.9406993648221));
#47485=CARTESIAN_POINT('Ctrl Pts',(-4.40711414606309,4.42163541431722,14.8479096062454));
#47486=CARTESIAN_POINT('Ctrl Pts',(-2.65249467663608,5.29980358224176,14.7551198476686));
#47487=CARTESIAN_POINT('Ctrl Pts',(-0.897875207209115,6.17797175016628,
14.6623300890919));
#47488=CARTESIAN_POINT('Ctrl Pts',(1.33617888075265,6.0982080017169,14.5695403305151));
#47489=CARTESIAN_POINT('Ctrl Pts',(3.02370298028995,5.09714295531438,14.4767505719384));
#47490=CARTESIAN_POINT('Ctrl Pts',(4.71122707982726,4.09607790891186,14.3839608133616));
#47491=CARTESIAN_POINT('Ctrl Pts',(5.85222119094007,2.17371156455622,14.2911710547849));
#47492=CARTESIAN_POINT('Ctrl Pts',(5.92269639990486,0.212869383612165,14.1983812962081));
#47493=CARTESIAN_POINT('Ctrl Pts',(5.99317160886964,-1.74797279733192,14.1055915376314));
#47494=CARTESIAN_POINT('Ctrl Pts',(4.99312791568633,-3.74729081486445,14.0128017790546));
#47495=CARTESIAN_POINT('Ctrl Pts',(3.38182431508907,-4.86692000363656,13.9200120204778));
#47496=CARTESIAN_POINT('Ctrl Pts',(1.77052071449184,-5.98654919240866,13.8272222619011));
#47497=CARTESIAN_POINT('Ctrl Pts',(-0.452042793519305,-6.22648955242042,
13.7344325033243));
#47498=CARTESIAN_POINT('Ctrl Pts',(-2.26517852361662,-5.47655112968658,
13.6416427447476));
#47499=CARTESIAN_POINT('Ctrl Pts',(-4.07831425371399,-4.72661270695272,
13.5488529861708));
#47500=CARTESIAN_POINT('Ctrl Pts',(-5.48202220589748,-2.9867955014732,13.456063227594));
#47501=CARTESIAN_POINT('Ctrl Pts',(-5.83166504340434,-1.05609130356291,
13.3632734690173));
#47502=CARTESIAN_POINT('Ctrl Pts',(-5.89433925572756,-0.710008524644843,
13.3466407100798));
#47503=CARTESIAN_POINT('Ctrl Pts',(-5.92314497004129,-0.357792295683551,
13.3300079511424));
#47504=CARTESIAN_POINT('Ctrl Pts',(-5.91994540799989,-0.00505429986354111,
13.3133751922049));
#47505=CARTESIAN_POINT('Ctrl Pts',(-5.92521073655459,-0.00253761243528721,
13.0616248077955));
#47506=CARTESIAN_POINT('Ctrl Pts',(-5.92596913367662,-0.143544438342343,
13.0682892067627));
#47507=CARTESIAN_POINT('Ctrl Pts',(-5.92137364653565,-0.284500977027824,
13.0749536057299));
#47508=CARTESIAN_POINT('Ctrl Pts',(-5.91126638991079,-0.425061181139209,
13.0816180046971));
#47509=CARTESIAN_POINT('Ctrl Pts',(-5.7705134451392,-2.38249269600794,13.1744259559128));
#47510=CARTESIAN_POINT('Ctrl Pts',(-4.56085468421472,-4.26306244577067,
13.2672339071285));
#47511=CARTESIAN_POINT('Ctrl Pts',(-2.83801190608778,-5.20282959178026,
13.3600418583442));
#47512=CARTESIAN_POINT('Ctrl Pts',(-1.11516912796078,-6.14259673778988,
13.4528498095599));
#47513=CARTESIAN_POINT('Ctrl Pts',(1.12085766736865,-6.14156128004636,13.5456577607757));
#47514=CARTESIAN_POINT('Ctrl Pts',(2.84282933333981,-5.20019891174396,13.6384657119914));
#47515=CARTESIAN_POINT('Ctrl Pts',(4.56480099931093,-4.25883654344159,13.7312736632071));
#47516=CARTESIAN_POINT('Ctrl Pts',(5.77271753592375,-2.37714726458037,13.8240816144228));
#47517=CARTESIAN_POINT('Ctrl Pts',(5.91165752865023,-0.419586229699372,
13.9168895656385));
#47518=CARTESIAN_POINT('Ctrl Pts',(6.05059752137672,1.53797480518165,14.0096975168542));
#47519=CARTESIAN_POINT('Ctrl Pts',(5.12056097021688,3.57140759608242,14.1025054680699));
#47520=CARTESIAN_POINT('Ctrl Pts',(3.54881017590845,4.74654544648726,14.1953134192856));
#47521=CARTESIAN_POINT('Ctrl Pts',(1.97705938160005,5.92168329689209,14.2881213705013));
#47522=CARTESIAN_POINT('Ctrl Pts',(-0.236405655857032,6.23852620680096,
14.380929321717));
#47523=CARTESIAN_POINT('Ctrl Pts',(-2.0747107465965,5.55151534791694,14.4737372729327));
#47524=CARTESIAN_POINT('Ctrl Pts',(-3.91301583733602,4.8645044890329,14.5665452241485));
#47525=CARTESIAN_POINT('Ctrl Pts',(-5.37616098135797,3.17363986135601,14.6593531753642));
#47526=CARTESIAN_POINT('Ctrl Pts',(-5.79197177888372,1.25571105466782,14.7521611265799));
#47527=CARTESIAN_POINT('Ctrl Pts',(-5.88077753451924,0.846094185777964,
14.7719823536518));
#47528=CARTESIAN_POINT('Ctrl Pts',(-5.92181100139047,0.426120189229642,
14.7918035807236));
#47529=CARTESIAN_POINT('Ctrl Pts',(-5.91789849188119,0.00538873909439685,
14.8116248077955));
#47530=CARTESIAN_POINT('Origin',(0.,0.,-10.));
#47531=CARTESIAN_POINT('',(-5.9087266087589,0.0032487932499714,16.8133751922049));
#47532=CARTESIAN_POINT('',(-5.90693834692481,3.43012228386451E-5,16.5616248077955));
#47533=CARTESIAN_POINT('',(-5.91675,-7.2459289488551E-16,-10.));
#47534=CARTESIAN_POINT('Ctrl Pts',(-5.9087266087589,0.0032487932499714,
16.8133751922049));
#47535=CARTESIAN_POINT('Ctrl Pts',(-5.91259668880297,0.782268437741723,
16.7768183873968));
#47536=CARTESIAN_POINT('Ctrl Pts',(-5.7695619904093,1.55992356720195,16.7402615825886));
#47537=CARTESIAN_POINT('Ctrl Pts',(-5.47298242841067,2.27378744790129,16.7037047777805));
#47538=CARTESIAN_POINT('Ctrl Pts',(-4.72019382718881,4.08574167897852,16.6109150192038));
#47539=CARTESIAN_POINT('Ctrl Pts',(-2.97817148087205,5.4867120813921,16.518125260627));
#47540=CARTESIAN_POINT('Ctrl Pts',(-1.04691986629196,5.83331850780399,16.4253355020502));
#47541=CARTESIAN_POINT('Ctrl Pts',(0.884331748288081,6.17992493421588,16.3325457434735));
#47542=CARTESIAN_POINT('Ctrl Pts',(3.00481263113146,5.47216738462615,16.2397559848967));
#47543=CARTESIAN_POINT('Ctrl Pts',(4.34071541237453,4.0350756781874,16.14696622632));
#47544=CARTESIAN_POINT('Ctrl Pts',(5.67661819361766,2.59798397174859,16.0541764677432));
#47545=CARTESIAN_POINT('Ctrl Pts',(6.22794287326043,0.431558108460773,15.9613867091665));
#47546=CARTESIAN_POINT('Ctrl Pts',(5.74149969582441,-1.46929481819459,15.8685969505897));
#47547=CARTESIAN_POINT('Ctrl Pts',(5.25505651838841,-3.37014774484988,15.775807192013));
#47548=CARTESIAN_POINT('Ctrl Pts',(3.73084548387367,-5.0054277348727,15.6830174334362));
#47549=CARTESIAN_POINT('Ctrl Pts',(1.86884363552882,-5.62415055682801,15.5902276748594));
#47550=CARTESIAN_POINT('Ctrl Pts',(0.0068417871839091,-6.24287337878334,
15.4974379162827));
#47551=CARTESIAN_POINT('Ctrl Pts',(-2.19295087499116,-5.84503903267113,
15.4046481577059));
#47552=CARTESIAN_POINT('Ctrl Pts',(-3.72030392452555,-4.61334853756847,
15.3118583991292));
#47553=CARTESIAN_POINT('Ctrl Pts',(-5.08367846669871,-3.51389385328867,
15.2290306634878));
#47554=CARTESIAN_POINT('Ctrl Pts',(-5.9112504576224,-1.75001928117738,15.1462029278463));
#47555=CARTESIAN_POINT('Ctrl Pts',(-5.92377318385666,0.00359036632908968,
15.0633751922049));
#47556=CARTESIAN_POINT('Ctrl Pts',(-5.91789849188119,0.00538873909439685,
14.8116248077955));
#47557=CARTESIAN_POINT('Ctrl Pts',(-5.90349165161704,-1.54384987152742,
14.8846115319393));
#47558=CARTESIAN_POINT('Ctrl Pts',(-5.27966370824949,-3.10335877189863,
14.9575982560832));
#47559=CARTESIAN_POINT('Ctrl Pts',(-4.18752543318034,-4.19385003149471,
15.030584980227));
#47560=CARTESIAN_POINT('Ctrl Pts',(-2.79879183892172,-5.58048932526967,
15.1233929314427));
#47561=CARTESIAN_POINT('Ctrl Pts',(-0.652848199374933,-6.2087749271202,
15.2162008826584));
#47562=CARTESIAN_POINT('Ctrl Pts',(1.26445088055988,-5.79007006096228,15.3090088338741));
#47563=CARTESIAN_POINT('Ctrl Pts',(3.18174996049471,-5.37136519480435,15.4018167850898));
#47564=CARTESIAN_POINT('Ctrl Pts',(4.8704044808176,-3.90566986063792,15.4946247363055));
#47565=CARTESIAN_POINT('Ctrl Pts',(5.55464018340432,-2.06633002521627,15.5874326875213));
#47566=CARTESIAN_POINT('Ctrl Pts',(6.23887588599105,-0.226990189794622,
15.680240638737));
#47567=CARTESIAN_POINT('Ctrl Pts',(5.91869277084165,1.98599414688221,15.7730485899527));
#47568=CARTESIAN_POINT('Ctrl Pts',(4.74118416914349,3.55596963070039,15.8658565411684));
#47569=CARTESIAN_POINT('Ctrl Pts',(3.56367556744535,5.12594511451855,15.9586644923841));
#47570=CARTESIAN_POINT('Ctrl Pts',(1.52884147919836,6.05291174547805,16.0514724435998));
#47571=CARTESIAN_POINT('Ctrl Pts',(-0.428507637793467,5.91101755576424,
16.1442803948155));
#47572=CARTESIAN_POINT('Ctrl Pts',(-2.38585675478535,5.76912336605042,16.2370883460312));
#47573=CARTESIAN_POINT('Ctrl Pts',(-4.26572090052208,4.55836835566334,16.3298962972469));
#47574=CARTESIAN_POINT('Ctrl Pts',(-5.20448339350851,2.83497794469277,16.4227042484627));
#47575=CARTESIAN_POINT('Ctrl Pts',(-5.67288223541112,1.97508624825669,16.4690111015736));
#47576=CARTESIAN_POINT('Ctrl Pts',(-5.90698948598436,0.987571607557929,
16.5153179546846));
#47577=CARTESIAN_POINT('Ctrl Pts',(-5.90693863091242,3.43002300271205E-5,
16.5616248077955));
#47578=CARTESIAN_POINT('Origin',(0.,0.,-10.));
#47579=CARTESIAN_POINT('',(-5.91186200022437,-0.00484233898808362,18.5633751922049));
#47580=CARTESIAN_POINT('',(-5.91777217212816,-0.00540066091151231,18.3116248077955));
#47581=CARTESIAN_POINT('',(-5.91675,-7.2459289488551E-16,-10.));
#47582=CARTESIAN_POINT('Ctrl Pts',(-5.91186200022437,-0.00484233898808362,
18.5633751922049));
#47583=CARTESIAN_POINT('Ctrl Pts',(-5.90155532688764,1.33911565951482,18.500223605524));
#47584=CARTESIAN_POINT('Ctrl Pts',(-5.44739994873886,2.68937513445512,18.4370720188431));
#47585=CARTESIAN_POINT('Ctrl Pts',(-4.60749275915341,3.72755368764478,18.3739204321621));
#47586=CARTESIAN_POINT('Ctrl Pts',(-3.37340206651128,5.2529680497059,18.2811306735854));
#47587=CARTESIAN_POINT('Ctrl Pts',(-1.30651364845072,6.104632414813,18.1883409150086));
#47588=CARTESIAN_POINT('Ctrl Pts',(0.643976871300414,5.89142935196167,18.0955511564318));
#47589=CARTESIAN_POINT('Ctrl Pts',(2.59446739105152,5.67822628911034,18.0027613978551));
#47590=CARTESIAN_POINT('Ctrl Pts',(4.42856001249322,4.40015579830073,17.9099716392784));
#47591=CARTESIAN_POINT('Ctrl Pts',(5.30396800424161,2.64415760307637,17.8171818807016));
#47592=CARTESIAN_POINT('Ctrl Pts',(6.17937599599001,0.888159407852008,17.7243921221248));
#47593=CARTESIAN_POINT('Ctrl Pts',(6.09609935804498,-1.34576649178713,17.6316023635481));
#47594=CARTESIAN_POINT('Ctrl Pts',(5.09238196443743,-3.0317143579496,17.5388126049713));
#47595=CARTESIAN_POINT('Ctrl Pts',(4.0886645708299,-4.71766222411203,17.4460228463946));
#47596=CARTESIAN_POINT('Ctrl Pts',(2.1645064215599,-5.8556320567979,17.3532330878178));
#47597=CARTESIAN_POINT('Ctrl Pts',(0.203555844562213,-5.92302380866985,
17.2604433292411));
#47598=CARTESIAN_POINT('Ctrl Pts',(-1.75739473243558,-5.99041556054181,
17.1676535706643));
#47599=CARTESIAN_POINT('Ctrl Pts',(-3.75513773716107,-4.9872292315997,17.0748638120876));
#47600=CARTESIAN_POINT('Ctrl Pts',(-4.8722318114603,-3.37416703725817,16.9820740535108));
#47601=CARTESIAN_POINT('Ctrl Pts',(-5.54921923333517,-2.39661031988311,
16.9258410997422));
#47602=CARTESIAN_POINT('Ctrl Pts',(-5.90277351648673,-1.1950664283202,16.8696081459735));
#47603=CARTESIAN_POINT('Ctrl Pts',(-5.9087266087589,0.0032487932499714,
16.8133751922049));
#47604=CARTESIAN_POINT('Ctrl Pts',(-5.90693863091242,3.43002300271205E-5,
16.5616248077955));
#47605=CARTESIAN_POINT('Ctrl Pts',(-5.90688756251691,-0.991645464752838,
16.6081259059003));
#47606=CARTESIAN_POINT('Ctrl Pts',(-5.67070980570828,-1.98334808692469,
16.654627004005));
#47607=CARTESIAN_POINT('Ctrl Pts',(-5.19854053303828,-2.84586079535849,
16.7011281021098));
#47608=CARTESIAN_POINT('Ctrl Pts',(-4.2561743393455,-4.56728331288531,16.7939360533255));
#47609=CARTESIAN_POINT('Ctrl Pts',(-2.37378111172378,-5.77410253638496,
16.8867440045412));
#47610=CARTESIAN_POINT('Ctrl Pts',(-0.416139401428914,-5.91190116111381,
16.9795519557569));
#47611=CARTESIAN_POINT('Ctrl Pts',(1.54150230886587,-6.04969978584265,17.0723599069726));
#47612=CARTESIAN_POINT('Ctrl Pts',(3.5743925018338,-5.11847781180086,17.1651678581883));
#47613=CARTESIAN_POINT('Ctrl Pts',(4.74861375249686,-3.54604212747086,17.257975809404));
#47614=CARTESIAN_POINT('Ctrl Pts',(5.92283500315997,-1.9736064431408,17.3507837606197));
#47615=CARTESIAN_POINT('Ctrl Pts',(6.23838731151808,0.240042951477567,17.4435917118355));
#47616=CARTESIAN_POINT('Ctrl Pts',(5.55030475649628,2.07794717214253,17.5363996630512));
#47617=CARTESIAN_POINT('Ctrl Pts',(4.8622222014745,3.91585139280746,17.6292076142669));
#47618=CARTESIAN_POINT('Ctrl Pts',(3.1705047830729,5.37801043951901,17.7220155654826));
#47619=CARTESIAN_POINT('Ctrl Pts',(1.25233386634964,5.79270292932359,17.8148235166983));
#47620=CARTESIAN_POINT('Ctrl Pts',(-0.665837050373649,6.20739541912817,
17.907631467914));
#47621=CARTESIAN_POINT('Ctrl Pts',(-2.81046146541861,5.5746213520257,18.0004394191297));
#47622=CARTESIAN_POINT('Ctrl Pts',(-4.19629083059877,4.18507952197244,18.0932473703454));
#47623=CARTESIAN_POINT('Ctrl Pts',(-5.28324462980405,3.09521390844165,18.1660398494955));
#47624=CARTESIAN_POINT('Ctrl Pts',(-5.90340241438398,1.53979942792063,18.2388323286455));
#47625=CARTESIAN_POINT('Ctrl Pts',(-5.91777217212816,-0.00540066091151231,
18.3116248077955));
#47626=CARTESIAN_POINT('Origin',(0.,0.,-10.));
#47627=CARTESIAN_POINT('',(-5.92622532488715,-0.00120034675680336,20.3133751922049));
#47628=CARTESIAN_POINT('',(-5.92528153879606,0.00246997438850003,20.0616248077955));
#47629=CARTESIAN_POINT('',(-5.91675,-7.2459289488551E-16,-10.));
#47630=CARTESIAN_POINT('Ctrl Pts',(-5.92622532488715,-0.00120034675680336,
20.3133751922049));
#47631=CARTESIAN_POINT('Ctrl Pts',(-5.92097756735111,1.89680731405714,20.2236288236512));
#47632=CARTESIAN_POINT('Ctrl Pts',(-4.92835420966625,3.7995314474951,20.1338824550975));
#47633=CARTESIAN_POINT('Ctrl Pts',(-3.36650141622386,4.8775315718597,20.0441360865437));
#47634=CARTESIAN_POINT('Ctrl Pts',(-1.75168461670958,5.9920877694804,19.951346327967));
#47635=CARTESIAN_POINT('Ctrl Pts',(0.471622498167445,6.22503711256374,19.8585565693902));
#47636=CARTESIAN_POINT('Ctrl Pts',(2.28239074985864,5.46940019425212,19.7657668108135));
#47637=CARTESIAN_POINT('Ctrl Pts',(4.09315900154977,4.71376327594051,19.6729770522367));
#47638=CARTESIAN_POINT('Ctrl Pts',(5.4913883900551,2.96954009623401,19.58018729366));
#47639=CARTESIAN_POINT('Ctrl Pts',(5.83495754832857,1.03774584033322,19.4873975350832));
#47640=CARTESIAN_POINT('Ctrl Pts',(6.17852670660203,-0.894048415567604,
19.3946077765065));
#47641=CARTESIAN_POINT('Ctrl Pts',(5.46743563464361,-3.01341374766271,19.3018180179297));
#47642=CARTESIAN_POINT('Ctrl Pts',(4.0282450348487,-4.3470550904195,19.2090282593529));
#47643=CARTESIAN_POINT('Ctrl Pts',(2.5890544350538,-5.68069643317628,19.1162385007762));
#47644=CARTESIAN_POINT('Ctrl Pts',(0.421764307422399,-6.22861378659473,
19.0234487421994));
#47645=CARTESIAN_POINT('Ctrl Pts',(-1.47832135073232,-5.73918217204283,
18.9306589836227));
#47646=CARTESIAN_POINT('Ctrl Pts',(-3.37840700888707,-5.24975055749093,
18.8378692250459));
#47647=CARTESIAN_POINT('Ctrl Pts',(-5.01128819756513,-3.72296997496864,
18.7450794664691));
#47648=CARTESIAN_POINT('Ctrl Pts',(-5.62708230829223,-1.85999750419993,
18.6522897078924));
#47649=CARTESIAN_POINT('Ctrl Pts',(-5.82377440002851,-1.26494155004352,
18.6226515359966));
#47650=CARTESIAN_POINT('Ctrl Pts',(-5.91669910681317,-0.63558592396959,
18.5930133641007));
#47651=CARTESIAN_POINT('Ctrl Pts',(-5.91186200022437,-0.00484233898808362,
18.5633751922049));
#47652=CARTESIAN_POINT('Ctrl Pts',(-5.91777217212816,-0.00540066091151231,
18.3116248077955));
#47653=CARTESIAN_POINT('Ctrl Pts',(-5.92172336994527,-0.430278472122732,
18.3316402798612));
#47654=CARTESIAN_POINT('Ctrl Pts',(-5.8798731060043,-0.854384009783482,
18.3516557519269));
#47655=CARTESIAN_POINT('Ctrl Pts',(-5.78933184621644,-1.26782653174028,
18.3716712239925));
#47656=CARTESIAN_POINT('Ctrl Pts',(-5.3695091813386,-3.18488116239587,18.4644791752083));
#47657=CARTESIAN_POINT('Ctrl Pts',(-3.90282953626755,-4.87268083070307,
18.557287126424));
#47658=CARTESIAN_POINT('Ctrl Pts',(-2.06309107389996,-5.55584400077924,
18.6500950776397));
#47659=CARTESIAN_POINT('Ctrl Pts',(-0.223352611532319,-6.23900717085543,
18.7429030288554));
#47660=CARTESIAN_POINT('Ctrl Pts',(1.98944466813189,-5.91753384270046,18.8357109800711));
#47661=CARTESIAN_POINT('Ctrl Pts',(3.55873334567604,-4.73911007622462,18.9285189312868));
#47662=CARTESIAN_POINT('Ctrl Pts',(5.12802202322017,-3.5606863097488,19.0213268825025));
#47663=CARTESIAN_POINT('Ctrl Pts',(6.05380209864429,-1.52531210495216,19.1141348337182));
#47664=CARTESIAN_POINT('Ctrl Pts',(5.91076671222382,0.43195394878065,19.2069427849339));
#47665=CARTESIAN_POINT('Ctrl Pts',(5.76773132580335,2.38922000251349,19.2997507361496));
#47666=CARTESIAN_POINT('Ctrl Pts',(4.55588047753819,4.26837790518251,19.3925586873654));
#47667=CARTESIAN_POINT('Ctrl Pts',(2.83194301957413,5.20613542602243,19.4853666385811));
#47668=CARTESIAN_POINT('Ctrl Pts',(1.10800556161013,6.14389294686232,19.5781745897968));
#47669=CARTESIAN_POINT('Ctrl Pts',(-1.12801850605279,6.14025008587321,19.6709825410125));
#47670=CARTESIAN_POINT('Ctrl Pts',(-2.84889128995409,5.19688038713843,19.7637904922282));
#47671=CARTESIAN_POINT('Ctrl Pts',(-4.56976407385542,4.25351068840363,19.8565984434439));
#47672=CARTESIAN_POINT('Ctrl Pts',(-5.77548557399514,2.37041415192319,19.9494063946596));
#47673=CARTESIAN_POINT('Ctrl Pts',(-5.91214278388311,0.412692431696099,
20.0422143458753));
#47674=CARTESIAN_POINT('Ctrl Pts',(-5.92166991144025,0.276208856732997,
20.0486844998487));
#47675=CARTESIAN_POINT('Ctrl Pts',(-5.9260011162672,0.139362584510233,20.0551546538221));
#47676=CARTESIAN_POINT('Ctrl Pts',(-5.92528153879606,0.00246997438850003,
20.0616248077955));
#47677=CARTESIAN_POINT('Origin',(0.,0.,-10.));
#47678=CARTESIAN_POINT('',(-5.91548613894553,0.00544808287233939,22.0633751922049));
#47679=CARTESIAN_POINT('',(-5.91019222577512,0.00418729649785822,21.8116248077955));
#47680=CARTESIAN_POINT('',(-5.91675,-7.2459289488551E-16,-10.));
#47681=CARTESIAN_POINT('Ctrl Pts',(-5.91548613894553,0.00544808287233939,
22.0633751922049));
#47682=CARTESIAN_POINT('Ctrl Pts',(-5.92001583191384,0.505878420791942,
22.0398238003552));
#47683=CARTESIAN_POINT('Ctrl Pts',(-5.86183352928881,1.00527075686111,22.0162724085054));
#47684=CARTESIAN_POINT('Ctrl Pts',(-5.73685045715431,1.4873442278685,21.9927210166556));
#47685=CARTESIAN_POINT('Ctrl Pts',(-5.24443161568961,3.38665791923673,21.8999312580789));
#47686=CARTESIAN_POINT('Ctrl Pts',(-3.71508526038522,5.01713626899271,21.8071414995021));
#47687=CARTESIAN_POINT('Ctrl Pts',(-1.85114677370993,5.63000014583558,21.7143517409254));
#47688=CARTESIAN_POINT('Ctrl Pts',(0.0127917129653046,6.24286402267844,
21.6215619823486));
#47689=CARTESIAN_POINT('Ctrl Pts',(2.21132233101142,5.83811342660825,21.5287722237718));
#47690=CARTESIAN_POINT('Ctrl Pts',(3.73479423375194,4.60162558792636,21.4359824651951));
#47691=CARTESIAN_POINT('Ctrl Pts',(5.25826613649246,3.36513774924446,21.3431927066183));
#47692=CARTESIAN_POINT('Ctrl Pts',(6.10667932392737,1.29691266795085,21.2504029480416));
#47693=CARTESIAN_POINT('Ctrl Pts',(5.8904094324049,-0.65324018443506,21.1576131894648));
#47694=CARTESIAN_POINT('Ctrl Pts',(5.67413954088243,-2.603393036821,21.0648234308881));
#47695=CARTESIAN_POINT('Ctrl Pts',(4.39318657040249,-4.43547366029928,20.9720336723113));
#47696=CARTESIAN_POINT('Ctrl Pts',(2.6358139913858,-5.30811931127591,20.8792439137345));
#47697=CARTESIAN_POINT('Ctrl Pts',(0.878441412369118,-6.18076496225253,
20.7864541551578));
#47698=CARTESIAN_POINT('Ctrl Pts',(-1.35535077518424,-6.09397564072757,
20.6936643965811));
#47699=CARTESIAN_POINT('Ctrl Pts',(-3.03971823917821,-5.0876083817775,20.6008746380043));
#47700=CARTESIAN_POINT('Ctrl Pts',(-4.7240857031722,-4.08124112282742,20.5080848794275));
#47701=CARTESIAN_POINT('Ctrl Pts',(-5.85902844360669,-2.15529592645219,
20.4152951208508));
#47702=CARTESIAN_POINT('Ctrl Pts',(-5.92333657174814,-0.194241802185547,
20.322505362274));
#47703=CARTESIAN_POINT('Ctrl Pts',(-5.92544579930286,-0.129921637460919,
20.319461972251));
#47704=CARTESIAN_POINT('Ctrl Pts',(-5.92640328164669,-0.0655637039783095,
20.3164185822279));
#47705=CARTESIAN_POINT('Ctrl Pts',(-5.92622532488715,-0.00120034675680336,
20.3133751922049));
#47706=CARTESIAN_POINT('Ctrl Pts',(-5.92528153879606,0.00246997438850003,
20.0616248077955));
#47707=CARTESIAN_POINT('Ctrl Pts',(-5.91567949005679,-1.82422633999111,
20.1479626050378));
#47708=CARTESIAN_POINT('Ctrl Pts',(-5.00672204207656,-3.65917370087608,
20.2343004022801));
#47709=CARTESIAN_POINT('Ctrl Pts',(-3.54327287359004,-4.75068044426073,
20.3206381995225));
#47710=CARTESIAN_POINT('Ctrl Pts',(-1.97015283377279,-5.92398469601676,
20.4134461507382));
#47711=CARTESIAN_POINT('Ctrl Pts',(0.243680165497836,-6.23824629555509,
20.5062541019539));
#47712=CARTESIAN_POINT('Ctrl Pts',(2.08118289131029,-5.54909227830262,20.5990620531696));
#47713=CARTESIAN_POINT('Ctrl Pts',(3.91868561712269,-4.85993826105017,20.6918700043853));
#47714=CARTESIAN_POINT('Ctrl Pts',(5.3798580694769,-3.16736862700695,20.784677955601));
#47715=CARTESIAN_POINT('Ctrl Pts',(5.79343211058954,-1.24895625231246,20.8774859068167));
#47716=CARTESIAN_POINT('Ctrl Pts',(6.20700615170218,0.669456122382023,20.9702938580324));
#47717=CARTESIAN_POINT('Ctrl Pts',(5.57298178157328,2.81371123772783,21.0631018092481));
#47718=CARTESIAN_POINT('Ctrl Pts',(4.18263218808697,4.19873020321373,21.1559097604638));
#47719=CARTESIAN_POINT('Ctrl Pts',(2.79228259460061,5.58374916869967,21.2487177116796));
#47720=CARTESIAN_POINT('Ctrl Pts',(0.645607777756869,6.20953198432568,21.3415256628953));
#47721=CARTESIAN_POINT('Ctrl Pts',(-1.27120175193518,5.78859166344261,21.434333614111));
#47722=CARTESIAN_POINT('Ctrl Pts',(-3.18801128162718,5.36765134255955,21.5271415653267));
#47723=CARTESIAN_POINT('Ctrl Pts',(-4.87495552416746,3.89998788516743,21.6199495165424));
#47724=CARTESIAN_POINT('Ctrl Pts',(-5.55704592949822,2.05985142125534,21.7127574677581));
#47725=CARTESIAN_POINT('Ctrl Pts',(-5.79925385513654,1.40642537636112,21.7457132477706));
#47726=CARTESIAN_POINT('Ctrl Pts',(-5.91475620853708,0.706032893476995,
21.7786690277831));
#47727=CARTESIAN_POINT('Ctrl Pts',(-5.91019222577512,0.00418729649785822,
21.8116248077955));
#47728=CARTESIAN_POINT('Origin',(0.,0.,-10.));
#47729=CARTESIAN_POINT('',(-5.90721141655292,-0.00131122188027244,23.8133751922049));
#47730=CARTESIAN_POINT('',(-5.91000536569632,-0.00409134141470152,23.5616248077955));
#47731=CARTESIAN_POINT('',(-5.91675,-7.2459289488551E-16,-10.));
#47732=CARTESIAN_POINT('Ctrl Pts',(-5.90721141655292,-0.00131122188027244,
23.8133751922049));
#47733=CARTESIAN_POINT('Ctrl Pts',(-5.90510013293806,1.06798059387856,23.7632290184824));
#47734=CARTESIAN_POINT('Ctrl Pts',(-5.62812187284361,2.13829178876222,23.7130828447598));
#47735=CARTESIAN_POINT('Ctrl Pts',(-5.08282221913792,3.0477146041851,23.6629366710372));
#47736=CARTESIAN_POINT('Ctrl Pts',(-4.07380758326,4.73049750112469,23.5701469124605));
#47737=CARTESIAN_POINT('Ctrl Pts',(-2.14608010200764,5.86241034296819,23.4773571538837));
#47738=CARTESIAN_POINT('Ctrl Pts',(-0.184927279512977,5.92363468836636,
23.384567395307));
#47739=CARTESIAN_POINT('Ctrl Pts',(1.77622554298163,5.98485903376453,23.2917776367302));
#47740=CARTESIAN_POINT('Ctrl Pts',(3.77080370671858,4.97539488271743,23.1989878781534));
#47741=CARTESIAN_POINT('Ctrl Pts',(4.88281927173037,3.35882747094039,23.1061981195767));
#47742=CARTESIAN_POINT('Ctrl Pts',(5.99483483674221,1.74226005916329,23.0134083609999));
#47743=CARTESIAN_POINT('Ctrl Pts',(6.22428780302885,-0.481410613343747,
22.9206186024232));
#47744=CARTESIAN_POINT('Ctrl Pts',(5.46580443606862,-2.29098840821553,22.8278288438465));
#47745=CARTESIAN_POINT('Ctrl Pts',(4.70732106910843,-4.10056620308723,22.7350390852697));
#47746=CARTESIAN_POINT('Ctrl Pts',(2.96090136890143,-5.49605112032366,22.6422493266929));
#47747=CARTESIAN_POINT('Ctrl Pts',(1.0285692483707,-5.8365821609253,22.5494595681161));
#47748=CARTESIAN_POINT('Ctrl Pts',(-0.903762872160078,-6.17711320152695,
22.4566698095394));
#47749=CARTESIAN_POINT('Ctrl Pts',(-3.02200741301463,-5.46269036549375,
22.3638800509627));
#47750=CARTESIAN_POINT('Ctrl Pts',(-4.35338401962936,-4.0214044309869,22.2710902923859));
#47751=CARTESIAN_POINT('Ctrl Pts',(-5.34683785714821,-2.94593785339808,
22.2018519256589));
#47752=CARTESIAN_POINT('Ctrl Pts',(-5.90216936578403,-1.46575920199717,
22.1326135589319));
#47753=CARTESIAN_POINT('Ctrl Pts',(-5.91548613894553,0.00544808287233939,
22.0633751922049));
#47754=CARTESIAN_POINT('Ctrl Pts',(-5.91019222577512,0.00418729649785822,
21.8116248077955));
#47755=CARTESIAN_POINT('Ctrl Pts',(-5.90190341338669,-1.2704596034613,21.8714769789988));
#47756=CARTESIAN_POINT('Ctrl Pts',(-5.49759390107015,-2.54989938108599,
21.931329150202));
#47757=CARTESIAN_POINT('Ctrl Pts',(-4.73703437229062,-3.56149585089434,
21.9911813214053));
#47758=CARTESIAN_POINT('Ctrl Pts',(-3.55769584163102,-5.13009718869973,
22.083989272621));
#47759=CARTESIAN_POINT('Ctrl Pts',(-1.52178221219059,-6.05469039387844,
22.1767972238367));
#47760=CARTESIAN_POINT('Ctrl Pts',(0.435400112929308,-5.91051385937479,
22.2696051750524));
#47761=CARTESIAN_POINT('Ctrl Pts',(2.39258243804923,-5.76633732487114,22.3624131262681));
#47762=CARTESIAN_POINT('Ctrl Pts',(4.27103345884864,-4.55339105068509,22.4552210774838));
#47763=CARTESIAN_POINT('Ctrl Pts',(5.20778568876036,-2.82890713176364,22.5480290286995));
#47764=CARTESIAN_POINT('Ctrl Pts',(6.14453791867207,-1.1044232128422,22.6408369799152));
#47765=CARTESIAN_POINT('Ctrl Pts',(6.13959135769615,1.13159835081458,22.7336449311309));
#47766=CARTESIAN_POINT('Ctrl Pts',(5.19521847460889,2.85192081609621,22.8264528823466));
#47767=CARTESIAN_POINT('Ctrl Pts',(4.25084559152163,4.57224328137783,22.9192608335623));
#47768=CARTESIAN_POINT('Ctrl Pts',(2.36704638632299,5.77686664828424,23.0120687847781));
#47769=CARTESIAN_POINT('Ctrl Pts',(0.409245321672443,5.91238239687603,23.1048767359938));
#47770=CARTESIAN_POINT('Ctrl Pts',(-1.54855574297816,6.04789814546782,23.1976846872095));
#47771=CARTESIAN_POINT('Ctrl Pts',(-3.58035866708069,5.11430627574492,23.2904926384252));
#47772=CARTESIAN_POINT('Ctrl Pts',(-4.75274552107614,3.54050241520763,23.3833005896409));
#47773=CARTESIAN_POINT('Ctrl Pts',(-5.50363294101133,2.53251642807758,23.4427419956924));
#47774=CARTESIAN_POINT('Ctrl Pts',(-5.901978050059,1.26190815291944,23.502183401744));
#47775=CARTESIAN_POINT('Ctrl Pts',(-5.91000536569632,-0.00409134141470152,
23.5616248077955));
#47776=CARTESIAN_POINT('Origin',(0.,0.,-10.));
#47777=CARTESIAN_POINT('',(-5.92031232679181,-0.00496695537298586,25.5633751922049));
#47778=CARTESIAN_POINT('',(-5.9251298904235,-0.0026123641298589,25.3116248077955));
#47779=CARTESIAN_POINT('',(-5.91675,-7.2459289488551E-16,-10.));
#47780=CARTESIAN_POINT('Ctrl Pts',(-5.92031232679181,-0.00496695537298586,
25.5633751922049));
#47781=CARTESIAN_POINT('Ctrl Pts',(-5.90569424287378,1.62225043238685,25.4866342366096));
#47782=CARTESIAN_POINT('Ctrl Pts',(-5.20828674903878,3.26047459758013,25.4098932810142));
#47783=CARTESIAN_POINT('Ctrl Pts',(-4.01455388351686,4.35970218435446,25.3331523254189));
#47784=CARTESIAN_POINT('Ctrl Pts',(-2.57117617812347,5.68881076277143,25.2403625668421));
#47785=CARTESIAN_POINT('Ctrl Pts',(-0.402173600912262,6.22990940771235,
25.1475728082653));
#47786=CARTESIAN_POINT('Ctrl Pts',(1.49636342729237,5.73450455692444,25.0547830496886));
#47787=CARTESIAN_POINT('Ctrl Pts',(3.39490045549694,5.23909970613655,24.9619932911118));
#47788=CARTESIAN_POINT('Ctrl Pts',(5.02297193469495,3.70719135961988,24.8692035325351));
#47789=CARTESIAN_POINT('Ctrl Pts',(5.63290406224316,1.84229146594393,24.7764137739583));
#47790=CARTESIAN_POINT('Ctrl Pts',(6.24283618979139,-0.0226084277320635,
24.6836240153816));
#47791=CARTESIAN_POINT('Ctrl Pts',(5.83462896568976,-2.22049986856735,24.5908342568048));
#47792=CARTESIAN_POINT('Ctrl Pts',(4.59574703839515,-3.74202554494321,24.4980444982281));
#47793=CARTESIAN_POINT('Ctrl Pts',(3.35686511110057,-5.26355122131904,24.4052547396513));
#47794=CARTESIAN_POINT('Ctrl Pts',(1.28730848061306,-6.10871113323548,24.3124649810745));
#47795=CARTESIAN_POINT('Ctrl Pts',(-0.662501882322089,-5.88937494780601,
24.2196752224978));
#47796=CARTESIAN_POINT('Ctrl Pts',(-2.61231224525729,-5.67003876237653,
24.126885463921));
#47797=CARTESIAN_POINT('Ctrl Pts',(-4.44237634064012,-4.38620647960109,
24.0340957053443));
#47798=CARTESIAN_POINT('Ctrl Pts',(-5.31225749307975,-2.62746386219553,
23.9413059467675));
#47799=CARTESIAN_POINT('Ctrl Pts',(-5.71203060711839,-1.81919481189961,
23.8986623619133));
#47800=CARTESIAN_POINT('Ctrl Pts',(-5.90900682177127,-0.910621601800537,
23.8560187770591));
#47801=CARTESIAN_POINT('Ctrl Pts',(-5.90721141655292,-0.00131122188027244,
23.8133751922049));
#47802=CARTESIAN_POINT('Ctrl Pts',(-5.91000536569632,-0.00409134141470152,
23.5616248077955));
#47803=CARTESIAN_POINT('Ctrl Pts',(-5.91451137939202,-0.71474124207285,
23.5949913529597));
#47804=CARTESIAN_POINT('Ctrl Pts',(-5.79602940848674,-1.42393892949713,
23.6283578981239));
#47805=CARTESIAN_POINT('Ctrl Pts',(-5.54787791374812,-2.08441790299983,
23.661724443288));
#47806=CARTESIAN_POINT('Ctrl Pts',(-4.8576526685363,-3.92151850931827,23.7545323945037));
#47807=CARTESIAN_POINT('Ctrl Pts',(-3.16423139422438,-5.38170387060348,
23.8473403457194));
#47808=CARTESIAN_POINT('Ctrl Pts',(-1.24557821370455,-5.79415932243367,
23.9401482969352));
#47809=CARTESIAN_POINT('Ctrl Pts',(0.673074966815246,-6.20661477426384,
24.0329562481509));
#47810=CARTESIAN_POINT('Ctrl Pts',(2.81696005354294,-5.57134031663897,24.1257641993666));
#47811=CARTESIAN_POINT('Ctrl Pts',(4.20116814851063,-4.18018343235558,24.2185721505823));
#47812=CARTESIAN_POINT('Ctrl Pts',(5.58537624347835,-2.78902654807216,24.311380101798));
#47813=CARTESIAN_POINT('Ctrl Pts',(6.20990734668606,-0.641987237130237,
24.4041880530137));
#47814=CARTESIAN_POINT('Ctrl Pts',(5.78784951289245,1.27457653999713,24.4969960042294));
#47815=CARTESIAN_POINT('Ctrl Pts',(5.36579167909883,3.19114031712452,24.5898039554451));
#47816=CARTESIAN_POINT('Ctrl Pts',(3.89714490830379,4.87722856043733,24.6826119066608));
#47817=CARTESIAN_POINT('Ctrl Pts',(2.05661106838393,5.5582459691526,24.7754198578766));
#47818=CARTESIAN_POINT('Ctrl Pts',(0.216077228464096,6.23926337786785,24.8682278090923));
#47819=CARTESIAN_POINT('Ctrl Pts',(-1.99634368058052,5.91520995198563,24.961035760308));
#47820=CARTESIAN_POINT('Ctrl Pts',(-3.56425714541619,4.73495705804709,25.0538437115237));
#47821=CARTESIAN_POINT('Ctrl Pts',(-5.01592318095989,3.64220986382467,25.1397707436143));
#47822=CARTESIAN_POINT('Ctrl Pts',(-5.91510841625453,1.81551650414691,25.2256977757049));
#47823=CARTESIAN_POINT('Ctrl Pts',(-5.9251298904235,-0.0026123641298589,
25.3116248077955));
#47824=CARTESIAN_POINT('Origin',(0.,0.,-10.));
#47825=CARTESIAN_POINT('',(-5.92348042272801,0.00375680996992422,27.3133751922049));
#47826=CARTESIAN_POINT('',(-5.91803924330658,0.00537434068105684,27.0616248077955));
#47827=CARTESIAN_POINT('',(-5.91675,-7.2459289488551E-16,-10.));
#47828=CARTESIAN_POINT('Ctrl Pts',(-5.92348042272801,0.00375680996992422,
27.3133751922049));
#47829=CARTESIAN_POINT('Ctrl Pts',(-5.92513185972389,0.227062797683139,
27.3028292133135));
#47830=CARTESIAN_POINT('Ctrl Pts',(-5.91360289431451,0.450196582758903,
27.2922832344221));
#47831=CARTESIAN_POINT('Ctrl Pts',(-5.88832590072296,0.671761942060206,
27.2817372555307));
#47832=CARTESIAN_POINT('Ctrl Pts',(-5.66592396373262,2.62122499430588,27.188947496954));
#47833=CARTESIAN_POINT('Ctrl Pts',(-4.37921554315603,4.44926803644757,27.0961577383772));
#47834=CARTESIAN_POINT('Ctrl Pts',(-2.61910723615281,5.3163825394207,27.0033679798005));
#47835=CARTESIAN_POINT('Ctrl Pts',(-0.858998929149595,6.18349704239383,
26.9105782212237));
#47836=CARTESIAN_POINT('Ctrl Pts',(1.3745092642802,6.08968300619837,26.817788462647));
#47837=CARTESIAN_POINT('Ctrl Pts',(3.05570343319762,5.07802348835348,26.7249987040702));
#47838=CARTESIAN_POINT('Ctrl Pts',(4.73689760211508,4.06636397050856,26.6322089454934));
#47839=CARTESIAN_POINT('Ctrl Pts',(5.86577774652006,2.13685897101416,26.5394191869167));
#47840=CARTESIAN_POINT('Ctrl Pts',(5.92391815778737,0.175612299576325,26.4466294283399));
#47841=CARTESIAN_POINT('Ctrl Pts',(5.98205856905467,-1.78563437186146,26.3538396697632));
#47842=CARTESIAN_POINT('Ctrl Pts',(4.96945924718425,-3.77862271524274,26.2610499111864));
#47843=CARTESIAN_POINT('Ctrl Pts',(3.35114522038306,-4.88809489799749,26.1682601526097));
#47844=CARTESIAN_POINT('Ctrl Pts',(1.73283119358188,-5.99756708075225,26.0754703940329));
#47845=CARTESIAN_POINT('Ctrl Pts',(-0.491197538150089,-6.22352310288061,
25.9826806354562));
#47846=CARTESIAN_POINT('Ctrl Pts',(-2.29958040171263,-5.46219516275138,
25.8898908768794));
#47847=CARTESIAN_POINT('Ctrl Pts',(-4.10796326527522,-4.70086722262212,
25.7971011183026));
#47848=CARTESIAN_POINT('Ctrl Pts',(-5.50070026066831,-2.95225532023523,
25.7043113597259));
#47849=CARTESIAN_POINT('Ctrl Pts',(-5.83819234157705,-1.01939011309528,
25.6115216011491));
#47850=CARTESIAN_POINT('Ctrl Pts',(-5.89656455848294,-0.685084114515375,
25.5954727981677));
#47851=CARTESIAN_POINT('Ctrl Pts',(-5.92336940038369,-0.345266226622166,
25.5794239951863));
#47852=CARTESIAN_POINT('Ctrl Pts',(-5.92031232679181,-0.00496695537298586,
25.5633751922049));
#47853=CARTESIAN_POINT('Ctrl Pts',(-5.9251298904235,-0.0026123641298589,
25.3116248077955));
#47854=CARTESIAN_POINT('Ctrl Pts',(-5.92593239635899,-0.148205635504764,
25.3185057269206));
#47855=CARTESIAN_POINT('Ctrl Pts',(-5.9210330621433,-0.293743986331754,
25.3253866460457));
#47856=CARTESIAN_POINT('Ctrl Pts',(-5.91025899730312,-0.438846129067858,
25.3322675651708));
#47857=CARTESIAN_POINT('Ctrl Pts',(-5.76494136372773,-2.39594406024946,
25.4250755163865));
#47858=CARTESIAN_POINT('Ctrl Pts',(-4.55090007595029,-4.2736875606178,25.5178834676022));
#47859=CARTESIAN_POINT('Ctrl Pts',(-2.82587028229322,-5.20943418116137,
25.6106914188179));
#47860=CARTESIAN_POINT('Ctrl Pts',(-1.1008404886361,-6.14518080170496,25.7034993700336));
#47861=CARTESIAN_POINT('Ctrl Pts',(1.13517781090063,-6.13893054242372,25.7963073212493));
#47862=CARTESIAN_POINT('Ctrl Pts',(2.85494937275541,-5.19355479601437,25.889115272465));
#47863=CARTESIAN_POINT('Ctrl Pts',(4.57472093461016,-4.24817904960505,25.9819232236808));
#47864=CARTESIAN_POINT('Ctrl Pts',(5.77824575878293,-2.36367781606772,26.0747311748965));
#47865=CARTESIAN_POINT('Ctrl Pts',(5.91262000001114,-0.405798072529415,
26.1675391261122));
#47866=CARTESIAN_POINT('Ctrl Pts',(6.04699424123935,1.55208167100884,26.2603470773279));
#47867=CARTESIAN_POINT('Ctrl Pts',(5.11221789952294,3.58333992454814,26.3531550285436));
#47868=CARTESIAN_POINT('Ctrl Pts',(3.53773075326523,4.75480898224122,26.4459629797593));
#47869=CARTESIAN_POINT('Ctrl Pts',(1.96324360700748,5.92627803993433,26.538770930975));
#47870=CARTESIAN_POINT('Ctrl Pts',(-0.250954343791611,6.2379579017813,26.6315788821908));
#47871=CARTESIAN_POINT('Ctrl Pts',(-2.0876522061113,5.54666166324565,26.7243868334065));
#47872=CARTESIAN_POINT('Ctrl Pts',(-3.92435006843105,4.85536542470998,26.8171947846222));
#47873=CARTESIAN_POINT('Ctrl Pts',(-5.38354784227131,3.16109308579165,26.9100027358379));
#47874=CARTESIAN_POINT('Ctrl Pts',(-5.79488456460875,1.24219975167425,27.0028106870536));
#47875=CARTESIAN_POINT('Ctrl Pts',(-5.88177513571553,0.836853648007722,
27.0224153939676));
#47876=CARTESIAN_POINT('Ctrl Pts',(-5.92190791045004,0.421484476168763,
27.0420201008815));
#47877=CARTESIAN_POINT('Ctrl Pts',(-5.91803924330658,0.00537434068105684,
27.0616248077955));
#47878=CARTESIAN_POINT('Origin',(0.,0.,-10.));
#47879=CARTESIAN_POINT('',(-5.90852622603088,0.0030797858564896,29.0633751922049));
#47880=CARTESIAN_POINT('',(-5.90694030856026,0.000110760884720807,28.8116248077955));
#47881=CARTESIAN_POINT('',(-5.91675,-7.2459289488551E-16,-10.));
#47882=CARTESIAN_POINT('Ctrl Pts',(-5.90852622603088,0.0030797858564896,
29.0633751922049));
#47883=CARTESIAN_POINT('Ctrl Pts',(-5.91224613300031,0.79461059927319,29.0262344314407));
#47884=CARTESIAN_POINT('Ctrl Pts',(-5.76444534826255,1.58480920067904,28.9890936706765));
#47885=CARTESIAN_POINT('Ctrl Pts',(-5.45857238322479,2.30816670910508,28.9519529099124));
#47886=CARTESIAN_POINT('Ctrl Pts',(-4.69440175243967,4.1153501698233,28.8591631513356));
#47887=CARTESIAN_POINT('Ctrl Pts',(-2.94360197161417,5.5053357995932,28.7663733927588));
#47888=CARTESIAN_POINT('Ctrl Pts',(-1.01020845720406,5.83978808630234,28.6735836341821));
#47889=CARTESIAN_POINT('Ctrl Pts',(0.923185057206098,6.17424037301148,28.5807938756053));
#47890=CARTESIAN_POINT('Ctrl Pts',(3.03917230520087,5.4531593166598,28.4880041170286));
#47891=CARTESIAN_POINT('Ctrl Pts',(4.36600956897235,4.00769340937742,28.3952143584518));
#47892=CARTESIAN_POINT('Ctrl Pts',(5.69284683274379,2.56222750209508,28.3024245998751));
#47893=CARTESIAN_POINT('Ctrl Pts',(6.23053411229197,0.392376743882084,28.2096348412983));
#47894=CARTESIAN_POINT('Ctrl Pts',(5.73214447715392,-1.50537892670225,28.1168450827216));
#47895=CARTESIAN_POINT('Ctrl Pts',(5.23375484201585,-3.40313459728663,28.0240553241448));
#47896=CARTESIAN_POINT('Ctrl Pts',(3.69928829219149,-5.02879518024234,27.931265565568));
#47897=CARTESIAN_POINT('Ctrl Pts',(1.83343160279787,-5.63579405033464,27.8384758069913));
#47898=CARTESIAN_POINT('Ctrl Pts',(-0.0324250865956979,-6.24279292042693,
27.7456860484145));
#47899=CARTESIAN_POINT('Ctrl Pts',(-2.2296719155585,-5.83113007765588,27.6528962898378));
#47900=CARTESIAN_POINT('Ctrl Pts',(-3.74924760333789,-4.58985712509556,
27.560106531261));
#47901=CARTESIAN_POINT('Ctrl Pts',(-5.09611658972049,-3.48966049989016,
27.4778627515756));
#47902=CARTESIAN_POINT('Ctrl Pts',(-5.91060154046853,-1.73771533263892,
27.3956189718903));
#47903=CARTESIAN_POINT('Ctrl Pts',(-5.92348042272801,0.00375680996992422,
27.3133751922049));
#47904=CARTESIAN_POINT('Ctrl Pts',(-5.91803924330658,0.00537434068105684,
27.0616248077955));
#47905=CARTESIAN_POINT('Ctrl Pts',(-5.90359378450591,-1.54836538305896,
27.1348280520972));
#47906=CARTESIAN_POINT('Ctrl Pts',(-5.2756592157719,-3.11243597574232,27.208031296399));
#47907=CARTESIAN_POINT('Ctrl Pts',(-4.17773325561082,-4.20360466566063,
27.2812345407007));
#47908=CARTESIAN_POINT('Ctrl Pts',(-2.7857695534408,-5.58700141956182,27.3740424919164));
#47909=CARTESIAN_POINT('Ctrl Pts',(-0.638366478266117,-6.21028059804786,
27.4668504431321));
#47910=CARTESIAN_POINT('Ctrl Pts',(1.27795089477905,-5.78710539481819,27.5596583943478));
#47911=CARTESIAN_POINT('Ctrl Pts',(3.19426826782428,-5.3639301915885,27.6524663455635));
#47912=CARTESIAN_POINT('Ctrl Pts',(4.87949993873997,-3.89430060664304,27.7452742967793));
#47913=CARTESIAN_POINT('Ctrl Pts',(5.5594441193344,-2.05337001638734,27.838082247995));
#47914=CARTESIAN_POINT('Ctrl Pts',(6.2393882999288,-0.212439426131689,27.9308901992107));
#47915=CARTESIAN_POINT('Ctrl Pts',(5.91404499020199,1.99979216943419,28.0236981504264));
#47916=CARTESIAN_POINT('Ctrl Pts',(4.73287813420022,3.56701722830292,28.1165061016421));
#47917=CARTESIAN_POINT('Ctrl Pts',(3.55171127819844,5.13424228717165,28.2093140528578));
#47918=CARTESIAN_POINT('Ctrl Pts',(1.51472087592169,6.05646080934324,28.3021220040735));
#47919=CARTESIAN_POINT('Ctrl Pts',(-0.44229199602487,5.91000212609545,28.3949299552892));
#47920=CARTESIAN_POINT('Ctrl Pts',(-2.39930486797143,5.76354344284765,28.4877379065049));
#47921=CARTESIAN_POINT('Ctrl Pts',(-4.27634020958782,4.54840755418047,28.5805458577206));
#47922=CARTESIAN_POINT('Ctrl Pts',(-5.2110809026651,2.82283247219515,28.6733538089364));
#47923=CARTESIAN_POINT('Ctrl Pts',(-5.67529231132518,1.96587647842105,28.7194441418894));
#47924=CARTESIAN_POINT('Ctrl Pts',(-5.90710376233207,0.983029875912657,
28.7655344748425));
#47925=CARTESIAN_POINT('Ctrl Pts',(-5.90694030856026,0.000110760884720807,
28.8116248077955));
#47926=CARTESIAN_POINT('Origin',(0.,0.,-10.));
#47927=CARTESIAN_POINT('',(-5.9121820127379,-0.00493613606119603,30.8133751922049));
#47928=CARTESIAN_POINT('',(-5.91763133808765,-0.00541284032780908,30.5616248077955));
#47929=CARTESIAN_POINT('',(-5.91675,-7.2459289488551E-16,-10.));
#47930=CARTESIAN_POINT('Ctrl Pts',(-5.9121820127379,-0.00493613606119603,
30.8133751922049));
#47931=CARTESIAN_POINT('Ctrl Pts',(-5.90153888682002,1.35126409100681,30.7496396495679));
#47932=CARTESIAN_POINT('Ctrl Pts',(-5.43820318556864,2.71403437919626,30.6859041069309));
#47933=CARTESIAN_POINT('Ctrl Pts',(-4.58395586259118,3.75646039107845,30.622168564294));
#47934=CARTESIAN_POINT('Ctrl Pts',(-3.34029495402418,5.27408233285128,30.5293788057172));
#47935=CARTESIAN_POINT('Ctrl Pts',(-1.26809058042409,6.11272943237414,30.4365890471405));
#47936=CARTESIAN_POINT('Ctrl Pts',(0.681020340752165,5.88726229374972,30.3437992885637));
#47937=CARTESIAN_POINT('Ctrl Pts',(2.63013126192847,5.66179515512528,30.2510095299869));
#47938=CARTESIAN_POINT('Ctrl Pts',(4.45614873068094,4.3722137783535,30.1582197714102));
#47939=CARTESIAN_POINT('Ctrl Pts',(5.32049444009904,2.61074413392055,30.0654300128334));
#47940=CARTESIAN_POINT('Ctrl Pts',(6.18484014951711,0.849274489487636,29.9726402542567));
#47941=CARTESIAN_POINT('Ctrl Pts',(6.08751409960087,-1.38408342260643,29.8798504956799));
#47942=CARTESIAN_POINT('Ctrl Pts',(5.07321220128966,-3.0636847064623,29.7870607371032));
#47943=CARTESIAN_POINT('Ctrl Pts',(4.05891030297843,-4.74328599031823,29.6942709785264));
#47944=CARTESIAN_POINT('Ctrl Pts',(2.12763255627217,-5.86913064593594,29.6014812199496));
#47945=CARTESIAN_POINT('Ctrl Pts',(0.166296885408143,-5.92418697931023,
29.5086914613729));
#47946=CARTESIAN_POINT('Ctrl Pts',(-1.79503878545582,-5.97924331268453,
29.4159017027961));
#47947=CARTESIAN_POINT('Ctrl Pts',(-3.78643238047755,-4.96351132381548,
29.3231119442194));
#47948=CARTESIAN_POINT('Ctrl Pts',(-4.89335843761608,-3.34345468354768,
29.2303221856426));
#47949=CARTESIAN_POINT('Ctrl Pts',(-5.55721753884891,-2.37185469435356,
29.1746731878301));
#47950=CARTESIAN_POINT('Ctrl Pts',(-5.90295258966627,-1.18289205742564,
29.1190241900175));
#47951=CARTESIAN_POINT('Ctrl Pts',(-5.90852622603088,0.0030797858564896,
29.0633751922049));
#47952=CARTESIAN_POINT('Ctrl Pts',(-5.90694030856026,0.000110760884720807,
28.8116248077955));
#47953=CARTESIAN_POINT('Ctrl Pts',(-5.90677463019724,-0.996185795395627,
28.8583424260582));
#47954=CARTESIAN_POINT('Ctrl Pts',(-5.66827676300471,-1.99255685140481,
28.9050600443208));
#47955=CARTESIAN_POINT('Ctrl Pts',(-5.19188935192074,-2.8579769589016,28.9517776625835));
#47956=CARTESIAN_POINT('Ctrl Pts',(-4.24551106356089,-4.57719703270963,
29.0445856137992));
#47957=CARTESIAN_POINT('Ctrl Pts',(-2.36030844230297,-5.77962290502219,
29.1373935650149));
#47958=CARTESIAN_POINT('Ctrl Pts',(-0.402350685439387,-5.91285559320764,
29.2302015162306));
#47959=CARTESIAN_POINT('Ctrl Pts',(1.55560707142414,-6.04608828139308,29.3230094674463));
#47960=CARTESIAN_POINT('Ctrl Pts',(3.58631996389338,-5.11012778545148,29.415817418662));
#47961=CARTESIAN_POINT('Ctrl Pts',(4.75687082705447,-3.53495788870511,29.5086253698777));
#47962=CARTESIAN_POINT('Ctrl Pts',(5.92742169021559,-1.95978799195868,29.6014333210935));
#47963=CARTESIAN_POINT('Ctrl Pts',(6.23781052406856,0.254591305592438,29.6942412723092));
#47964=CARTESIAN_POINT('Ctrl Pts',(5.54544352720855,2.09088579954553,29.7870492235249));
#47965=CARTESIAN_POINT('Ctrl Pts',(4.85307653034854,3.92718029349861,29.8798571747406));
#47966=CARTESIAN_POINT('Ctrl Pts',(3.15795370277548,5.38538998385357,29.9726651259563));
#47967=CARTESIAN_POINT('Ctrl Pts',(1.23882086737003,5.79560783686828,30.065473077172));
#47968=CARTESIAN_POINT('Ctrl Pts',(-0.68031196803538,6.20582568988297,30.1582810283877));
#47969=CARTESIAN_POINT('Ctrl Pts',(-2.82345481127323,5.56805170555748,30.2510889796034));
#47970=CARTESIAN_POINT('Ctrl Pts',(-4.20603975383542,4.1752816586856,30.3438969308191));
#47971=CARTESIAN_POINT('Ctrl Pts',(-5.2872232815409,3.08613336392054,30.4164728898112));
#47972=CARTESIAN_POINT('Ctrl Pts',(-5.90330559059264,1.53528506123078,30.4890488488034));
#47973=CARTESIAN_POINT('Ctrl Pts',(-5.91763133808765,-0.00541284032780908,
30.5616248077955));
#47974=CARTESIAN_POINT('Origin',(0.,0.,-10.));
#47975=CARTESIAN_POINT('',(-5.9263255902637,-0.000973344357376172,32.5633751922049));
#47976=CARTESIAN_POINT('',(-5.92535850276232,0.00239395280352964,32.3116248077955));
#47977=CARTESIAN_POINT('',(-5.91675,-7.2459289488551E-16,-10.));
#47978=CARTESIAN_POINT('Ctrl Pts',(-5.9263255902637,-0.000973344357376172,
32.5633751922049));
#47979=CARTESIAN_POINT('Ctrl Pts',(-5.92197889376489,1.90929747733607,32.4730448676951));
#47980=CARTESIAN_POINT('Ctrl Pts',(-4.9145647186513,3.82350469477119,32.3827145431853));
#47981=CARTESIAN_POINT('Ctrl Pts',(-3.33575587944999,4.89860987757141,32.2923842186756));
#47982=CARTESIAN_POINT('Ctrl Pts',(-1.7139606315819,6.00298707203011,32.1995944600988));
#47983=CARTESIAN_POINT('Ctrl Pts',(0.510767719857083,6.22194753834564,32.1068047015221));
#47984=CARTESIAN_POINT('Ctrl Pts',(2.31674730916162,5.45493610644687,32.0140149429453));
#47985=CARTESIAN_POINT('Ctrl Pts',(4.12272689846615,4.6879246745481,31.9212251843686));
#47986=CARTESIAN_POINT('Ctrl Pts',(5.50995772563631,2.93494134443502,31.8284354257918));
#47987=CARTESIAN_POINT('Ctrl Pts',(5.84136939115547,1.00102430339996,31.735645667215));
#47988=CARTESIAN_POINT('Ctrl Pts',(6.17278105667463,-0.932892737635148,
31.6428559086383));
#47989=CARTESIAN_POINT('Ctrl Pts',(5.44837356054283,-3.04774348959217,31.5500661500615));
#47990=CARTESIAN_POINT('Ctrl Pts',(4.00082302553252,-4.37230615788672,31.4572763914848));
#47991=CARTESIAN_POINT('Ctrl Pts',(2.55327249052222,-5.69686882618127,31.364486632908));
#47992=CARTESIAN_POINT('Ctrl Pts',(0.382578916633404,-6.23114341081323,
31.2716968743313));
#47993=CARTESIAN_POINT('Ctrl Pts',(-1.5143907038061,-5.72977022367835,31.1789071157545));
#47994=CARTESIAN_POINT('Ctrl Pts',(-3.41136032424556,-5.22839703654348,
31.0861173571777));
#47995=CARTESIAN_POINT('Ctrl Pts',(-5.03460599123578,-3.6913760776418,30.993327598601));
#47996=CARTESIAN_POINT('Ctrl Pts',(-5.63867010296394,-1.82456720617958,
30.9005378400242));
#47997=CARTESIAN_POINT('Ctrl Pts',(-5.82781392026467,-1.24003429110695,
30.8714836240845));
#47998=CARTESIAN_POINT('Ctrl Pts',(-5.91703374327784,-0.623167857712015,
30.8424294081447));
#47999=CARTESIAN_POINT('Ctrl Pts',(-5.9121820127379,-0.00493613606119603,
30.8133751922049));
#48000=CARTESIAN_POINT('Ctrl Pts',(-5.91763133808765,-0.00541284032780908,
30.5616248077955));
#48001=CARTESIAN_POINT('Ctrl Pts',(-5.92162492516443,-0.434913027388583,
30.5818568000191));
#48002=CARTESIAN_POINT('Ctrl Pts',(-5.87885441369386,-0.863624399853681,
30.6020887922427));
#48003=CARTESIAN_POINT('Ctrl Pts',(-5.78635930947281,-1.2813248151338,30.6223207844663));
#48004=CARTESIAN_POINT('Ctrl Pts',(-5.36206688066144,-3.19739513266305,
30.715128735682));
#48005=CARTESIAN_POINT('Ctrl Pts',(-3.89145498115216,-4.88176965830319,
30.8079366868977));
#48006=CARTESIAN_POINT('Ctrl Pts',(-2.05012826636742,-5.5606403796363,30.9007446381134));
#48007=CARTESIAN_POINT('Ctrl Pts',(-0.20880155158272,-6.23951110096938,
30.9935525893291));
#48008=CARTESIAN_POINT('Ctrl Pts',(2.00323997847749,-5.91287801799537,31.0863605405448));
#48009=CARTESIAN_POINT('Ctrl Pts',(3.56977609861613,-4.73079760145679,31.1791684917605));
#48010=CARTESIAN_POINT('Ctrl Pts',(5.13631221875486,-3.54871718491814,31.2719764429762));
#48011=CARTESIAN_POINT('Ctrl Pts',(6.05734292897206,-1.51118943481486,31.3647843941919));
#48012=CARTESIAN_POINT('Ctrl Pts',(5.90974324583908,0.445737712628944,31.4575923454076));
#48013=CARTESIAN_POINT('Ctrl Pts',(5.76214356270612,2.40266486007264,31.5504002966233));
#48014=CARTESIAN_POINT('Ctrl Pts',(4.54591348622311,4.27899140485678,31.6432082478391));
#48015=CARTESIAN_POINT('Ctrl Pts',(2.81979370250234,5.21272585271166,31.7360161990548));
#48016=CARTESIAN_POINT('Ctrl Pts',(1.09367391878148,6.14646030056659,31.8288241502705));
#48017=CARTESIAN_POINT('Ctrl Pts',(-1.14233557217731,6.13760265149206,31.9216321014862));
#48018=CARTESIAN_POINT('Ctrl Pts',(-2.86100357350615,5.19022214289383,32.0144400527019));
#48019=CARTESIAN_POINT('Ctrl Pts',(-4.57967157483495,4.24284163429563,32.1072480039176));
#48020=CARTESIAN_POINT('Ctrl Pts',(-5.78099808653392,2.35693826617388,32.2000559551333));
#48021=CARTESIAN_POINT('Ctrl Pts',(-5.91308917638543,0.398903161574089,
32.292863906349));
#48022=CARTESIAN_POINT('Ctrl Pts',(-5.92198980715467,0.266965818042131,
32.2991175401645));
#48023=CARTESIAN_POINT('Ctrl Pts',(-5.92603567684633,0.134700967265697,
32.30537117398));
#48024=CARTESIAN_POINT('Ctrl Pts',(-5.92535850276232,0.00239395280352964,
32.3116248077955));
#48025=CARTESIAN_POINT('Origin',(0.,0.,-10.));
#48026=CARTESIAN_POINT('',(-5.91511646839551,0.00542726113904934,34.3133751922049));
#48027=CARTESIAN_POINT('',(-5.91029258610688,0.00423669449690529,34.0616248077955));
#48028=CARTESIAN_POINT('',(-5.91675,-7.2459289488551E-16,-10.));
#48029=CARTESIAN_POINT('Ctrl Pts',(-5.91511646839551,0.00542726113904934,
34.3133751922049));
#48030=CARTESIAN_POINT('Ctrl Pts',(-5.91971679252729,0.518347327012361,
34.2892398443991));
#48031=CARTESIAN_POINT('Ctrl Pts',(-5.85856864434903,1.03018765930209,34.2651044965933));
#48032=CARTESIAN_POINT('Ctrl Pts',(-5.72738180236852,1.52339873632063,34.2409691487875));
#48033=CARTESIAN_POINT('Ctrl Pts',(-5.22302630296755,3.41957761603427,34.1481793902107));
#48034=CARTESIAN_POINT('Ctrl Pts',(-3.68345473553503,5.04040435330718,34.055389631634));
#48035=CARTESIAN_POINT('Ctrl Pts',(-1.81569829800748,5.64153221301962,33.9625998730572));
#48036=CARTESIAN_POINT('Ctrl Pts',(0.0520581395200725,6.24266007273206,
33.8698101144804));
#48037=CARTESIAN_POINT('Ctrl Pts',(2.24799944714261,5.82408905488403,33.7770203559037));
#48038=CARTESIAN_POINT('Ctrl Pts',(3.7636638903298,4.57804326547412,33.6842305973269));
#48039=CARTESIAN_POINT('Ctrl Pts',(5.27932833351703,3.33199747606418,33.5914408387502));
#48040=CARTESIAN_POINT('Ctrl Pts',(6.11471591226884,1.25847691509218,33.4986510801734));
#48041=CARTESIAN_POINT('Ctrl Pts',(5.88618412951617,-0.690277055505497,
33.4058613215966));
#48042=CARTESIAN_POINT('Ctrl Pts',(5.6576523467635,-2.63903102610312,33.3130715630199));
#48043=CARTESIAN_POINT('Ctrl Pts',(4.36520120250652,-4.46301840632649,33.2202818044431));
#48044=CARTESIAN_POINT('Ctrl Pts',(2.60237457617807,-5.32459318494731,33.1274920458664));
#48045=CARTESIAN_POINT('Ctrl Pts',(0.83954794984961,-6.18616796356814,33.0347022872896));
#48046=CARTESIAN_POINT('Ctrl Pts',(-1.39365415855027,-6.08533014058638,
32.9419125287129));
#48047=CARTESIAN_POINT('Ctrl Pts',(-3.07165840424395,-5.06838836984331,
32.8491227701361));
#48048=CARTESIAN_POINT('Ctrl Pts',(-4.74966264993768,-4.05144659910021,
32.7563330115594));
#48049=CARTESIAN_POINT('Ctrl Pts',(-5.87246903292514,-2.11840088059577,
32.6635432529826));
#48050=CARTESIAN_POINT('Ctrl Pts',(-5.92444115227025,-0.156981060042544,
32.5707534944058));
#48051=CARTESIAN_POINT('Ctrl Pts',(-5.92581869654681,-0.104992750122198,
32.5682940603389));
#48052=CARTESIAN_POINT('Ctrl Pts',(-5.92644393826595,-0.0529845062958709,
32.5658346262719));
#48053=CARTESIAN_POINT('Ctrl Pts',(-5.9263255902637,-0.000973344357376172,
32.5633751922049));
#48054=CARTESIAN_POINT('Ctrl Pts',(-5.92535850276232,0.00239395280352964,
32.3116248077955));
#48055=CARTESIAN_POINT('Ctrl Pts',(-5.91598597755038,-1.82882029189141,
32.3981791251957));
#48056=CARTESIAN_POINT('Ctrl Pts',(-5.00185104463509,-3.66811155632826,
32.484733442596));
#48057=CARTESIAN_POINT('Ctrl Pts',(-3.53218382246986,-4.75893105481499,
32.5712877599962));
#48058=CARTESIAN_POINT('Ctrl Pts',(-1.95633171069875,-5.92856332552653,
32.6640957112119));
#48059=CARTESIAN_POINT('Ctrl Pts',(0.258228180847425,-6.23766102587179,
32.7569036624276));
#48060=CARTESIAN_POINT('Ctrl Pts',(2.09411868220313,-5.54422350605098,32.8497116136433));
#48061=CARTESIAN_POINT('Ctrl Pts',(3.93000918355878,-4.85078598623018,32.942519564859));
#48062=CARTESIAN_POINT('Ctrl Pts',(5.38723029472394,-3.15481324624327,33.0353275160747));
#48063=CARTESIAN_POINT('Ctrl Pts',(5.79632913896631,-1.23544156194066,33.1281354672904));
#48064=CARTESIAN_POINT('Ctrl Pts',(6.20542798320869,0.68393012236201,33.2209434185061));
#48065=CARTESIAN_POINT('Ctrl Pts',(5.56640456052833,2.82670075098039,33.3137513697218));
#48066=CARTESIAN_POINT('Ctrl Pts',(4.17282864241345,4.20847341220712,33.4065593209376));
#48067=CARTESIAN_POINT('Ctrl Pts',(2.77925272429858,5.59024607343385,33.4993672721533));
#48068=CARTESIAN_POINT('Ctrl Pts',(0.631124310749118,6.21102076726887,33.592175223369));
#48069=CARTESIAN_POINT('Ctrl Pts',(-1.28469829991443,5.78561125710995,33.6849831745847));
#48070=CARTESIAN_POINT('Ctrl Pts',(-3.20052091057798,5.36020174695103,33.7777911258004));
#48071=CARTESIAN_POINT('Ctrl Pts',(-4.88403771835562,3.88860803279828,33.8705990770161));
#48072=CARTESIAN_POINT('Ctrl Pts',(-5.56183474965175,2.04688581942584,33.9634070282318));
#48073=CARTESIAN_POINT('Ctrl Pts',(-5.80093681844618,1.39719340262678,33.9961462880864));
#48074=CARTESIAN_POINT('Ctrl Pts',(-5.91488500290352,0.701441416885687,
34.0288855479409));
#48075=CARTESIAN_POINT('Ctrl Pts',(-5.91029258610688,0.00423669449690529,
34.0616248077955));
#48076=CARTESIAN_POINT('Origin',(0.,0.,-10.));
#48077=CARTESIAN_POINT('',(-5.90729969700522,-0.00151050143465004,36.0633751922049));
#48078=CARTESIAN_POINT('',(-5.90990876146918,-0.00403960103504912,35.8116248077955));
#48079=CARTESIAN_POINT('',(-5.91675,-7.2459289488551E-16,-10.));
#48080=CARTESIAN_POINT('Ctrl Pts',(-5.90729969700522,-0.00151050143465004,
36.0633751922049));
#48081=CARTESIAN_POINT('Ctrl Pts',(-5.90483716507214,1.08019297671428,36.0126450625263));
#48082=CARTESIAN_POINT('Ctrl Pts',(-5.62097754735415,2.16309938757096,35.9619149328477));
#48083=CARTESIAN_POINT('Ctrl Pts',(-5.06355200594223,3.07962450682608,35.9111848031691));
#48084=CARTESIAN_POINT('Ctrl Pts',(-4.04397287732933,4.7560275652059,35.8183950445923));
#48085=CARTESIAN_POINT('Ctrl Pts',(-2.109163966812,5.87579289923287,35.7256052860156));
#48086=CARTESIAN_POINT('Ctrl Pts',(-0.147664846514664,5.92468067603893,
35.6328155274388));
#48087=CARTESIAN_POINT('Ctrl Pts',(1.81383427378267,5.97356845284499,35.5400257688621));
#48088=CARTESIAN_POINT('Ctrl Pts',(3.80202360386,4.95157867243014,35.4472360102853));
#48089=CARTESIAN_POINT('Ctrl Pts',(4.90384920487803,3.32804882712716,35.3544462517086));
#48090=CARTESIAN_POINT('Ctrl Pts',(6.00567480589603,1.70451898182423,35.2616564931318));
#48091=CARTESIAN_POINT('Ctrl Pts',(6.22113667785476,-0.520550928366797,
35.168866734555));
#48092=CARTESIAN_POINT('Ctrl Pts',(5.45128634140899,-2.32532218066509,35.0760769759783));
#48093=CARTESIAN_POINT('Ctrl Pts',(4.68143600496318,-4.13009343296349,34.9832872174015));
#48094=CARTESIAN_POINT('Ctrl Pts',(2.92627346011274,-5.51456602736912,34.8904974588247));
#48095=CARTESIAN_POINT('Ctrl Pts',(0.991837674392355,-5.84293625222638,
34.797707700248));
#48096=CARTESIAN_POINT('Ctrl Pts',(-0.942598111327868,-6.17130647708362,
34.7049179416712));
#48097=CARTESIAN_POINT('Ctrl Pts',(-3.05630713791801,-5.4435743323927,34.6121281830945));
#48098=CARTESIAN_POINT('Ctrl Pts',(-4.37859193552841,-3.99394274897012,
34.5193384245177));
#48099=CARTESIAN_POINT('Ctrl Pts',(-5.35694003173801,-2.92137177000263,
34.4506840137468));
#48100=CARTESIAN_POINT('Ctrl Pts',(-5.9020305768988,-1.45360391497842,34.3820296029759));
#48101=CARTESIAN_POINT('Ctrl Pts',(-5.91511646839551,0.00542726113904934,
34.3133751922049));
#48102=CARTESIAN_POINT('Ctrl Pts',(-5.91029258610688,0.00423669449690529,
34.0616248077955));
#48103=CARTESIAN_POINT('Ctrl Pts',(-5.90186660249012,-1.27496678996694,
34.1216934991566));
#48104=CARTESIAN_POINT('Ctrl Pts',(-5.49439205420357,-2.55906068723431,
34.1817621905178));
#48105=CARTESIAN_POINT('Ctrl Pts',(-4.72871546052388,-3.57253375541824,
34.2418308818789));
#48106=CARTESIAN_POINT('Ctrl Pts',(-3.54572188528532,-5.13838040429787,
34.3346388330947));
#48107=CARTESIAN_POINT('Ctrl Pts',(-1.5076574799935,-6.05822298946509,34.4274467843104));
#48108=CARTESIAN_POINT('Ctrl Pts',(0.449183277708752,-5.90948235662204,
34.5202547355261));
#48109=CARTESIAN_POINT('Ctrl Pts',(2.406024035411,-5.760741723779,34.6130626867418));
#48110=CARTESIAN_POINT('Ctrl Pts',(4.28164114552377,-4.54341787292579,34.7058706379575));
#48111=CARTESIAN_POINT('Ctrl Pts',(5.21436903074208,-2.81675397424735,34.7986785891732));
#48112=CARTESIAN_POINT('Ctrl Pts',(6.1470969159604,-1.0900900755689,34.8914865403889));
#48113=CARTESIAN_POINT('Ctrl Pts',(6.13693557628423,1.14591387093472,34.9842944916046));
#48114=CARTESIAN_POINT('Ctrl Pts',(5.18855316950071,2.86402921553961,35.0771024428203));
#48115=CARTESIAN_POINT('Ctrl Pts',(4.2401707627172,4.58214456014451,35.1699103940361));
#48116=CARTESIAN_POINT('Ctrl Pts',(2.35356728882637,5.7823713028506,35.2627183452517));
#48117=CARTESIAN_POINT('Ctrl Pts',(0.395455502105646,5.91332074946512,35.3555262964675));
#48118=CARTESIAN_POINT('Ctrl Pts',(-1.56265628461502,6.04427019607964,35.4483342476832));
#48119=CARTESIAN_POINT('Ctrl Pts',(-3.59227638416566,5.10594234660255,35.5411421988989));
#48120=CARTESIAN_POINT('Ctrl Pts',(-4.76098966482233,3.52940855550265,35.6339501501146));
#48121=CARTESIAN_POINT('Ctrl Pts',(-5.5067976455242,2.52335214910344,35.6931750360082));
#48122=CARTESIAN_POINT('Ctrl Pts',(-5.90201989047548,1.25740013647395,35.7523999219019));
#48123=CARTESIAN_POINT('Ctrl Pts',(-5.90990876146918,-0.00403960103504912,
35.8116248077955));
#48124=CARTESIAN_POINT('Origin',(0.,0.,-10.));
#48125=CARTESIAN_POINT('',(-5.92067510213246,-0.00487139356358524,37.8133751922049));
#48126=CARTESIAN_POINT('',(-5.92504705000468,-0.0026864220054185,37.5616248077955));
#48127=CARTESIAN_POINT('',(-5.91675,-7.2459289488551E-16,-10.));
#48128=CARTESIAN_POINT('Ctrl Pts',(-5.92067510213246,-0.00487139356358524,
37.8133751922049));
#48129=CARTESIAN_POINT('Ctrl Pts',(-5.90611554008262,1.63446818848114,37.7360502806535));
#48130=CARTESIAN_POINT('Ctrl Pts',(-5.19681189997422,3.28486223478748,37.6587253691021));
#48131=CARTESIAN_POINT('Ctrl Pts',(-3.98705259670286,4.38486688635475,37.5814004575507));
#48132=CARTESIAN_POINT('Ctrl Pts',(-2.53534354932926,5.70487054370628,37.4886106989739));
#48133=CARTESIAN_POINT('Ctrl Pts',(-0.362980448390255,6.23231578369225,
37.3958209403972));
#48134=CARTESIAN_POINT('Ctrl Pts',(1.53240300197176,5.72497921913026,37.3030311818204));
#48135=CARTESIAN_POINT('Ctrl Pts',(3.42778645233388,5.21764265456824,37.2102414232437));
#48136=CARTESIAN_POINT('Ctrl Pts',(5.04619025211903,3.67552428545812,37.1174516646669));
#48137=CARTESIAN_POINT('Ctrl Pts',(5.64438037342458,1.80682490021162,37.0246619060902));
#48138=CARTESIAN_POINT('Ctrl Pts',(6.24257049473012,-0.0618744850348207,
36.9318721475134));
#48139=CARTESIAN_POINT('Ctrl Pts',(5.82054693755619,-2.25715488641753,36.8390823889367));
#48140=CARTESIAN_POINT('Ctrl Pts',(4.57211934836416,-3.77085808328017,36.7462926303599));
#48141=CARTESIAN_POINT('Ctrl Pts',(3.32369175917207,-5.2845612801429,36.6535028717831));
#48142=CARTESIAN_POINT('Ctrl Pts',(1.24886013796173,-6.11668727248533,36.5607131132064));
#48143=CARTESIAN_POINT('Ctrl Pts',(-0.699532063430729,-5.88509141068834,
36.4679233546296));
#48144=CARTESIAN_POINT('Ctrl Pts',(-2.64792426482302,-5.65349554889138,
36.3751335960529));
#48145=CARTESIAN_POINT('Ctrl Pts',(-4.4698770463975,-4.35817783295517,36.2823438374761));
#48146=CARTESIAN_POINT('Ctrl Pts',(-5.32867876383053,-2.59399858362084,
36.1895540788994));
#48147=CARTESIAN_POINT('Ctrl Pts',(-5.71795536166166,-1.79433355943125,
36.1474944500012));
#48148=CARTESIAN_POINT('Ctrl Pts',(-5.90934134720228,-0.898335468313729,
36.105434821103));
#48149=CARTESIAN_POINT('Ctrl Pts',(-5.90729969700522,-0.00151050143465004,
36.0633751922049));
#48150=CARTESIAN_POINT('Ctrl Pts',(-5.90990876146918,-0.00403960103504912,
35.8116248077955));
#48151=CARTESIAN_POINT('Ctrl Pts',(-5.91438209165634,-0.719330351965569,
35.8452078731176));
#48152=CARTESIAN_POINT('Ctrl Pts',(-5.79431305298316,-1.43317023532246,
35.8787909384397));
#48153=CARTESIAN_POINT('Ctrl Pts',(-5.54300160018766,-2.09735085298511,
35.9123740037618));
#48154=CARTESIAN_POINT('Ctrl Pts',(-4.8484937931335,-3.93283673765,36.0051819549775));
#48155=CARTESIAN_POINT('Ctrl Pts',(-3.15167171726243,-5.38906877425699,
36.0979899061931));
#48156=CARTESIAN_POINT('Ctrl Pts',(-1.23206183653459,-5.79704847065775,
36.1907978574088));
#48157=CARTESIAN_POINT('Ctrl Pts',(0.687548044193256,-6.20502816705852,
36.2836058086245));
#48158=CARTESIAN_POINT('Ctrl Pts',(2.82994572977787,-5.56475552325307,36.3764137598403));
#48159=CARTESIAN_POINT('Ctrl Pts',(4.21090563994866,-4.170374207628,36.469221711056));
#48160=CARTESIAN_POINT('Ctrl Pts',(5.59186555011949,-2.7759928920029,36.5620296622717));
#48161=CARTESIAN_POINT('Ctrl Pts',(6.21138768487646,-0.627502904558124,
36.6548376134874));
#48162=CARTESIAN_POINT('Ctrl Pts',(5.78486123798388,1.28807134797416,36.7476455647031));
#48163=CARTESIAN_POINT('Ctrl Pts',(5.35833479109132,3.2036456005064,36.8404535159188));
#48164=CARTESIAN_POINT('Ctrl Pts',(3.88575976254927,4.88630411812616,36.9332614671345));
#48165=CARTESIAN_POINT('Ctrl Pts',(2.04364267666501,5.56302722897469,37.0260694183503));
#48166=CARTESIAN_POINT('Ctrl Pts',(0.201525590780754,6.23975033982323,37.118877369566));
#48167=CARTESIAN_POINT('Ctrl Pts',(-2.01013355244571,5.91053804390054,37.2116853207817));
#48168=CARTESIAN_POINT('Ctrl Pts',(-3.57529019777168,4.72663171210939,37.3044932719974));
#48169=CARTESIAN_POINT('Ctrl Pts',(-5.02075231139987,3.63326399469971,37.3902037839301));
#48170=CARTESIAN_POINT('Ctrl Pts',(-5.91481283469339,1.81092824985332,37.4759142958628));
#48171=CARTESIAN_POINT('Ctrl Pts',(-5.92504705000468,-0.0026864220054185,
37.5616248077955));
#48172=CARTESIAN_POINT('Origin',(0.,0.,-10.));
#48173=CARTESIAN_POINT('',(-5.92317748384162,0.00391648730000096,39.5633751922049));
#48174=CARTESIAN_POINT('',(-5.91817991048888,0.00535877289898346,39.3116248077955));
#48175=CARTESIAN_POINT('',(-5.91675,-7.2459289488551E-16,-10.));
#48176=CARTESIAN_POINT('Ctrl Pts',(-5.92317748384162,0.00391648730000096,
39.5633751922049));
#48177=CARTESIAN_POINT('Ctrl Pts',(-5.92497651525942,0.239619045790868,
39.5522452573574));
#48178=CARTESIAN_POINT('Ctrl Pts',(-5.91213103375526,0.475123798574987,
39.54111532251));
#48179=CARTESIAN_POINT('Ctrl Pts',(-5.88398413996813,0.708785341643609,
39.5299853876626));
#48180=CARTESIAN_POINT('Ctrl Pts',(-5.64932477178711,2.65681095609875,39.4371956290858));
#48181=CARTESIAN_POINT('Ctrl Pts',(-4.35114368706545,4.47672463393544,39.3444058705091));
#48182=CARTESIAN_POINT('Ctrl Pts',(-2.58561617695903,5.33275116664683,39.2516161119323));
#48183=CARTESIAN_POINT('Ctrl Pts',(-0.820088666852756,6.18877769935815,
39.1588263533556));
#48184=CARTESIAN_POINT('Ctrl Pts',(1.41278526863818,6.08091708694438,39.0660365947788));
#48185=CARTESIAN_POINT('Ctrl Pts',(3.08758299451145,5.05870312154499,38.973246836202));
#48186=CARTESIAN_POINT('Ctrl Pts',(4.76238072038482,4.03648915614554,38.8804570776253));
#48187=CARTESIAN_POINT('Ctrl Pts',(5.87910223664044,2.09992183776038,38.7876673190485));
#48188=CARTESIAN_POINT('Ctrl Pts',(5.92490555002402,0.138348267860097,38.6948775604718));
#48189=CARTESIAN_POINT('Ctrl Pts',(5.9707088634076,-1.82322530204013,38.602087801895));
#48190=CARTESIAN_POINT('Ctrl Pts',(4.94559397391919,-3.80980512345547,38.5092980433183));
#48191=CARTESIAN_POINT('Ctrl Pts',(3.3203335456359,-4.909076406581,38.4165082847415));
#48192=CARTESIAN_POINT('Ctrl Pts',(1.69507311735257,-6.00834768970656,38.3237185261647));
#48193=CARTESIAN_POINT('Ctrl Pts',(-0.53033284972568,-6.22031043454227,
38.230928767588));
#48194=CARTESIAN_POINT('Ctrl Pts',(-2.33389130241298,-5.44762309713571,
38.1381390090112));
#48195=CARTESIAN_POINT('Ctrl Pts',(-4.13744975510023,-4.67493575972916,
38.0453492504345));
#48196=CARTESIAN_POINT('Ctrl Pts',(-5.51916069339655,-2.9175983400804,37.9525594918577));
#48197=CARTESIAN_POINT('Ctrl Pts',(-5.84448866564066,-0.982648592897399,
37.859769733281));
#48198=CARTESIAN_POINT('Ctrl Pts',(-5.89870959908197,-0.660159319286536,
37.8443048862556));
#48199=CARTESIAN_POINT('Ctrl Pts',(-5.92358698906954,-0.33273644184221,
37.8288400392302));
#48200=CARTESIAN_POINT('Ctrl Pts',(-5.92067510213246,-0.00487139356358524,
37.8133751922049));
#48201=CARTESIAN_POINT('Ctrl Pts',(-5.92504705000468,-0.0026864220054185,
37.5616248077955));
#48202=CARTESIAN_POINT('Ctrl Pts',(-5.92589451573722,-0.152866600912679,
37.5687222470785));
#48203=CARTESIAN_POINT('Ctrl Pts',(-5.92068156990396,-0.302986979278675,
37.5758196863615));
#48204=CARTESIAN_POINT('Ctrl Pts',(-5.90921945853301,-0.452628690092833,
37.5829171256445));
#48205=CARTESIAN_POINT('Ctrl Pts',(-5.75933792654291,-2.40938239284423,
37.6757250768602));
#48206=CARTESIAN_POINT('Ctrl Pts',(-4.54092071513729,-4.28428943068747,
37.7685330280759));
#48207=CARTESIAN_POINT('Ctrl Pts',(-2.81371328846423,-5.2160104361974,37.8613409792916));
#48208=CARTESIAN_POINT('Ctrl Pts',(-1.08650586179102,-6.14773144170741,
37.9541489305073));
#48209=CARTESIAN_POINT('Ctrl Pts',(1.14949178014972,-6.13626641488391,38.046956881723));
#48210=CARTESIAN_POINT('Ctrl Pts',(2.86705388397389,-5.18688243230851,38.1397648329388));
#48211=CARTESIAN_POINT('Ctrl Pts',(4.58461598779797,-4.23749844973315,38.2325727841545));
#48212=CARTESIAN_POINT('Ctrl Pts',(5.78374255350553,-2.35019551140599,38.3253807353702));
#48213=CARTESIAN_POINT('Ctrl Pts',(5.913550312368,-0.392007708205717,38.4181886865859));
#48214=CARTESIAN_POINT('Ctrl Pts',(6.04335807123046,1.56618009499456,38.5109966378016));
#48215=CARTESIAN_POINT('Ctrl Pts',(5.10384702324784,3.59525276306796,38.6038045890173));
#48216=CARTESIAN_POINT('Ctrl Pts',(3.52663208874664,4.76304665637687,38.696612540233));
#48217=CARTESIAN_POINT('Ctrl Pts',(1.94941715424539,5.93084054968582,38.7894204914487));
#48218=CARTESIAN_POINT('Ctrl Pts',(-0.265501666774463,6.23735566823023,
38.8822284426645));
#48219=CARTESIAN_POINT('Ctrl Pts',(-2.10058231079274,5.54177781003398,38.9750363938802));
#48220=CARTESIAN_POINT('Ctrl Pts',(-3.93566295481097,4.84619995183775,39.0678443450959));
#48221=CARTESIAN_POINT('Ctrl Pts',(-5.39090542182765,3.1485291169009,39.1606522963116));
#48222=CARTESIAN_POINT('Ctrl Pts',(-5.79776583169802,1.22868169230088,39.2534602475273));
#48223=CARTESIAN_POINT('Ctrl Pts',(-5.88276162685228,0.827613034672763,
39.2728484342833));
#48224=CARTESIAN_POINT('Ctrl Pts',(-5.92200399834135,0.416848160320931,
39.2922366210394));
#48225=CARTESIAN_POINT('Ctrl Pts',(-5.91817991048888,0.00535877289898346,
39.3116248077955));
#48226=CARTESIAN_POINT('Origin',(0.,0.,-10.));
#48227=CARTESIAN_POINT('',(-5.9083370126323,0.00290647373917707,41.3133751922049));
#48228=CARTESIAN_POINT('',(-5.90694375459152,0.000187200592619384,41.0616248077955));
#48229=CARTESIAN_POINT('',(-5.91675,-7.2459289488551E-16,-10.));
#48230=CARTESIAN_POINT('Ctrl Pts',(-5.9083370126323,0.00290647373917707,
41.3133751922049));
#48231=CARTESIAN_POINT('Ctrl Pts',(-5.9118961055199,0.806946743982272,41.2756504754847));
#48232=CARTESIAN_POINT('Ctrl Pts',(-5.75924372095175,1.60969263292704,41.2379257587644));
#48233=CARTESIAN_POINT('Ctrl Pts',(-5.44394638268512,2.34245465321636,41.2002010420442));
#48234=CARTESIAN_POINT('Ctrl Pts',(-4.66842395491908,4.1447958466867,41.1074112834675));
#48235=CARTESIAN_POINT('Ctrl Pts',(-2.90891600578834,5.52374171235785,41.0146215248907));
#48236=CARTESIAN_POINT('Ctrl Pts',(-0.973457081635854,5.84602662755981,
40.9218317663139));
#48237=CARTESIAN_POINT('Ctrl Pts',(0.962001842516637,6.16831154276178,40.8290420077372));
#48238=CARTESIAN_POINT('Ctrl Pts',(3.07341174169088,5.43393550749457,40.7362522491604));
#48239=CARTESIAN_POINT('Ctrl Pts',(4.39113099484952,3.98015258576819,40.6434624905837));
#48240=CARTESIAN_POINT('Ctrl Pts',(5.70885024800813,2.52636966404185,40.5506727320069));
#48241=CARTESIAN_POINT('Ctrl Pts',(6.23287885515117,0.353179855856394,40.4578829734301));
#48242=CARTESIAN_POINT('Ctrl Pts',(5.72256247990427,-1.54140347849522,40.3650932148534));
#48243=CARTESIAN_POINT('Ctrl Pts',(5.21224610465735,-3.4359868128469,40.2723034562766));
#48244=CARTESIAN_POINT('Ctrl Pts',(3.66758474702043,-5.05196367336471,40.1795136976999));
#48245=CARTESIAN_POINT('Ctrl Pts',(1.79794703473299,-5.64721457713625,40.0867239391231));
#48246=CARTESIAN_POINT('Ctrl Pts',(-0.0716906775543941,-6.24246548090778,
39.9939341805464));
#48247=CARTESIAN_POINT('Ctrl Pts',(-2.26630474449228,-5.81699042793309,
39.9011444219696));
#48248=CARTESIAN_POINT('Ctrl Pts',(-3.77804295214096,-4.566184125909,39.8083546633928));
#48249=CARTESIAN_POINT('Ctrl Pts',(-5.10845136633424,-3.46540938837883,
39.7266948396635));
#48250=CARTESIAN_POINT('Ctrl Pts',(-5.90997807248162,-1.72542242103686,
39.6450350159342));
#48251=CARTESIAN_POINT('Ctrl Pts',(-5.92317748384162,0.00391648730000096,
39.5633751922049));
#48252=CARTESIAN_POINT('Ctrl Pts',(-5.91817991048888,0.00535877289898346,
39.3116248077955));
#48253=CARTESIAN_POINT('Ctrl Pts',(-5.90369874043758,-1.55288152477645,
39.3850445722551));
#48254=CARTESIAN_POINT('Ctrl Pts',(-5.27164108271407,-3.1215113980975,39.4584643367148));
#48255=CARTESIAN_POINT('Ctrl Pts',(-4.16791835516374,-4.21333643623311,
39.5318841011744));
#48256=CARTESIAN_POINT('Ctrl Pts',(-2.77273211603503,-5.59348312590389,
39.6246920523901));
#48257=CARTESIAN_POINT('Ctrl Pts',(-0.623881285053837,-6.21175249098218,
39.7175000036058));
#48258=CARTESIAN_POINT('Ctrl Pts',(1.29144395816604,-5.78410925234965,39.8103079548215));
#48259=CARTESIAN_POINT('Ctrl Pts',(3.20676920138586,-5.35646601371713,39.9031159060372));
#48260=CARTESIAN_POINT('Ctrl Pts',(4.88856885684424,-3.88291017137353,39.9959238572529));
#48261=CARTESIAN_POINT('Ctrl Pts',(5.56421781719968,-2.04039883918756,40.0887318084687));
#48262=CARTESIAN_POINT('Ctrl Pts',(6.23986677755516,-0.197887507001491,
40.1815397596844));
#48263=CARTESIAN_POINT('Ctrl Pts',(5.90936504280782,2.01357931502706,40.2743477109001));
#48264=CARTESIAN_POINT('Ctrl Pts',(4.72454635692166,3.57804542473942,40.3671556621158));
#48265=CARTESIAN_POINT('Ctrl Pts',(3.53972767103556,5.14251153445169,40.4599636133315));
#48266=CARTESIAN_POINT('Ctrl Pts',(1.50059203401065,6.05997693184778,40.5527715645472));
#48267=CARTESIAN_POINT('Ctrl Pts',(-0.456073948610288,5.90895455166135,
40.6455795157629));
#48268=CARTESIAN_POINT('Ctrl Pts',(-2.41273993123128,5.75793217147491,40.7383874669786));
#48269=CARTESIAN_POINT('Ctrl Pts',(-4.28693625944829,4.538422013706,40.8311954181944));
#48270=CARTESIAN_POINT('Ctrl Pts',(-5.2176500685201,2.81067164618575,40.9240033694101));
#48271=CARTESIAN_POINT('Ctrl Pts',(-5.67769029658167,1.95666618783744,40.9698771822052));
#48272=CARTESIAN_POINT('Ctrl Pts',(-5.90721872419092,0.978487399899294,
41.0157509950003));
#48273=CARTESIAN_POINT('Ctrl Pts',(-5.90694375459152,0.000187200592619384,
41.0616248077955));
#48274=CARTESIAN_POINT('Origin',(0.,0.,-10.));
#48275=CARTESIAN_POINT('',(-5.91250905277058,-0.00502274925685997,43.0633751922049));
#48276=CARTESIAN_POINT('',(-5.91749050086513,-0.0054238502176924,42.8116248077955));
#48277=CARTESIAN_POINT('',(-5.91675,-7.2459289488551E-16,-10.));
#48278=CARTESIAN_POINT('Ctrl Pts',(-5.91250905277058,-0.00502274925685997,
43.0633751922049));
#48279=CARTESIAN_POINT('Ctrl Pts',(-5.9015374759735,1.3634120868958,42.9990556936118));
#48280=CARTESIAN_POINT('Ctrl Pts',(-5.42891142018307,2.73868470796129,42.9347361950188));
#48281=CARTESIAN_POINT('Ctrl Pts',(-4.5602376127848,3.78521847914597,42.8704166964258));
#48282=CARTESIAN_POINT('Ctrl Pts',(-3.30705569076064,5.29498795955015,42.777626937849));
#48283=CARTESIAN_POINT('Ctrl Pts',(-1.2296173434281,6.12058461442322,42.6848371792723));
#48284=CARTESIAN_POINT('Ctrl Pts',(0.718036867263995,5.88286232009343,42.5920474206956));
#48285=CARTESIAN_POINT('Ctrl Pts',(2.66569107795615,5.64514002576363,42.4992576621188));
#48286=CARTESIAN_POINT('Ctrl Pts',(4.48356115200779,4.34409878223093,42.406467903542));
#48287=CARTESIAN_POINT('Ctrl Pts',(5.336810383326,2.57722737692063,42.3136781449652));
#48288=CARTESIAN_POINT('Ctrl Pts',(6.19005961464416,0.810355971610422,42.2208883863885));
#48289=CARTESIAN_POINT('Ctrl Pts',(6.07868800322892,-1.42234559547743,42.1280986278118));
#48290=CARTESIAN_POINT('Ctrl Pts',(5.05384172864138,-3.09553384762119,42.035308869235));
#48291=CARTESIAN_POINT('Ctrl Pts',(4.02899545405375,-4.7687220997651,41.9425191106583));
#48292=CARTESIAN_POINT('Ctrl Pts',(2.09067451629372,-5.88239703696494,41.8497293520815));
#48293=CARTESIAN_POINT('Ctrl Pts',(0.129031347115672,-5.92511577366947,
41.7569395935047));
#48294=CARTESIAN_POINT('Ctrl Pts',(-1.83261182206221,-5.96783451037401,
41.6641498349279));
#48295=CARTESIAN_POINT('Ctrl Pts',(-3.81757722265803,-4.93959704658343,
41.5713600763512));
#48296=CARTESIAN_POINT('Ctrl Pts',(-4.91429146975527,-3.31261005405344,
41.4785703177745));
#48297=CARTESIAN_POINT('Ctrl Pts',(-5.56512424319231,-2.34709286532634,
41.4235052759179));
#48298=CARTESIAN_POINT('Ctrl Pts',(-5.9031419676892,-1.17071429758749,41.3684402340614));
#48299=CARTESIAN_POINT('Ctrl Pts',(-5.9083370126323,0.00290647373917707,
41.3133751922049));
#48300=CARTESIAN_POINT('Ctrl Pts',(-5.90694375459152,0.000187200592619384,
41.0616248077955));
#48301=CARTESIAN_POINT('Ctrl Pts',(-5.9066624293549,-1.00072539361877,41.108558946216));
#48302=CARTESIAN_POINT('Ctrl Pts',(-5.66583159864754,-2.00176507665916,
41.1554930846366));
#48303=CARTESIAN_POINT('Ctrl Pts',(-5.18520993188531,-2.87007757778048,
41.2024272230572));
#48304=CARTESIAN_POINT('Ctrl Pts',(-4.23482469625214,-4.58708585695503,
41.2952351742729));
#48305=CARTESIAN_POINT('Ctrl Pts',(-2.34682293505921,-5.78511183803251,
41.3880431254886));
#48306=CARTESIAN_POINT('Ctrl Pts',(-0.388559781046523,-5.91377786501602,
41.4808510767043));
#48307=CARTESIAN_POINT('Ctrl Pts',(1.56970337296606,-6.04244389199952,41.57365902792));
#48308=CARTESIAN_POINT('Ctrl Pts',(3.59822791979854,-5.10174996488907,41.6664669791358));
#48309=CARTESIAN_POINT('Ctrl Pts',(4.76510202877927,-3.52385442314578,41.7592749303515));
#48310=CARTESIAN_POINT('Ctrl Pts',(5.93197613776004,-1.94595888140243,41.8520828815672));
#48311=CARTESIAN_POINT('Ctrl Pts',(6.23719980888921,0.269138274973701,41.9448908327828));
#48312=CARTESIAN_POINT('Ctrl Pts',(5.54055213600606,2.1038130545272,42.0376987839985));
#48313=CARTESIAN_POINT('Ctrl Pts',(4.84390446312288,3.93848783408075,42.1305067352143));
#48314=CARTESIAN_POINT('Ctrl Pts',(3.14538544622723,5.3927402368115,42.22331468643));
#48315=CARTESIAN_POINT('Ctrl Pts',(1.22530113038875,5.79848122184322,42.3161226376457));
#48316=CARTESIAN_POINT('Ctrl Pts',(-0.694783185449667,6.20422220687492,
42.4089305888614));
#48317=CARTESIAN_POINT('Ctrl Pts',(-2.83643280023093,5.56145177420767,42.5017385400771));
#48318=CARTESIAN_POINT('Ctrl Pts',(-4.21576580023403,4.16546108585562,42.5945464912928));
#48319=CARTESIAN_POINT('Ctrl Pts',(-5.29118833179891,3.07705107891373,42.666905930127));
#48320=CARTESIAN_POINT('Ctrl Pts',(-5.90321154071277,1.53077127151761,42.7392653689613));
#48321=CARTESIAN_POINT('Ctrl Pts',(-5.91749050086513,-0.0054238502176924,
42.8116248077955));
#48322=CARTESIAN_POINT('Origin',(0.,0.,-10.));
#48323=CARTESIAN_POINT('',(-5.92640592629062,-0.000744257410045246,44.8133751922049));
#48324=CARTESIAN_POINT('',(-5.92543336817915,0.00231728688185692,44.5616248077955));
#48325=CARTESIAN_POINT('',(-5.91675,-7.2459289488551E-16,-10.));
#48326=CARTESIAN_POINT('Ctrl Pts',(-5.92640592629062,-0.000744257410045246,
44.8133751922049));
#48327=CARTESIAN_POINT('Ctrl Pts',(-5.92300951336607,1.92180582290993,44.7224609117391));
#48328=CARTESIAN_POINT('Ctrl Pts',(-4.9006682261132,3.84745506871863,44.6315466312733));
#48329=CARTESIAN_POINT('Ctrl Pts',(-3.30487837147756,4.9194943815056,44.5406323508074));
#48330=CARTESIAN_POINT('Ctrl Pts',(-1.67616883770366,6.01364888076154,44.4478425922307));
#48331=CARTESIAN_POINT('Ctrl Pts',(0.549892734243904,6.21861180766247,44.3550528336539));
#48332=CARTESIAN_POINT('Ctrl Pts',(2.35101221190118,5.44025620714841,44.2622630750772));
#48333=CARTESIAN_POINT('Ctrl Pts',(4.15213168955856,4.66190060663431,44.1694733165004));
#48334=CARTESIAN_POINT('Ctrl Pts',(5.52830907292561,2.90022647870511,44.0766835579236));
#48335=CARTESIAN_POINT('Ctrl Pts',(5.84755013418095,0.964263163335458,43.9838937993469));
#48336=CARTESIAN_POINT('Ctrl Pts',(6.16679119543626,-0.971700152034025,
43.8911040407701));
#48337=CARTESIAN_POINT('Ctrl Pts',(5.42909593457998,-3.08195265484406,43.7983142821934));
#48338=CARTESIAN_POINT('Ctrl Pts',(3.9732427332272,-4.39738424552399,43.7055245236166));
#48339=CARTESIAN_POINT('Ctrl Pts',(2.51738953187434,-5.71281583620399,43.6127347650398));
#48340=CARTESIAN_POINT('Ctrl Pts',(0.343378390025083,-6.23342651475394,
43.5199450064631));
#48341=CARTESIAN_POINT('Ctrl Pts',(-1.55040014363566,-5.72013159066641,
43.4271552478863));
#48342=CARTESIAN_POINT('Ctrl Pts',(-3.44417867729635,-5.20683666657891,
43.3343654893096));
#48343=CARTESIAN_POINT('Ctrl Pts',(-5.05772460276838,-3.65963613985392,
43.2415757307328));
#48344=CARTESIAN_POINT('Ctrl Pts',(-5.65003481714654,-1.78906472352378,
43.1487859721561));
#48345=CARTESIAN_POINT('Ctrl Pts',(-5.8317706687429,-1.2151257958025,43.1203157121723));
#48346=CARTESIAN_POINT('Ctrl Pts',(-5.91736549056436,-0.610744130926478,
43.0918454521886));
#48347=CARTESIAN_POINT('Ctrl Pts',(-5.91250905277058,-0.00502274925685997,
43.0633751922049));
#48348=CARTESIAN_POINT('Ctrl Pts',(-5.91749050086513,-0.0054238502176924,
42.8116248077955));
#48349=CARTESIAN_POINT('Ctrl Pts',(-5.92152568270421,-0.439546964952688,
42.832073320177));
#48350=CARTESIAN_POINT('Ctrl Pts',(-5.87782459649013,-0.872864709734026,
42.8525218325585));
#48351=CARTESIAN_POINT('Ctrl Pts',(-5.7833553004627,-1.29481612934438,42.87297034494));
#48352=CARTESIAN_POINT('Ctrl Pts',(-5.35459541546329,-3.20989171215526,
42.9657782961557));
#48353=CARTESIAN_POINT('Ctrl Pts',(-3.88005926023967,-4.8908319337401,43.0585862473713));
#48354=CARTESIAN_POINT('Ctrl Pts',(-2.03715430809605,-5.56540651392206,
43.1513941985871));
#48355=CARTESIAN_POINT('Ctrl Pts',(-0.194249355952331,-6.23998109410406,
43.2442021498028));
#48356=CARTESIAN_POINT('Ctrl Pts',(2.01702439311145,-5.90819003288294,43.3370101010186));
#48357=CARTESIAN_POINT('Ctrl Pts',(3.58079943538484,-4.72245939566959,43.4298180522343));
#48358=CARTESIAN_POINT('Ctrl Pts',(5.1445744776582,-3.53672875845627,43.52262600345));
#48359=CARTESIAN_POINT('Ctrl Pts',(6.06085081314126,-1.49705854525084,43.6154339546656));
#48360=CARTESIAN_POINT('Ctrl Pts',(5.90868763609711,0.459519052089763,43.7082419058814));
#48361=CARTESIAN_POINT('Ctrl Pts',(5.75652445905297,2.41609664943031,43.8010498570971));
#48362=CARTESIAN_POINT('Ctrl Pts',(4.53592176948156,4.28958163090607,43.8938578083128));
#48363=CARTESIAN_POINT('Ctrl Pts',(2.80762904844648,5.21928792715251,43.9866657595285));
#48364=CARTESIAN_POINT('Ctrl Pts',(1.07933632741135,6.14899422339897,44.0794737107442));
#48365=CARTESIAN_POINT('Ctrl Pts',(-1.15664642508744,6.13492183441616,44.1722816619599));
#48366=CARTESIAN_POINT('Ctrl Pts',(-2.8731002959318,5.18353566879953,44.2650896131756));
#48367=CARTESIAN_POINT('Ctrl Pts',(-4.58955416677612,4.23214950318292,44.3578975643913));
#48368=CARTESIAN_POINT('Ctrl Pts',(-5.786479155966,2.34344956093245,44.450705515607));
#48369=CARTESIAN_POINT('Ctrl Pts',(-5.91400340733182,0.385111721800315,
44.5435134668228));
#48370=CARTESIAN_POINT('Ctrl Pts',(-5.92229880001647,0.257722764713088,
44.5495505804803));
#48371=CARTESIAN_POINT('Ctrl Pts',(-5.92606908611989,0.130039138944288,
44.5555876941379));
#48372=CARTESIAN_POINT('Ctrl Pts',(-5.92543336817915,0.00231728688185692,
44.5616248077955));
#48373=CARTESIAN_POINT('Origin',(0.,0.,-10.));
#48374=CARTESIAN_POINT('',(-5.91475019377533,0.00539823251707206,46.5633751922049));
#48375=CARTESIAN_POINT('',(-5.91039421288723,0.00428526322922202,46.3116248077954));
#48376=CARTESIAN_POINT('',(-5.91675,-7.2459289488551E-16,-10.));
#48377=CARTESIAN_POINT('Ctrl Pts',(-5.91475019377533,0.00539823251707206,
46.5633751922049));
#48378=CARTESIAN_POINT('Ctrl Pts',(-5.91941312805242,0.530811138238026,
46.538655888443));
#48379=CARTESIAN_POINT('Ctrl Pts',(-5.85522209608251,1.055103733712,46.5139365846812));
#48380=CARTESIAN_POINT('Ctrl Pts',(-5.71768655742746,1.55939297514728,46.4892172809193));
#48381=CARTESIAN_POINT('Ctrl Pts',(-5.20141435370859,3.45236202542662,46.3964275223426));
#48382=CARTESIAN_POINT('Ctrl Pts',(-3.65167848361261,5.06347302608539,46.3036377637658));
#48383=CARTESIAN_POINT('Ctrl Pts',(-1.78017798854655,5.65284108648206,46.210848005189));
#48384=CARTESIAN_POINT('Ctrl Pts',(0.0913225065194465,6.24220914687871,
46.1180582466122));
#48385=CARTESIAN_POINT('Ctrl Pts',(2.28458762655536,5.80983426701343,46.0252684880356));
#48386=CARTESIAN_POINT('Ctrl Pts',(3.79238464655248,4.55427982369533,45.9324787294588));
#48387=CARTESIAN_POINT('Ctrl Pts',(5.3001816665496,3.29872538037722,45.839688970882));
#48388=CARTESIAN_POINT('Ctrl Pts',(6.12251058650776,1.21999137360628,45.7468992123053));
#48389=CARTESIAN_POINT('Ctrl Pts',(5.88172595383818,-0.727286617415579,
45.6541094537285));
#48390=CARTESIAN_POINT('Ctrl Pts',(5.64094132116859,-2.67456460843749,45.5613196951517));
#48391=CARTESIAN_POINT('Ctrl Pts',(4.33704313587116,-4.4903865837104,45.468529936575));
#48392=CARTESIAN_POINT('Ctrl Pts',(2.56883220424791,-5.34085640383115,45.3757401779983));
#48393=CARTESIAN_POINT('Ctrl Pts',(0.800621272624648,-6.19132622395189,
45.2829504194215));
#48394=CARTESIAN_POINT('Ctrl Pts',(-1.4319024053245,-6.07644388892052,45.1901606608447));
#48395=CARTESIAN_POINT('Ctrl Pts',(-3.10347704649546,-5.04896783925202,
45.0973709022679));
#48396=CARTESIAN_POINT('Ctrl Pts',(-4.77505168766637,-4.02149178958355,
45.0045811436912));
#48397=CARTESIAN_POINT('Ctrl Pts',(-5.88567729205918,-2.08142202527798,
44.9117913851144));
#48398=CARTESIAN_POINT('Ctrl Pts',(-5.92531134645547,-0.119714107319727,
44.8190016265377));
#48399=CARTESIAN_POINT('Ctrl Pts',(-5.92611243487954,-0.0800638235317725,
44.8171261484268));
#48400=CARTESIAN_POINT('Ctrl Pts',(-5.92647599117001,-0.0404046999098048,
44.8152506703158));
#48401=CARTESIAN_POINT('Ctrl Pts',(-5.92640592629062,-0.000744257410045246,
44.8133751922049));
#48402=CARTESIAN_POINT('Ctrl Pts',(-5.92543336817915,0.00231728688185692,
44.5616248077955));
#48403=CARTESIAN_POINT('Ctrl Pts',(-5.91629625708645,-1.83341626171998,
44.6483956453536));
#48404=CARTESIAN_POINT('Ctrl Pts',(-4.9969655697077,-3.67704660900026,44.7351664829118));
#48405=CARTESIAN_POINT('Ctrl Pts',(-3.52107555964431,-4.76715578133082,
44.8219373204699));
#48406=CARTESIAN_POINT('Ctrl Pts',(-1.94249994704928,-5.93310970931579,
44.9147452716856));
#48407=CARTESIAN_POINT('Ctrl Pts',(0.272774791682385,-6.23704182927182,
45.0075532229013));
#48408=CARTESIAN_POINT('Ctrl Pts',(2.107043083091,-5.53932457852026,45.100361174117));
#48409=CARTESIAN_POINT('Ctrl Pts',(3.94131137449957,-4.84160732776873,45.1931691253327));
#48410=CARTESIAN_POINT('Ctrl Pts',(5.394573218585,-3.1422407063096,45.2859770765484));
#48411=CARTESIAN_POINT('Ctrl Pts',(5.79919464085023,-1.22192015194707,45.3787850277641));
#48412=CARTESIAN_POINT('Ctrl Pts',(6.20381606311547,0.69840040241552,45.4715929789798));
#48413=CARTESIAN_POINT('Ctrl Pts',(5.55979706356047,2.83967488968159,45.5644009301955));
#48414=CARTESIAN_POINT('Ctrl Pts',(4.16300240053861,4.21819373112593,45.6572088814113));
#48415=CARTESIAN_POINT('Ctrl Pts',(2.7662077375168,5.59671257257024,45.750016832627));
#48416=CARTESIAN_POINT('Ctrl Pts',(0.616637411028301,6.21247576819288,45.8428247838427));
#48417=CARTESIAN_POINT('Ctrl Pts',(-1.29818786036205,5.78259938257951,45.9356327350584));
#48418=CARTESIAN_POINT('Ctrl Pts',(-3.21301313175245,5.35272299696613,46.0284406862741));
#48419=CARTESIAN_POINT('Ctrl Pts',(-4.89309334804463,3.87720703011655,46.1212486374898));
#48420=CARTESIAN_POINT('Ctrl Pts',(-5.56659331873784,2.0339090844931,46.2140565887055));
#48421=CARTESIAN_POINT('Ctrl Pts',(-5.80260827161228,1.38796120520504,46.2465793284022));
#48422=CARTESIAN_POINT('Ctrl Pts',(-5.91501360248399,0.696849126068583,
46.2791020680988));
#48423=CARTESIAN_POINT('Ctrl Pts',(-5.91039421288723,0.00428526322922202,
46.3116248077954));
#48424=CARTESIAN_POINT('Origin',(0.,0.,-10.));
#48425=CARTESIAN_POINT('',(-5.90740046258813,-0.00170769527667092,48.3133751922049));
#48426=CARTESIAN_POINT('',(-5.90981348303521,-0.00398707326546309,48.0616248077955));
#48427=CARTESIAN_POINT('',(-5.91675,-7.2459289488551E-16,-10.));
#48428=CARTESIAN_POINT('Ctrl Pts',(-5.90740046258813,-0.00170769527667092,
48.3133751922049));
#48429=CARTESIAN_POINT('Ctrl Pts',(-5.90458171200211,1.09240074162204,48.2620611065702));
#48430=CARTESIAN_POINT('Ctrl Pts',(-5.61374355902189,2.18790212669476,48.2107470209356));
#48431=CARTESIAN_POINT('Ctrl Pts',(-5.04408146542834,3.11141257149349,48.1594329353009));
#48432=CARTESIAN_POINT('Ctrl Pts',(-4.01397818128872,4.78136946843801,48.0666431767242));
#48433=CARTESIAN_POINT('Ctrl Pts',(-2.072164387591,5.88894299381245,47.9738534181474));
#48434=CARTESIAN_POINT('Ctrl Pts',(-0.110396571509901,5.92549226789844,
47.8810636595706));
#48435=CARTESIAN_POINT('Ctrl Pts',(1.85137124457137,5.96204154198443,47.7882739009939));
#48436=CARTESIAN_POINT('Ctrl Pts',(3.83309308303601,4.92756656478179,47.6954841424172));
#48437=CARTESIAN_POINT('Ctrl Pts',(4.92468512896701,3.29713851702603,47.6026943838404));
#48438=CARTESIAN_POINT('Ctrl Pts',(6.0162771748979,1.66671046927041,47.5099046252636));
#48439=CARTESIAN_POINT('Ctrl Pts',(6.21773942829533,-0.559670649038214,
47.4171148666868));
#48440=CARTESIAN_POINT('Ctrl Pts',(5.43655257965025,-2.35956395730728,47.3243251081101));
#48441=CARTESIAN_POINT('Ctrl Pts',(4.65536573100512,-4.15945726557646,47.2315353495333));
#48442=CARTESIAN_POINT('Ctrl Pts',(2.89152978031738,-5.53286276380603,47.1387455909566));
#48443=CARTESIAN_POINT('Ctrl Pts',(0.955066860730234,-5.84905918173686,
47.0459558323798));
#48444=CARTESIAN_POINT('Ctrl Pts',(-0.981396058856855,-6.16525559966767,
46.9531660738031));
#48445=CARTESIAN_POINT('Ctrl Pts',(-3.09048594734334,-5.4242429372998,46.8603763152263));
#48446=CARTESIAN_POINT('Ctrl Pts',(-4.4036266229157,-3.96632305616593,46.7675865566495));
#48447=CARTESIAN_POINT('Ctrl Pts',(-5.36694503642602,-2.89679479232864,
46.6995161018346));
#48448=CARTESIAN_POINT('Ctrl Pts',(-5.90190970036696,-1.44145058663312,
46.6314456470198));
#48449=CARTESIAN_POINT('Ctrl Pts',(-5.91475019377533,0.00539823251707206,
46.5633751922049));
#48450=CARTESIAN_POINT('Ctrl Pts',(-5.91039421288723,0.00428526322922202,
46.3116248077954));
#48451=CARTESIAN_POINT('Ctrl Pts',(-5.90183156159993,-1.27947371129696,
46.3719100193145));
#48452=CARTESIAN_POINT('Ctrl Pts',(-5.49117736245765,-2.5682209477384,46.4321952308336));
#48453=CARTESIAN_POINT('Ctrl Pts',(-4.72037082906262,-3.58355222877175,
46.4924804423527));
#48454=CARTESIAN_POINT('Ctrl Pts',(-3.53372864359993,-5.14663567201572,
46.5852883935684));
#48455=CARTESIAN_POINT('Ctrl Pts',(-1.49352454758038,-6.06172263410644,
46.6780963447841));
#48456=CARTESIAN_POINT('Ctrl Pts',(0.462963999359967,-5.90841871193105,
46.7709042959998));
#48457=CARTESIAN_POINT('Ctrl Pts',(2.41945254630037,-5.75511478975566,46.8637122472155));
#48458=CARTESIAN_POINT('Ctrl Pts',(4.29222554416156,-4.53341998331399,46.9565201984312));
#48459=CARTESIAN_POINT('Ctrl Pts',(5.2209240115379,-2.80458549628057,47.0493281496469));
#48460=CARTESIAN_POINT('Ctrl Pts',(6.14962247891425,-1.07575100924715,47.1421361008626));
#48461=CARTESIAN_POINT('Ctrl Pts',(6.13424641580585,1.16022315837803,47.2349440520783));
#48462=CARTESIAN_POINT('Ctrl Pts',(5.18185964362037,2.87612203740016,47.327752003294));
#48463=CARTESIAN_POINT('Ctrl Pts',(4.2294728714349,4.5920209164223,47.4205599545097));
#48464=CARTESIAN_POINT('Ctrl Pts',(2.34007539017238,5.78784450684132,47.5133679057255));
#48465=CARTESIAN_POINT('Ctrl Pts',(0.381663531638894,5.91422693923875,47.6061758569412));
#48466=CARTESIAN_POINT('Ctrl Pts',(-1.57674832689459,6.04060937163617,47.6989838081569));
#48467=CARTESIAN_POINT('Ctrl Pts',(-3.60417456269912,5.09755064601189,47.7917917593726));
#48468=CARTESIAN_POINT('Ctrl Pts',(-4.76920791333336,3.5182954991869,47.8845997105883));
#48469=CARTESIAN_POINT('Ctrl Pts',(-5.50994955397949,2.51418686330868,47.943608076324));
#48470=CARTESIAN_POINT('Ctrl Pts',(-5.90206343299662,1.25289181263786,48.0026164420597));
#48471=CARTESIAN_POINT('Ctrl Pts',(-5.90981348303521,-0.00398707326546309,
48.0616248077955));
#48472=CARTESIAN_POINT('Origin',(0.,0.,-10.));
#48473=CARTESIAN_POINT('',(-5.92103312412998,-0.00476770783831071,50.0633751922048));
#48474=CARTESIAN_POINT('',(-5.92496225112949,-0.0027597696008211,49.8116248077954));
#48475=CARTESIAN_POINT('',(-5.91675,-7.2459289488551E-16,-10.));
#48476=CARTESIAN_POINT('Ctrl Pts',(-5.92103312412998,-0.00476770783831071,
50.0633751922048));
#48477=CARTESIAN_POINT('Ctrl Pts',(-5.90655967293925,1.64669327195933,49.9854663246974));
#48478=CARTESIAN_POINT('Ctrl Pts',(-5.18523595369446,3.30923484336091,49.90755745719));
#48479=CARTESIAN_POINT('Ctrl Pts',(-3.95939357169421,4.40985811158953,49.8296485896825));
#48480=CARTESIAN_POINT('Ctrl Pts',(-2.49941061573483,5.72070462508994,49.7368588311058));
#48481=CARTESIAN_POINT('Ctrl Pts',(-0.32377293541545,6.23447559301229,49.644069072529));
#48482=CARTESIAN_POINT('Ctrl Pts',(1.56838195079361,5.71522738623322,49.5512793139523));
#48483=CARTESIAN_POINT('Ctrl Pts',(3.46053683700266,5.19597917945415,49.4584895553755));
#48484=CARTESIAN_POINT('Ctrl Pts',(5.06920892910144,3.64371179797354,49.3656997967988));
#48485=CARTESIAN_POINT('Ctrl Pts',(5.65563337820364,1.7712868517759,49.272910038222));
#48486=CARTESIAN_POINT('Ctrl Pts',(6.24205782730584,-0.10113809442173,49.1801202796453));
#48487=CARTESIAN_POINT('Ctrl Pts',(5.8062346334116,-2.29372060533647,49.0873305210685));
#48488=CARTESIAN_POINT('Ctrl Pts',(4.54831077337202,-3.79954143664119,48.9945407624917));
#48489=CARTESIAN_POINT('Ctrl Pts',(3.29038691333237,-5.30536226794598,48.901751003915));
#48490=CARTESIAN_POINT('Ctrl Pts',(1.21036238714734,-6.12442141964063,48.8089612453382));
#48491=CARTESIAN_POINT('Ctrl Pts',(-0.736534569227438,-5.88057504401213,
48.7161714867614));
#48492=CARTESIAN_POINT('Ctrl Pts',(-2.68343152560205,-5.63672866838366,
48.6233817281847));
#48493=CARTESIAN_POINT('Ctrl Pts',(-4.49720091216637,-4.32997676543226,
48.5305919696079));
#48494=CARTESIAN_POINT('Ctrl Pts',(-5.34488921815788,-2.56043067969923,
48.4378022110312));
#48495=CARTESIAN_POINT('Ctrl Pts',(-5.72379356574355,-1.76946930816867,
48.3963265380891));
#48496=CARTESIAN_POINT('Ctrl Pts',(-5.90967877615379,-0.886043509327994,
48.354850865147));
#48497=CARTESIAN_POINT('Ctrl Pts',(-5.90740046258813,-0.00170769527667092,
48.3133751922049));
#48498=CARTESIAN_POINT('Ctrl Pts',(-5.90981348303521,-0.00398707326546309,
48.0616248077955));
#48499=CARTESIAN_POINT('Ctrl Pts',(-5.91425265831972,-0.723918642500199,
48.0954243932754));
#48500=CARTESIAN_POINT('Ctrl Pts',(-5.79258515549998,-1.44240130362546,
48.1292239787554));
#48501=CARTESIAN_POINT('Ctrl Pts',(-5.53809513799413,-2.11027239538551,
48.1630235642354));
#48502=CARTESIAN_POINT('Ctrl Pts',(-4.83930854655658,-3.94413357510722,
48.2558315154511));
#48503=CARTESIAN_POINT('Ctrl Pts',(-3.13909489821737,-5.39640436652492,
48.3486394666669));
#48504=CARTESIAN_POINT('Ctrl Pts',(-1.21853875812531,-5.7999060884765,48.4414474178826));
#48505=CARTESIAN_POINT('Ctrl Pts',(0.702017381966812,-6.20340781042809,
48.5342553690983));
#48506=CARTESIAN_POINT('Ctrl Pts',(2.8429160138118,-5.5581404629135,48.627063320314));
#48507=CARTESIAN_POINT('Ctrl Pts',(4.2206202280831,-4.16054230004888,48.7198712715297));
#48508=CARTESIAN_POINT('Ctrl Pts',(5.59832444235433,-2.76294413718435,48.8126792227454));
#48509=CARTESIAN_POINT('Ctrl Pts',(6.21283423905197,-0.613015158969908,
48.9054871739611));
#48510=CARTESIAN_POINT('Ctrl Pts',(5.78184149895695,1.30155915007333,48.9982951251768));
#48511=CARTESIAN_POINT('Ctrl Pts',(5.35084875886191,3.21613345911667,49.0911030763925));
#48512=CARTESIAN_POINT('Ctrl Pts',(3.87435348197408,4.89535309898879,49.1839110276082));
#48513=CARTESIAN_POINT('Ctrl Pts',(2.03066316948238,5.56777823124342,49.2767189788239));
#48514=CARTESIAN_POINT('Ctrl Pts',(0.186972856990724,6.24020336349805,49.3695269300396));
#48515=CARTESIAN_POINT('Ctrl Pts',(-2.02391249110479,5.90583398813525,49.4623348812554));
#48516=CARTESIAN_POINT('Ctrl Pts',(-3.58630380396423,4.71828065781085,49.5551428324711));
#48517=CARTESIAN_POINT('Ctrl Pts',(-5.02556701687734,3.62431539594555,49.6406368242459));
#48518=CARTESIAN_POINT('Ctrl Pts',(-5.91452098969204,1.80634191132433,49.7261308160207));
#48519=CARTESIAN_POINT('Ctrl Pts',(-5.92496225112949,-0.0027597696008211,
49.8116248077954));
#48520=CARTESIAN_POINT('Origin',(0.,0.,-10.));
#48521=CARTESIAN_POINT('',(-5.92286503569152,0.00406918162620035,51.8133751922048));
#48522=CARTESIAN_POINT('',(-5.91832046510867,0.00534203625220547,51.5616248077954));
#48523=CARTESIAN_POINT('',(-5.91675,-7.2459289488551E-16,-10.));
#48524=CARTESIAN_POINT('Ctrl Pts',(-5.92286503569152,0.00406918162620035,
51.8133751922048));
#48525=CARTESIAN_POINT('Ctrl Pts',(-5.92481339761004,0.25217262273859,51.8016613014014));
#48526=CARTESIAN_POINT('Ctrl Pts',(-5.9105794954103,0.500050794796438,51.7899474105979));
#48527=CARTESIAN_POINT('Ctrl Pts',(-5.8794095934613,0.745780699831111,51.7782335197944));
#48528=CARTESIAN_POINT('Ctrl Pts',(-5.63250207782596,2.69229180752391,51.6854437612177));
#48529=CARTESIAN_POINT('Ctrl Pts',(-4.32289968838734,4.50400412052595,51.5926540026409));
#48530=CARTESIAN_POINT('Ctrl Pts',(-2.55202282404879,5.34890881633436,51.4998642440641));
#48531=CARTESIAN_POINT('Ctrl Pts',(-0.781145959710435,6.19381351214267,
51.4070744854874));
#48532=CARTESIAN_POINT('Ctrl Pts',(1.45100537952779,6.07191059075762,51.3142847269106));
#48533=CARTESIAN_POINT('Ctrl Pts',(3.11934040299276,5.03918261925308,51.2214949683339));
#48534=CARTESIAN_POINT('Ctrl Pts',(4.78767542645788,4.00645464774845,51.1287052097571));
#48535=CARTESIAN_POINT('Ctrl Pts',(5.89219413414971,2.06290162612413,51.0359154511803));
#48536=CARTESIAN_POINT('Ctrl Pts',(5.92565853755101,0.101078762725555,50.9431256926036));
#48537=CARTESIAN_POINT('Ctrl Pts',(5.95912294095232,-1.86074410067291,50.8503359340268));
#48538=CARTESIAN_POINT('Ctrl Pts',(4.92153304006336,-3.84083680584558,50.7575461754501));
#48539=CARTESIAN_POINT('Ctrl Pts',(3.2893905098375,-4.9298636993041,50.6647564168733));
#48540=CARTESIAN_POINT('Ctrl Pts',(1.6572479796116,-6.01889059276266,50.5719666582966));
#48541=CARTESIAN_POINT('Ctrl Pts',(-0.569447179951226,-6.21685167450689,
50.4791768997198));
#48542=CARTESIAN_POINT('Ctrl Pts',(-2.368109868289,-5.43283550934846,50.3863871411431));
#48543=CARTESIAN_POINT('Ctrl Pts',(-4.16677255662673,-4.64881934419006,
50.2935973825663));
#48544=CARTESIAN_POINT('Ctrl Pts',(-5.53740277373949,-2.88282593212903,
50.2008076239896));
#48545=CARTESIAN_POINT('Ctrl Pts',(-5.85055376649621,-0.945868196559284,
50.1080178654128));
#48546=CARTESIAN_POINT('Ctrl Pts',(-5.90077445769035,-0.635234162038707,
50.0931369743435));
#48547=CARTESIAN_POINT('Ctrl Pts',(-5.92379760855206,-0.320203058547937,
50.0782560832742));
#48548=CARTESIAN_POINT('Ctrl Pts',(-5.92103312412998,-0.00476770783831071,
50.0633751922048));
#48549=CARTESIAN_POINT('Ctrl Pts',(-5.92496225112949,-0.0027597696008211,
49.8116248077954));
#48550=CARTESIAN_POINT('Ctrl Pts',(-5.92585549474907,-0.157527327462026,
49.8189387672364));
#48551=CARTESIAN_POINT('Ctrl Pts',(-5.92031916798354,-0.312229955259537,
49.8262527266773));
#48552=CARTESIAN_POINT('Ctrl Pts',(-5.90814777925456,-0.466408789250156,
49.8335666861182));
#48553=CARTESIAN_POINT('Ctrl Pts',(-5.75370316406207,-2.42280762070086,
49.9263746373339));
#48554=CARTESIAN_POINT('Ctrl Pts',(-4.53091665605359,-4.29486799831616,
50.0191825885497));
#48555=CARTESIAN_POINT('Ctrl Pts',(-2.8015409907225,-5.22255832112021,50.1119905397654));
#48556=CARTESIAN_POINT('Ctrl Pts',(-1.07216532539152,-6.15024864392421,
50.2047984909811));
#48557=CARTESIAN_POINT('Ctrl Pts',(1.16379949726205,-6.13356891191712,50.2976064421968));
#48558=CARTESIAN_POINT('Ctrl Pts',(2.87914280115849,-5.18018185691753,50.3904143934125));
#48559=CARTESIAN_POINT('Ctrl Pts',(4.59448610505489,-4.22679480191797,50.4832223446282));
#48560=CARTESIAN_POINT('Ctrl Pts',(5.78920789019427,-2.33670042392594,50.5760302958439));
#48561=CARTESIAN_POINT('Ctrl Pts',(5.9144484606608,-0.378215211734605,50.6688382470596));
#48562=CARTESIAN_POINT('Ctrl Pts',(6.03968903112733,1.58027000045679,50.7616461982753));
#48563=CARTESIAN_POINT('Ctrl Pts',(5.09544838692106,3.60714604684744,50.854454149491));
#48564=CARTESIAN_POINT('Ctrl Pts',(3.51551424271886,4.7712584240891,50.9472621007067));
#48565=CARTESIAN_POINT('Ctrl Pts',(1.93558009851661,5.9353708013308,51.0400700519224));
#48566=CARTESIAN_POINT('Ctrl Pts',(-0.280047545681603,6.23671950942332,
51.1328780031381));
#48567=CARTESIAN_POINT('Ctrl Pts',(-2.11350099031294,5.5368638148456,51.2256859543539));
#48568=CARTESIAN_POINT('Ctrl Pts',(-3.94695443494423,4.8370081202679,51.3184939055696));
#48569=CARTESIAN_POINT('Ctrl Pts',(-5.39823368000872,3.13594802301999,51.4113018567853));
#48570=CARTESIAN_POINT('Ctrl Pts',(-5.80061556448015,1.21515695007312,51.504109808001));
#48571=CARTESIAN_POINT('Ctrl Pts',(-5.88373701294625,0.818372347322348,
51.5232814745991));
#48572=CARTESIAN_POINT('Ctrl Pts',(-5.92209925711613,0.412211246926501,
51.5424531411973));
#48573=CARTESIAN_POINT('Ctrl Pts',(-5.91832046510867,0.00534203625220547,
51.5616248077954));
#48574=CARTESIAN_POINT('Origin',(0.,0.,-10.));
#48575=CARTESIAN_POINT('',(-5.90815917370761,0.00272910693063455,53.5633751922048));
#48576=CARTESIAN_POINT('',(-5.90694896850773,0.00026360489279184,53.3116248077954));
#48577=CARTESIAN_POINT('',(-5.91675,-7.2459289488551E-16,-10.));
#48578=CARTESIAN_POINT('Ctrl Pts',(-5.90815917370761,0.00272910693063455,
53.5633751922048));
#48579=CARTESIAN_POINT('Ctrl Pts',(-5.91154687758133,0.819276877355236,
53.5250665195286));
#48580=CARTESIAN_POINT('Ctrl Pts',(-5.75395693091378,1.63457377819285,53.4867578468523));
#48581=CARTESIAN_POINT('Ctrl Pts',(-5.42910500543416,2.37664992371513,53.448449174176));
#48582=CARTESIAN_POINT('Ctrl Pts',(-4.64226146237614,4.17407754462117,53.3556594155992));
#48583=CARTESIAN_POINT('Ctrl Pts',(-2.87411495566173,5.54192909150009,53.2628696570225));
#48584=CARTESIAN_POINT('Ctrl Pts',(-0.936667193567707,5.85203388476343,
53.1700798984458));
#48585=CARTESIAN_POINT('Ctrl Pts',(1.00078056852626,6.16213867802676,53.077290139869));
#48586=CARTESIAN_POINT('Ctrl Pts',(3.10752958599982,5.41449671767459,52.9845003812922));
#48587=CARTESIAN_POINT('Ctrl Pts',(4.41607869613672,3.95245429694674,52.8917106227155));
#48588=CARTESIAN_POINT('Ctrl Pts',(5.72462780627373,2.49041187621876,52.7989208641387));
#48589=CARTESIAN_POINT('Ctrl Pts',(6.23497700907392,0.31396899511498,52.706131105562));
#48590=CARTESIAN_POINT('Ctrl Pts',(5.71275408316433,-1.57736704834818,52.6133413469852));
#48591=CARTESIAN_POINT('Ctrl Pts',(5.19053115725477,-3.46870309181124,52.5205515884085));
#48592=CARTESIAN_POINT('Ctrl Pts',(3.63573610263556,-5.07493229763371,52.4277618298317));
#48593=CARTESIAN_POINT('Ctrl Pts',(1.76239133519637,-5.65841168540697,52.334972071255));
#48594=CARTESIAN_POINT('Ctrl Pts',(-0.110953432242873,-6.24189107318024,
52.2421823126782));
#48595=CARTESIAN_POINT('Ctrl Pts',(-2.30284791250211,-5.80262064290423,
52.1493925541014));
#48596=CARTESIAN_POINT('Ctrl Pts',(-3.80668883171557,-4.54233047657448,
52.0566027955247));
#48597=CARTESIAN_POINT('Ctrl Pts',(-5.1206830632809,-3.44114085771377,51.9755269277514));
#48598=CARTESIAN_POINT('Ctrl Pts',(-5.90937975262626,-1.71314008071065,
51.8944510599781));
#48599=CARTESIAN_POINT('Ctrl Pts',(-5.92286503569152,0.00406918162620035,
51.8133751922048));
#48600=CARTESIAN_POINT('Ctrl Pts',(-5.91832046510867,0.00534203625220547,
51.5616248077954));
#48601=CARTESIAN_POINT('Ctrl Pts',(-5.90380653631969,-1.55739831529493,
51.635261092413));
#48602=CARTESIAN_POINT('Ctrl Pts',(-5.26760929556394,-3.1305850246698,51.7088973770305));
#48603=CARTESIAN_POINT('Ctrl Pts',(-4.15808078522284,-4.22304529028058,
51.7825336616481));
#48604=CARTESIAN_POINT('Ctrl Pts',(-2.75967959761573,-5.59993440904152,
51.8753416128638));
#48605=CARTESIAN_POINT('Ctrl Pts',(-0.609392698522968,-6.2131905979175,
51.9681495640795));
#48606=CARTESIAN_POINT('Ctrl Pts',(1.30492999733203,-5.78108164985268,52.0609575152952));
#48607=CARTESIAN_POINT('Ctrl Pts',(3.21925269318707,-5.34897270178784,52.153765466511));
#48608=CARTESIAN_POINT('Ctrl Pts',(4.8976111858045,-3.8714986167822,52.2465734177267));
#48609=CARTESIAN_POINT('Ctrl Pts',(5.56896125103606,-2.02741656416713,52.3393813689424));
#48610=CARTESIAN_POINT('Ctrl Pts',(6.24031131626763,-0.183334511552064,
52.4321893201581));
#48611=CARTESIAN_POINT('Ctrl Pts',(5.90465295411334,2.02735550867244,52.5249972713738));
#48612=CARTESIAN_POINT('Ctrl Pts',(4.71618888262451,3.58905416002731,52.6178052225895));
#48613=CARTESIAN_POINT('Ctrl Pts',(3.52772481113574,5.1507528113821,52.7106131738052));
#48614=CARTESIAN_POINT('Ctrl Pts',(1.48645503031256,6.06346009386735,52.803421125021));
#48615=CARTESIAN_POINT('Ctrl Pts',(-0.469853420589139,5.90787483815975,
52.8962290762367));
#48616=CARTESIAN_POINT('Ctrl Pts',(-2.42616187149089,5.75228958245214,52.9890370274524));
#48617=CARTESIAN_POINT('Ctrl Pts',(-4.29750899247115,4.52841178855161,53.081844978668));
#48618=CARTESIAN_POINT('Ctrl Pts',(-5.22419085534354,2.79849553280782,53.1746529298837));
#48619=CARTESIAN_POINT('Ctrl Pts',(-5.68007620180948,1.94745538278016,53.2203102225209));
#48620=CARTESIAN_POINT('Ctrl Pts',(-5.90733435577458,0.973944175586275,
53.2659675151582));
#48621=CARTESIAN_POINT('Ctrl Pts',(-5.90694896850773,0.00026360489279184,
53.3116248077954));
#48622=CARTESIAN_POINT('Origin',(0.,0.,-10.));
#48623=CARTESIAN_POINT('',(-5.91284273101683,-0.00510202345033239,55.3133751922048));
#48624=CARTESIAN_POINT('',(-5.9173496880968,-0.00543369097055152,55.0616248077955));
#48625=CARTESIAN_POINT('',(-5.91675,-7.2459289488551E-16,-10.));
#48626=CARTESIAN_POINT('Ctrl Pts',(-5.91284273101683,-0.00510202345033239,
55.3133751922048));
#48627=CARTESIAN_POINT('Ctrl Pts',(-5.90155143772713,1.37555990727446,55.2484717376557));
#48628=CARTESIAN_POINT('Ctrl Pts',(-5.41952439852393,2.76332589927981,55.1835682831067));
#48629=CARTESIAN_POINT('Ctrl Pts',(-4.53633894809001,3.81382681410247,55.1186648285576));
#48630=CARTESIAN_POINT('Ctrl Pts',(-3.27368559175257,5.3156841027214,55.0258750699808));
#48631=CARTESIAN_POINT('Ctrl Pts',(-1.1910954595644,6.12819765018871,54.9330853114041));
#48632=CARTESIAN_POINT('Ctrl Pts',(0.755024986365453,5.87822960506726,54.8402955528274));
#48633=CARTESIAN_POINT('Ctrl Pts',(2.70114543229536,5.6282615599458,54.7475057942506));
#48634=CARTESIAN_POINT('Ctrl Pts',(4.51079619196693,4.31581192223552,54.6547160356738));
#48635=CARTESIAN_POINT('Ctrl Pts',(5.35291518842123,2.54360865808689,54.5619262770971));
#48636=CARTESIAN_POINT('Ctrl Pts',(6.19503418487551,0.771405393938316,54.4691365185203));
#48637=CARTESIAN_POINT('Ctrl Pts',(6.06962141811261,-1.46055149664842,54.3763467599436));
#48638=CARTESIAN_POINT('Ctrl Pts',(5.03427131283913,-3.12726052139094,54.2835570013668));
#48639=CARTESIAN_POINT('Ctrl Pts',(3.99892120756563,-4.79396954613351,54.1907672427901));
#48640=CARTESIAN_POINT('Ctrl Pts',(2.05363376378125,-5.89543070503176,54.0979774842133));
#48641=CARTESIAN_POINT('Ctrl Pts',(0.0917607040070565,-5.92581015500205,
54.0051877256365));
#48642=CARTESIAN_POINT('Ctrl Pts',(-1.87011235576708,-5.95618960497235,
53.9123979670598));
#48643=CARTESIAN_POINT('Ctrl Pts',(-3.84857103153118,-4.91548734601488,
53.8196082084831));
#48644=CARTESIAN_POINT('Ctrl Pts',(-4.93503007971246,-3.28163436906956,
53.7268184499063));
#48645=CARTESIAN_POINT('Ctrl Pts',(-5.57293958221817,-2.32232500399466,
53.6723373640058));
#48646=CARTESIAN_POINT('Ctrl Pts',(-5.90334131464709,-1.15853298111622,
53.6178562781053));
#48647=CARTESIAN_POINT('Ctrl Pts',(-5.90815917370761,0.00272910693063455,
53.5633751922048));
#48648=CARTESIAN_POINT('Ctrl Pts',(-5.90694896850773,0.00026360489279184,
53.3116248077954));
#48649=CARTESIAN_POINT('Ctrl Pts',(-5.90655097593327,-1.00526426374504,
53.3587754663739));
#48650=CARTESIAN_POINT('Ctrl Pts',(-5.66337430186719,-2.01097275620775,
53.4059261249524));
#48651=CARTESIAN_POINT('Ctrl Pts',(-5.17850230926167,-2.88216258617933,
53.4530767835309));
#48652=CARTESIAN_POINT('Ctrl Pts',(-4.22411529554287,-4.59694973183572,
53.5458847347466));
#48653=CARTESIAN_POINT('Ctrl Pts',(-2.33332466334076,-5.79056930556137,
53.6386926859623));
#48654=CARTESIAN_POINT('Ctrl Pts',(-0.374766763259672,-5.91466797152268,
53.731500637178));
#48655=CARTESIAN_POINT('Ctrl Pts',(1.58379113682131,-6.03876663748399,53.8243085883937));
#48656=CARTESIAN_POINT('Ctrl Pts',(3.61011630478126,-5.09334439568107,53.9171165396094));
#48657=CARTESIAN_POINT('Ctrl Pts',(4.77330731290138,-3.51273179118511,54.0099244908252));
#48658=CARTESIAN_POINT('Ctrl Pts',(5.93649832102157,-1.93211918668906,54.1027324420409));
#48659=CARTESIAN_POINT('Ctrl Pts',(6.2365551693018,0.28368378050013,54.1955403932565));
#48660=CARTESIAN_POINT('Ctrl Pts',(5.53563060949312,2.11672886677609,54.2883483444723));
#48661=CARTESIAN_POINT('Ctrl Pts',(4.83470604968444,3.94977395305205,54.381156295688));
#48662=CARTESIAN_POINT('Ctrl Pts',(3.13280008178686,5.40006115841479,54.4739642469037));
#48663=CARTESIAN_POINT('Ctrl Pts',(1.21177472893962,5.8013230686201,54.5667721981195));
#48664=CARTESIAN_POINT('Ctrl Pts',(-0.709250623907553,6.20258497882539,
54.6595801493352));
#48665=CARTESIAN_POINT('Ctrl Pts',(-2.84939536170436,5.55482159387331,54.7523881005508));
#48666=CARTESIAN_POINT('Ctrl Pts',(-4.22546891689455,4.15561785689665,54.8451960517666));
#48667=CARTESIAN_POINT('Ctrl Pts',(-5.2951397940584,3.06796706743294,54.9173389704428));
#48668=CARTESIAN_POINT('Ctrl Pts',(-5.90312024773647,1.52625804066341,54.9894818891192));
#48669=CARTESIAN_POINT('Ctrl Pts',(-5.9173496880968,-0.00543369097055152,
55.0616248077955));
#48670=CARTESIAN_POINT('Origin',(0.,0.,-10.));
#48671=CARTESIAN_POINT('',(-5.92646560327161,-0.000513552043279186,57.0633751922049));
#48672=CARTESIAN_POINT('',(-5.92550609890763,0.00223999432222687,56.8116248077954));
#48673=CARTESIAN_POINT('',(-5.91675,-7.2459289488551E-16,-10.));
#48674=CARTESIAN_POINT('Ctrl Pts',(-5.92646560327161,-0.000513552043279186,
57.0633751922049));
#48675=CARTESIAN_POINT('Ctrl Pts',(-5.92406967673236,1.93433291671647,56.971876955783));
#48676=CARTESIAN_POINT('Ctrl Pts',(-4.88666447252146,3.87138216918967,56.8803787193611));
#48677=CARTESIAN_POINT('Ctrl Pts',(-3.27387011390087,4.94018425741713,56.7888804829392));
#48678=CARTESIAN_POINT('Ctrl Pts',(-1.63831073021625,6.02407277386586,56.6960907243624));
#48679=CARTESIAN_POINT('Ctrl Pts',(0.588995993440916,6.2150300524844,56.6033009657857));
#48680=CARTESIAN_POINT('Ctrl Pts',(2.38518410246891,5.42536107713163,56.510511207209));
#48681=CARTESIAN_POINT('Ctrl Pts',(4.18137221149686,4.63569210177889,56.4177214486322));
#48682=CARTESIAN_POINT('Ctrl Pts',(5.54644170589567,2.86539687245493,56.3249316900555));
#48683=CARTESIAN_POINT('Ctrl Pts',(5.85349953287863,0.927463874506721,56.2321419314787));
#48684=CARTESIAN_POINT('Ctrl Pts',(6.16055735986159,-1.01046912344149,56.139352172902));
#48685=CARTESIAN_POINT('Ctrl Pts',(5.40960351942869,-3.11603989001394,56.0465624143252));
#48686=CARTESIAN_POINT('Ctrl Pts',(3.94550524908144,-4.42228836117639,55.9537726557485));
#48687=CARTESIAN_POINT('Ctrl Pts',(2.48140697873415,-5.72853683233887,55.8609828971717));
#48688=CARTESIAN_POINT('Ctrl Pts',(0.304164278472461,-6.2354630080913,55.7681931385949));
#48689=CARTESIAN_POINT('Ctrl Pts',(-1.58634824559367,-5.71026665433649,
55.6754033800182));
#48690=CARTESIAN_POINT('Ctrl Pts',(-3.47686076965975,-5.1850703005817,55.5826136214414));
#48691=CARTESIAN_POINT('Ctrl Pts',(-5.0806431175303,-3.62775141731974,55.4898238628647));
#48692=CARTESIAN_POINT('Ctrl Pts',(-5.66117600122224,-1.75349146080347,
55.3970341042879));
#48693=CARTESIAN_POINT('Ctrl Pts',(-5.83564478679751,-1.1902161190413,55.3691478002602));
#48694=CARTESIAN_POINT('Ctrl Pts',(-5.91769412821487,-0.598314798134851,
55.3412614962325));
#48695=CARTESIAN_POINT('Ctrl Pts',(-5.91284273101683,-0.00510202345033239,
55.3133751922048));
#48696=CARTESIAN_POINT('Ctrl Pts',(-5.9173496880968,-0.00543369097055152,
55.0616248077955));
#48697=CARTESIAN_POINT('Ctrl Pts',(-5.92142565083105,-0.444180279760379,
55.0822898403349));
#48698=CARTESIAN_POINT('Ctrl Pts',(-5.8767836491699,-0.882104937779715,
55.1029548728743));
#48699=CARTESIAN_POINT('Ctrl Pts',(-5.78031983552505,-1.30830040099209,
55.1236199054137));
#48700=CARTESIAN_POINT('Ctrl Pts',(-5.34709482638179,-3.22237083290313,
55.2164278566294));
#48701=CARTESIAN_POINT('Ctrl Pts',(-3.8686424355115,-4.89986760772403,55.3092358078451));
#48702=CARTESIAN_POINT('Ctrl Pts',(-2.02416926965118,-5.57014237771353,
55.4020437590608));
#48703=CARTESIAN_POINT('Ctrl Pts',(-0.179696103790855,-6.24041714770303,
55.4948517102765));
#48704=CARTESIAN_POINT('Ctrl Pts',(2.03079783705953,-5.90346991286125,55.5876596614922));
#48705=CARTESIAN_POINT('Ctrl Pts',(3.59180329602535,-4.71409550421518,55.6804676127079));
#48706=CARTESIAN_POINT('Ctrl Pts',(5.15280875499122,-3.52472109556908,55.7732755639237));
#48707=CARTESIAN_POINT('Ctrl Pts',(6.06432573207242,-1.48291951311867,55.8660835151394));
#48708=CARTESIAN_POINT('Ctrl Pts',(5.9075998887394,0.473297892205948,55.9588914663551));
#48709=CARTESIAN_POINT('Ctrl Pts',(5.75087404540639,2.42951529753051,56.0516994175708));
#48710=CARTESIAN_POINT('Ctrl Pts',(4.5259053816591,4.30014852572942,56.1445073687865));
#48711=CARTESIAN_POINT('Ctrl Pts',(2.79544912357091,5.22582161365339,56.2373153200022));
#48712=CARTESIAN_POINT('Ctrl Pts',(1.06499286548277,6.15149470157734,56.3301232712179));
#48713=CARTESIAN_POINT('Ctrl Pts',(-1.17095098694624,6.13220764922659,56.4229312224336));
#48714=CARTESIAN_POINT('Ctrl Pts',(-2.88518139143687,5.17682100122332,56.5157391736493));
#48715=CARTESIAN_POINT('Ctrl Pts',(-4.5994117959276,4.22143435321999,56.608547124865));
#48716=CARTESIAN_POINT('Ctrl Pts',(-5.79192875247984,2.32994810956407,56.7013550760807));
#48717=CARTESIAN_POINT('Ctrl Pts',(-5.91488547174977,0.371318187386364,
56.7941630272965));
#48718=CARTESIAN_POINT('Ctrl Pts',(-5.92259689163941,0.248479697322472,
56.7999836207961));
#48719=CARTESIAN_POINT('Ctrl Pts',(-5.92610134150221,0.12537710671222,56.8058042142958));
#48720=CARTESIAN_POINT('Ctrl Pts',(-5.92550609890763,0.00223999432222687,
56.8116248077954));
#48721=CARTESIAN_POINT('Origin',(0.,0.,-10.));
#48722=CARTESIAN_POINT('',(-5.91438778693357,0.00536108274356934,58.8133751922048));
#48723=CARTESIAN_POINT('',(-5.91049709031373,0.00433299224853631,58.5616248077954));
#48724=CARTESIAN_POINT('',(-5.91675,-7.2459289488551E-16,-10.));
#48725=CARTESIAN_POINT('Ctrl Pts',(-5.91438778693357,0.00536108274356934,
58.8133751922048));
#48726=CARTESIAN_POINT('Ctrl Pts',(-5.91910502988221,0.543269775243645,
58.788071932487));
#48727=CARTESIAN_POINT('Ctrl Pts',(-5.85179376277142,1.08001893776843,58.7627686727691));
#48728=CARTESIAN_POINT('Ctrl Pts',(-5.70776510590029,1.59532552032253,58.7374654130512));
#48729=CARTESIAN_POINT('Ctrl Pts',(-5.17959662293784,3.48500985037694,58.6446756544744));
#48730=CARTESIAN_POINT('Ctrl Pts',(-3.61975776176974,5.08634137467013,58.5518858958976));
#48731=CARTESIAN_POINT('Ctrl Pts',(-1.74458725060383,5.66392631881418,58.4590961373208));
#48732=CARTESIAN_POINT('Ctrl Pts',(0.130583260561965,6.24151126295819,58.3663063787441));
#48733=CARTESIAN_POINT('Ctrl Pts',(2.32108542172547,5.79534962695318,58.2735166201674));
#48734=CARTESIAN_POINT('Ctrl Pts',(3.82095536615163,4.53033620273401,58.1807268615907));
#48735=CARTESIAN_POINT('Ctrl Pts',(5.32082531057801,3.26532277851466,58.0879371030139));
#48736=CARTESIAN_POINT('Ctrl Pts',(6.13006303826679,1.18145756608075,57.9951473444371));
#48737=CARTESIAN_POINT('Ctrl Pts',(5.87703508174782,-0.764267405971718,
57.9023575858603));
#48738=CARTESIAN_POINT('Ctrl Pts',(5.62400712522888,-2.70999237802402,57.8095678272836));
#48739=CARTESIAN_POINT('Ctrl Pts',(4.30871348450246,-4.51757710969499,57.7167780687069));
#48740=CARTESIAN_POINT('Ctrl Pts',(2.53518820261855,-5.35690832451229,57.6239883101301));
#48741=CARTESIAN_POINT('Ctrl Pts',(0.761662920734645,-6.1962395393296,57.5311985515533));
#48742=CARTESIAN_POINT('Ctrl Pts',(-1.4700940023067,-6.06731723729321,57.4384087929765));
#48743=CARTESIAN_POINT('Ctrl Pts',(-3.13517290710431,-5.02934755833045,
57.3456190343997));
#48744=CARTESIAN_POINT('Ctrl Pts',(-4.80025181190193,-3.99137787936768,
57.252829275823));
#48745=CARTESIAN_POINT('Ctrl Pts',(-5.89865269845576,-2.04436082347857,
57.1600395172463));
#48746=CARTESIAN_POINT('Ctrl Pts',(-5.92594711987667,-0.0824424183945678,
57.0672497586696));
#48747=CARTESIAN_POINT('Ctrl Pts',(-5.92632702548814,-0.0551348671611112,
57.0659582365147));
#48748=CARTESIAN_POINT('Ctrl Pts',(-5.92649942241751,-0.0278244290443891,
57.0646667143598));
#48749=CARTESIAN_POINT('Ctrl Pts',(-5.92646560327161,-0.000513552043279186,
57.0633751922049));
#48750=CARTESIAN_POINT('Ctrl Pts',(-5.92550609890763,0.00223999432222687,
56.8116248077954));
#48751=CARTESIAN_POINT('Ctrl Pts',(-5.91661034274359,-1.83801427600624,
56.8986121655115));
#48752=CARTESIAN_POINT('Ctrl Pts',(-4.99206560383895,-3.68597883993112,
56.9855995232275));
#48753=CARTESIAN_POINT('Ctrl Pts',(-3.50994814553166,-4.77535457907361,
57.0725868809436));
#48754=CARTESIAN_POINT('Ctrl Pts',(-1.92865761805595,-5.93762382265653,
57.1653948321593));
#48755=CARTESIAN_POINT('Ctrl Pts',(0.287319918883132,-6.23638870912298,
57.258202783375));
#48756=CARTESIAN_POINT('Ctrl Pts',(2.11995602367751,-5.53439552235597,57.3510107345907));
#48757=CARTESIAN_POINT('Ctrl Pts',(3.95259212847195,-4.83240233558894,57.4438186858064));
#48758=CARTESIAN_POINT('Ctrl Pts',(5.40188680112165,-3.12965107558839,57.5366266370221));
#48759=CARTESIAN_POINT('Ctrl Pts',(5.80202860065573,-1.20839209587507,57.6294345882378));
#48760=CARTESIAN_POINT('Ctrl Pts',(6.20217040018978,0.712866883838148,57.7222425394535));
#48761=CARTESIAN_POINT('Ctrl Pts',(5.55315932660834,2.8526335832641,57.8150504906693));
#48762=CARTESIAN_POINT('Ctrl Pts',(4.15315351590817,4.22789110710056,57.907858441885));
#48763=CARTESIAN_POINT('Ctrl Pts',(2.75314770520792,5.60314863093708,58.0006663931007));
#48764=CARTESIAN_POINT('Ctrl Pts',(0.602147157388864,6.21389697918402,58.0934743443164));
#48765=CARTESIAN_POINT('Ctrl Pts',(-1.31167035990828,5.7795560562329,58.1862822955321));
#48766=CARTESIAN_POINT('Ctrl Pts',(-3.22548787720537,5.3452151332818,58.2790902467478));
#48767=CARTESIAN_POINT('Ctrl Pts',(-4.90212236398056,3.8657849391327,58.3718981979635));
#48768=CARTESIAN_POINT('Ctrl Pts',(-5.57132161087445,2.02092128703809,58.4647061491792));
#48769=CARTESIAN_POINT('Ctrl Pts',(-5.8042682226907,1.37872878754992,58.497012368718));
#48770=CARTESIAN_POINT('Ctrl Pts',(-5.91514199481682,0.692256022528799,
58.5293185882567));
#48771=CARTESIAN_POINT('Ctrl Pts',(-5.91049709031373,0.00433299224853631,
58.5616248077954));
#48772=CARTESIAN_POINT('Origin',(0.,0.,-10.));
#48773=CARTESIAN_POINT('',(-5.90751360641923,-0.00190252881137831,60.5633751922048));
#48774=CARTESIAN_POINT('',(-5.90971954504434,-0.00393376914176207,60.3116248077954));
#48775=CARTESIAN_POINT('',(-5.91675,-7.2459289488551E-16,-10.));
#48776=CARTESIAN_POINT('Ctrl Pts',(-5.90751360641923,-0.00190252881137831,
60.5633751922048));
#48777=CARTESIAN_POINT('Ctrl Pts',(-5.90433409970571,1.10460401303531,60.5114771506141));
#48778=CARTESIAN_POINT('Ctrl Pts',(-5.60641968371212,2.21269985804919,60.4595791090234));
#48779=CARTESIAN_POINT('Ctrl Pts',(-5.0244113679022,3.1430775405676,60.4076810674328));
#48780=CARTESIAN_POINT('Ctrl Pts',(-3.9838246818073,4.80652220822881,60.314891308856));
#48781=CARTESIAN_POINT('Ctrl Pts',(-2.03508282814485,5.9018601064549,60.2221015502792));
#48782=CARTESIAN_POINT('Ctrl Pts',(-0.0731239289288037,5.9260694318362,
60.1293117917025));
#48783=CARTESIAN_POINT('Ctrl Pts',(1.88883497028713,5.9502787572175,60.0365220331257));
#48784=CARTESIAN_POINT('Ctrl Pts',(3.86401091505666,4.90335950975414,59.943732274549));
#48785=CARTESIAN_POINT('Ctrl Pts',(4.94532621967354,3.26609776352986,59.8509425159722));
#48786=CARTESIAN_POINT('Ctrl Pts',(6.02664152429041,1.62883601730559,59.7581527573955));
#48787=CARTESIAN_POINT('Ctrl Pts',(6.21409618875463,-0.598768227679594,
59.6653629988187));
#48788=CARTESIAN_POINT('Ctrl Pts',(5.42160373369846,-2.39371238344798,59.5725732402419));
#48789=CARTESIAN_POINT('Ctrl Pts',(4.6291112786423,-4.18865653921637,59.4797834816652));
#48790=CARTESIAN_POINT('Ctrl Pts',(2.85667170406575,-5.55094060576796,59.3869937230885));
#48791=CARTESIAN_POINT('Ctrl Pts',(0.918258262133265,-5.85495070721773,
59.2942039645117));
#48792=CARTESIAN_POINT('Ctrl Pts',(-1.02015517979933,-6.15896080866752,
59.201414205935));
#48793=CARTESIAN_POINT('Ctrl Pts',(-3.12454248908787,-5.40469694501536,
59.1086244473581));
#48794=CARTESIAN_POINT('Ctrl Pts',(-4.42848709135374,-3.93854644528139,
59.0158346887814));
#48795=CARTESIAN_POINT('Ctrl Pts',(-5.37685313155668,-2.87220716878292,
58.9483481899225));
#48796=CARTESIAN_POINT('Ctrl Pts',(-5.90180639566545,-1.42929890839187,
58.8808616910637));
#48797=CARTESIAN_POINT('Ctrl Pts',(-5.91438778693357,0.00536108274356934,
58.8133751922048));
#48798=CARTESIAN_POINT('Ctrl Pts',(-5.91049709031373,0.00433299224853631,
58.5616248077954));
#48799=CARTESIAN_POINT('Ctrl Pts',(-5.90179830816206,-1.28398037857263,
58.6221265394724));
#48800=CARTESIAN_POINT('Ctrl Pts',(-5.48794981324838,-2.57738015247874,
58.6826282711494));
#48801=CARTESIAN_POINT('Ctrl Pts',(-4.71200052329397,-3.5945512110245,58.7431300028264));
#48802=CARTESIAN_POINT('Ctrl Pts',(-3.52171618180695,-5.15486294695242,
58.8359379540421));
#48803=CARTESIAN_POINT('Ctrl Pts',(-1.47938349182042,-6.06518930876796,
58.9287459052578));
#48804=CARTESIAN_POINT('Ctrl Pts',(0.476742202929665,-5.90732293108699,
59.0215538564735));
#48805=CARTESIAN_POINT('Ctrl Pts',(2.43286789767958,-5.74945655340603,59.1143618076892));
#48806=CARTESIAN_POINT('Ctrl Pts',(4.30278659719299,-4.52339743622863,59.2071697589049));
#48807=CARTESIAN_POINT('Ctrl Pts',(5.22745059549495,-2.79240176404826,59.2999777101206));
#48808=CARTESIAN_POINT('Ctrl Pts',(6.15211459379697,-1.06140609186779,59.3927856613363));
#48809=CARTESIAN_POINT('Ctrl Pts',(6.13152389088747,1.17452613531577,59.4855936125521));
#48810=CARTESIAN_POINT('Ctrl Pts',(5.17513793337419,2.88819921590459,59.5784015637678));
#48811=CARTESIAN_POINT('Ctrl Pts',(4.21875197586095,4.60187229649331,59.6712095149835));
#48812=CARTESIAN_POINT('Ctrl Pts',(2.326570763744,5.79328623048741,59.7640174661991));
#48813=CARTESIAN_POINT('Ctrl Pts',(0.367869485287327,5.9151009612681,59.8568254174148));
#48814=CARTESIAN_POINT('Ctrl Pts',(-1.59083179316951,6.0369156920488,59.9496333686306));
#48815=CARTESIAN_POINT('Ctrl Pts',(-3.61605313796599,5.089131219616,60.0424413198463));
#48816=CARTESIAN_POINT('Ctrl Pts',(-4.77740022190952,3.50716330670518,60.135249271062));
#48817=CARTESIAN_POINT('Ctrl Pts',(-5.51308867884712,2.50502058049953,60.1940411166398));
#48818=CARTESIAN_POINT('Ctrl Pts',(-5.90210866022388,1.24838317086696,60.2528329622176));
#48819=CARTESIAN_POINT('Ctrl Pts',(-5.90971954504434,-0.00393376914176207,
60.3116248077954));
#48820=CARTESIAN_POINT('Origin',(0.,0.,-10.));
#48821=CARTESIAN_POINT('',(-5.92138577511996,-0.00465600546497968,62.3133751922048));
#48822=CARTESIAN_POINT('',(-5.92487552954592,-0.00283239076988535,62.0616248077954));
#48823=CARTESIAN_POINT('',(-5.91675,-7.2459289488551E-16,-10.));
#48824=CARTESIAN_POINT('Ctrl Pts',(-5.92138577511996,-0.00465600546497968,
62.3133751922048));
#48825=CARTESIAN_POINT('Ctrl Pts',(-5.90702696023975,1.65892609794656,62.2348823687413));
#48826=CARTESIAN_POINT('Ctrl Pts',(-5.17355864322008,3.33359211408665,62.1563895452778));
#48827=CARTESIAN_POINT('Ctrl Pts',(-3.93157790275368,4.43467487134112,62.0778967218143));
#48828=CARTESIAN_POINT('Ctrl Pts',(-2.46337879894035,5.73631238048495,61.9851069632376));
#48829=CARTESIAN_POINT('Ctrl Pts',(-0.284552613138903,6.23638875022473,
61.8923172046609));
#48830=CARTESIAN_POINT('Ctrl Pts',(1.60429885033706,5.70524944404121,61.7995274460841));
#48831=CARTESIAN_POINT('Ctrl Pts',(3.49315031381303,5.17411013785769,61.7067376875074));
#48832=CARTESIAN_POINT('Ctrl Pts',(5.09202705496358,3.61175515575085,61.6139479289306));
#48833=CARTESIAN_POINT('Ctrl Pts',(5.66666263138229,1.73567872661414,61.5211581703538));
#48834=CARTESIAN_POINT('Ctrl Pts',(6.24129820780094,-0.140397702522356,
61.428368411777));
#48835=CARTESIAN_POINT('Ctrl Pts',(5.79169261948807,-2.3301955786887,61.3355786532003));
#48836=CARTESIAN_POINT('Ctrl Pts',(4.52432225534832,-3.82807447023764,61.2427888946235));
#48837=CARTESIAN_POINT('Ctrl Pts',(3.2569518912085,-5.32595336178667,61.1499991360468));
#48838=CARTESIAN_POINT('Ctrl Pts',(1.17181675124172,-6.13191326871823,61.05720937747));
#48839=CARTESIAN_POINT('Ctrl Pts',(-0.773507935796127,-5.87582602645669,
60.9644196188933));
#48840=CARTESIAN_POINT('Ctrl Pts',(-2.71883262283403,-5.61973878419514,
60.8716298603165));
#48841=CARTESIAN_POINT('Ctrl Pts',(-4.52434685694288,-4.30160439274053,
60.7788401017398));
#48842=CARTESIAN_POINT('Ctrl Pts',(-5.36088821473366,-2.52676147846508,
60.686050343163));
#48843=CARTESIAN_POINT('Ctrl Pts',(-5.72954541327163,-1.74460216197929,
60.645158626177));
#48844=CARTESIAN_POINT('Ctrl Pts',(-5.91001881634045,-0.873745684460358,
60.6042669091909));
#48845=CARTESIAN_POINT('Ctrl Pts',(-5.90751360641923,-0.00190252881137831,
60.5633751922048));
#48846=CARTESIAN_POINT('Ctrl Pts',(-5.90971954504434,-0.00393376914176207,
60.3116248077954));
#48847=CARTESIAN_POINT('Ctrl Pts',(-5.91412309216056,-0.728506112548232,
60.3456409134333));
#48848=CARTESIAN_POINT('Ctrl Pts',(-5.79084570775551,-1.45163213075908,
60.3796570190712));
#48849=CARTESIAN_POINT('Ctrl Pts',(-5.533158553854,-2.12318245992016,60.4136731247091));
#48850=CARTESIAN_POINT('Ctrl Pts',(-4.83009697876454,-3.95540896024582,
60.5064810759248));
#48851=CARTESIAN_POINT('Ctrl Pts',(-3.12650100549514,-5.40371060750862,
60.5992890271406));
#48852=CARTESIAN_POINT('Ctrl Pts',(-1.2050090520295,-5.80273216034717,60.6920969783563));
#48853=CARTESIAN_POINT('Ctrl Pts',(0.716482901436298,-6.20175371318575,
60.784904929572));
#48854=CARTESIAN_POINT('Ctrl Pts',(2.85587083509837,-5.55149517160003,60.8777128807877));
#48855=CARTESIAN_POINT('Ctrl Pts',(4.23031186007554,-4.15068776309476,60.9705208320034));
#48856=CARTESIAN_POINT('Ctrl Pts',(5.60475288505267,-2.74988035458953,61.0633287832191));
#48857=CARTESIAN_POINT('Ctrl Pts',(6.21424700134487,-0.598524079164734,
61.1561367344349));
#48858=CARTESIAN_POINT('Ctrl Pts',(5.77879031223601,1.31503987293452,61.2489446856506));
#48859=CARTESIAN_POINT('Ctrl Pts',(5.34333362312715,3.22860382503377,61.3417526368663));
#48860=CARTESIAN_POINT('Ctrl Pts',(3.86292612861721,4.90437545380759,61.434560588082));
#48861=CARTESIAN_POINT('Ctrl Pts',(2.01767261743198,5.57249895011794,61.5273685392977));
#48862=CARTESIAN_POINT('Ctrl Pts',(0.172419106246808,6.24062244642827,61.6201764905134));
#48863=CARTESIAN_POINT('Ctrl Pts',(-2.03768042161353,5.90109781027533,61.7129844417291));
#48864=CARTESIAN_POINT('Ctrl Pts',(-3.59729790409035,4.70990394057326,61.8057923929448));
#48865=CARTESIAN_POINT('Ctrl Pts',(-5.03036731089132,3.61536408614182,61.8910698645617));
#48866=CARTESIAN_POINT('Ctrl Pts',(-5.9142328668594,1.80175746265739,61.9763473361785));
#48867=CARTESIAN_POINT('Ctrl Pts',(-5.92487552954592,-0.00283239076988535,
62.0616248077954));
#48868=CARTESIAN_POINT('Origin',(0.,0.,-10.));
#48869=CARTESIAN_POINT('',(-5.92254374065673,0.00421469164317803,64.0633751922048));
#48870=CARTESIAN_POINT('',(-5.9184608786744,0.00532413147862563,63.8116248077953));
#48871=CARTESIAN_POINT('',(-5.91675,-7.2459289488551E-16,-10.));
#48872=CARTESIAN_POINT('Ctrl Pts',(-5.92254374065673,0.00421469164317803,
64.0633751922048));
#48873=CARTESIAN_POINT('Ctrl Pts',(-5.92464260024143,0.264723398301747,
64.0510773454453));
#48874=CARTESIAN_POINT('Ctrl Pts',(-5.90894822076181,0.524977554909748,
64.0387794986858));
#48875=CARTESIAN_POINT('Ctrl Pts',(-5.87460244218337,0.782746552990558,
64.0264816519262));
#48876=CARTESIAN_POINT('Ctrl Pts',(-5.61545654739851,2.72766614486684,63.9336918933495));
#48877=CARTESIAN_POINT('Ctrl Pts',(-4.29448466452766,4.53110541697169,63.8409021347727));
#48878=CARTESIAN_POINT('Ctrl Pts',(-2.51832850646255,5.36485484924461,63.748112376196));
#48879=CARTESIAN_POINT('Ctrl Pts',(-0.742172348397438,6.19860428151754,
63.6553226176192));
#48880=CARTESIAN_POINT('Ctrl Pts',(1.48916808486193,6.06266387395855,63.5625328590425));
#48881=CARTESIAN_POINT('Ctrl Pts',(3.15097440223581,5.01946275375961,63.4697431004657));
#48882=CARTESIAN_POINT('Ctrl Pts',(4.81278071960959,3.97626163356074,63.376953341889));
#48883=CARTESIAN_POINT('Ctrl Pts',(5.90505292109795,2.02579980072203,63.2841635833122));
#48884=CARTESIAN_POINT('Ctrl Pts',(5.92617709057818,0.063805258652316,63.1913738247354));
#48885=CARTESIAN_POINT('Ctrl Pts',(5.94730126005842,-1.89818928341785,63.0985840661587));
#48886=CARTESIAN_POINT('Ctrl Pts',(4.89727739752999,-3.87171653471903,63.0057943075819));
#48887=CARTESIAN_POINT('Ctrl Pts',(3.2583173371746,-4.95045595376757,62.9130045490052));
#48888=CARTESIAN_POINT('Ctrl Pts',(1.61935727681958,-6.02919537281587,62.8202147904284));
#48889=CARTESIAN_POINT('Ctrl Pts',(-0.608538981362105,-6.21314695961199,
62.7274250318516));
#48890=CARTESIAN_POINT('Ctrl Pts',(-2.40223474556518,-5.41783298442511,
62.6346352732749));
#48891=CARTESIAN_POINT('Ctrl Pts',(-4.19593050976836,-4.62251900923819,
62.5418455146981));
#48892=CARTESIAN_POINT('Ctrl Pts',(-5.55542577999287,-2.84793947206817,
62.4490557561214));
#48893=CARTESIAN_POINT('Ctrl Pts',(-5.85638740419252,-0.909050379209287,
62.3562659975446));
#48894=CARTESIAN_POINT('Ctrl Pts',(-5.90275921158555,-0.610308664847524,
62.3419690624314));
#48895=CARTESIAN_POINT('Ctrl Pts',(-5.9240011358063,-0.30766619593341,62.3276721273181));
#48896=CARTESIAN_POINT('Ctrl Pts',(-5.92138577511996,-0.00465600546497968,
62.3133751922048));
#48897=CARTESIAN_POINT('Ctrl Pts',(-5.92487552954592,-0.00283239076988535,
62.0616248077954));
#48898=CARTESIAN_POINT('Ctrl Pts',(-5.92581533642245,-0.162187808066437,
62.0691552873942));
#48899=CARTESIAN_POINT('Ctrl Pts',(-5.91994585449146,-0.3214729136569,62.0766857669931));
#48900=CARTESIAN_POINT('Ctrl Pts',(-5.90704396529663,-0.480186351589765,
62.0842162465919));
#48901=CARTESIAN_POINT('Ctrl Pts',(-5.74803710693276,-2.43621967079874,
62.1770241978076));
#48902=CARTESIAN_POINT('Ctrl Pts',(-4.52088795311218,-4.30542320596569,
62.2698321490233));
#48903=CARTESIAN_POINT('Ctrl Pts',(-2.78935345527504,-5.22907780031484,
62.3626401002391));
#48904=CARTESIAN_POINT('Ctrl Pts',(-1.05781895743761,-6.15273239466415,
62.4554480514548));
#48905=CARTESIAN_POINT('Ctrl Pts',(1.17810088441637,-6.13083804819549,62.5482560026705));
#48906=CARTESIAN_POINT('Ctrl Pts',(2.89121605855662,-5.17345310628643,62.6410639538862));
#48907=CARTESIAN_POINT('Ctrl Pts',(4.60433123269666,-4.21606816437748,62.7338719051019));
#48908=CARTESIAN_POINT('Ctrl Pts',(5.79464173912287,-2.32319262702822,62.8266798563176));
#48909=CARTESIAN_POINT('Ctrl Pts',(5.91531444000447,-0.364420658134239,
62.9194878075333));
#48910=CARTESIAN_POINT('Ctrl Pts',(6.03598714088608,1.59435131075997,63.012295758749));
#48911=CARTESIAN_POINT('Ctrl Pts',(5.08702203622284,3.61901971119909,63.1051037099647));
#48912=CARTESIAN_POINT('Ctrl Pts',(3.50437727565169,4.77944424071423,63.1979116611804));
#48913=CARTESIAN_POINT('Ctrl Pts',(1.92173251508063,5.93986877022931,63.2907196123961));
#48914=CARTESIAN_POINT('Ctrl Pts',(-0.294591901398011,6.23604942882064,
63.3835275636119));
#48915=CARTESIAN_POINT('Ctrl Pts',(-2.12640817440725,5.53191970440772,63.4763355148276));
#48916=CARTESIAN_POINT('Ctrl Pts',(-3.95822444741638,4.82778997999483,63.5691434660433));
#48917=CARTESIAN_POINT('Ctrl Pts',(-5.40553257695601,3.12334987257762,63.661951417259));
#48918=CARTESIAN_POINT('Ctrl Pts',(-5.80343374745539,1.20162559855231,63.7547593684747));
#48919=CARTESIAN_POINT('Ctrl Pts',(-5.88470129896102,0.809131587481785,
63.7737145149149));
#48920=CARTESIAN_POINT('Ctrl Pts',(-5.92219367890825,0.407573741272489,
63.7926696613551));
#48921=CARTESIAN_POINT('Ctrl Pts',(-5.9184608786744,0.00532413147862563,
63.8116248077953));
#48922=CARTESIAN_POINT('Origin',(0.,0.,-10.));
#48923=CARTESIAN_POINT('',(-5.90799290133436,0.00254793967829986,65.8133751922048));
#48924=CARTESIAN_POINT('',(-5.90695594955463,0.000339959333261384,65.5616248077954));
#48925=CARTESIAN_POINT('',(-5.91675,-7.2459289488551E-16,-10.));
#48926=CARTESIAN_POINT('Ctrl Pts',(-5.90799290133436,0.00254793967829986,
65.8133751922048));
#48927=CARTESIAN_POINT('Ctrl Pts',(-5.91119872342175,0.8316010093993,65.7744825635725));
#48928=CARTESIAN_POINT('Ctrl Pts',(-5.7485847983095,1.65945254838475,65.7355899349402));
#48929=CARTESIAN_POINT('Ctrl Pts',(-5.41404883863568,2.41075116774689,65.6966973063079));
#48930=CARTESIAN_POINT('Ctrl Pts',(-4.61591530986757,4.20319410516615,65.6039075477311));
#48931=CARTESIAN_POINT('Ctrl Pts',(-2.83920019805476,5.55989721747976,65.5111177891543));
#48932=CARTESIAN_POINT('Ctrl Pts',(-0.899840248503511,5.85780962025043,
65.4183280305776));
#48933=CARTESIAN_POINT('Ctrl Pts',(1.03951970104785,6.15572202302112,65.3255382720008));
#48934=CARTESIAN_POINT('Ctrl Pts',(3.14152448833767,5.39484371624875,65.2327485134241));
#48935=CARTESIAN_POINT('Ctrl Pts',(4.44085168583864,3.92459963872871,65.1399587548473));
#48936=CARTESIAN_POINT('Ctrl Pts',(5.74017888333953,2.45435556120876,65.0471689962706));
#48937=CARTESIAN_POINT('Ctrl Pts',(6.23682849105167,0.274745712941213,64.9543792376938));
#48938=CARTESIAN_POINT('Ctrl Pts',(5.70271967497977,-1.61326821344872,64.861589479117));
#48939=CARTESIAN_POINT('Ctrl Pts',(5.1686108589079,-3.50128213983854,64.7687997205403));
#48940=CARTESIAN_POINT('Ctrl Pts',(3.60374361905212,-5.09770014435078,64.6760099619635));
#48941=CARTESIAN_POINT('Ctrl Pts',(1.72676591086401,-5.66938493216004,64.5832202033868));
#48942=CARTESIAN_POINT('Ctrl Pts',(-0.150211797324312,-6.24106971996937,
64.49043044481));
#48943=CARTESIAN_POINT('Ctrl Pts',(-2.33929997384504,-5.78802129107543,
64.3976406862333));
#48944=CARTESIAN_POINT('Ctrl Pts',(-3.83518410875603,-4.51829712080455,
64.3048509276565));
#48945=CARTESIAN_POINT('Ctrl Pts',(-5.13281194746251,-3.41685524280773,
64.2243590158393));
#48946=CARTESIAN_POINT('Ctrl Pts',(-5.90880627718756,-1.7008678528067,64.1438671040221));
#48947=CARTESIAN_POINT('Ctrl Pts',(-5.92254374065673,0.00421469164317803,
64.0633751922048));
#48948=CARTESIAN_POINT('Ctrl Pts',(-5.9184608786744,0.00532413147862563,
63.8116248077953));
#48949=CARTESIAN_POINT('Ctrl Pts',(-5.90391718903288,-1.56191577335664,
63.8854776125708));
#48950=CARTESIAN_POINT('Ctrl Pts',(-5.26356384080163,-3.1396568410927,63.9593304173463));
#48951=CARTESIAN_POINT('Ctrl Pts',(-4.14822059929475,-4.23273117499648,
64.0331832221218));
#48952=CARTESIAN_POINT('Ctrl Pts',(-2.74661206917558,-5.60635523388617,
64.1259911733375));
#48953=CARTESIAN_POINT('Ctrl Pts',(-0.594900797478113,-6.21459491103191,
64.2187991245533));
#48954=CARTESIAN_POINT('Ctrl Pts',(1.31840893892553,-5.77802260379462,64.311607075769));
#48955=CARTESIAN_POINT('Ctrl Pts',(3.23171867532906,-5.34145029655737,64.4044150269847));
#48956=CARTESIAN_POINT('Ctrl Pts',(4.90662687643879,-3.86006600493721,64.4972229782003));
#48957=CARTESIAN_POINT('Ctrl Pts',(5.57367439504355,-2.01442326193784,64.590030929416));
#48958=CARTESIAN_POINT('Ctrl Pts',(6.24072191364835,-0.168780518938366,
64.6828388806317));
#48959=CARTESIAN_POINT('Ctrl Pts',(5.89990874974806,2.04112067544036,64.7756468318475));
#48960=CARTESIAN_POINT('Ctrl Pts',(4.70780575676577,3.60004337428919,64.8684547830633));
#48961=CARTESIAN_POINT('Ctrl Pts',(3.51570276378348,5.15896607313801,64.961262734279));
#48962=CARTESIAN_POINT('Ctrl Pts',(1.47230994171919,6.06691027645692,65.0540706854946));
#48963=CARTESIAN_POINT('Ctrl Pts',(-0.48363033701444,5.90676299146323,65.1468786367103));
#48964=CARTESIAN_POINT('Ctrl Pts',(-2.43957061574796,5.74661570646955,65.239686587926));
#48965=CARTESIAN_POINT('Ctrl Pts',(-4.30805835115084,4.51837693316338,65.3324945391418));
#48966=CARTESIAN_POINT('Ctrl Pts',(-5.23070322755976,2.7863041982878,65.4253024903575));
#48967=CARTESIAN_POINT('Ctrl Pts',(-5.68245003760025,1.93824406947249,65.4707432628368));
#48968=CARTESIAN_POINT('Ctrl Pts',(-5.90745064133749,0.969400199144218,
65.5161840353161));
#48969=CARTESIAN_POINT('Ctrl Pts',(-5.90695594955463,0.000339959333261384,
65.5616248077954));
#48970=CARTESIAN_POINT('Origin',(0.,0.,-10.));
#48971=CARTESIAN_POINT('',(-5.91318264661351,-0.00517381203793132,67.5633751922048));
#48972=CARTESIAN_POINT('',(-5.91720892724047,-0.00544236320477147,67.3116248077954));
#48973=CARTESIAN_POINT('',(-5.91675,-7.2459289488551E-16,-10.));
#48974=CARTESIAN_POINT('Ctrl Pts',(-5.91318264661351,-0.00517381203793133,
67.5633751922048));
#48975=CARTESIAN_POINT('Ctrl Pts',(-5.90158111533912,1.3877078186906,67.4978877816997));
#48976=CARTESIAN_POINT('Ctrl Pts',(-5.4100418655732,2.78795772811743,67.4324003711946));
#48977=CARTESIAN_POINT('Ctrl Pts',(-4.51226081400018,3.84228426412776,67.3669129606895));
#48978=CARTESIAN_POINT('Ctrl Pts',(-3.24018597720788,5.33616994357178,67.2741232021127));
#48979=CARTESIAN_POINT('Ctrl Pts',(-1.15252645285901,6.13556823847911,67.1813334435359));
#48980=CARTESIAN_POINT('Ctrl Pts',(0.791983234710277,5.87336433195347,67.0885436849592));
#48981=CARTESIAN_POINT('Ctrl Pts',(2.73649292227957,5.61116042542782,66.9957539263824));
#48982=CARTESIAN_POINT('Ctrl Pts',(4.53785277306916,4.28735431746923,66.9029641678057));
#48983=CARTESIAN_POINT('Ctrl Pts',(5.36880821823668,2.50988930746351,66.8101744092289));
#48984=CARTESIAN_POINT('Ctrl Pts',(6.19976366340414,0.732424297457894,66.7173846506522));
#48985=CARTESIAN_POINT('Ctrl Pts',(6.0603147029495,-1.498699614595,66.6245948920754));
#48986=CARTESIAN_POINT('Ctrl Pts',(5.01450172813933,-3.15886347258204,66.5318051334987));
#48987=CARTESIAN_POINT('Ctrl Pts',(3.96868875332904,-4.81902733056926,66.4390153749219));
#48988=CARTESIAN_POINT('Ctrl Pts',(2.01651176416312,-5.90823113449073,66.3462256163452));
#48989=CARTESIAN_POINT('Ctrl Pts',(0.0544864306054393,-5.92627009583644,
66.2534358577684));
#48990=CARTESIAN_POINT('Ctrl Pts',(-1.90753890295213,-5.94430905718215,
66.1606460991917));
#48991=CARTESIAN_POINT('Ctrl Pts',(-3.87941258090134,-4.89118317595221,
66.0678563406149));
#48992=CARTESIAN_POINT('Ctrl Pts',(-4.95557344701427,-3.25052885407475,
65.9750665820381));
#48993=CARTESIAN_POINT('Ctrl Pts',(-5.58066379029856,-2.29755127835456,
65.9211694520937));
#48994=CARTESIAN_POINT('Ctrl Pts',(-5.9035502957379,-1.14634794627538,65.8672723221492));
#48995=CARTESIAN_POINT('Ctrl Pts',(-5.90799290133436,0.00254793967829986,
65.8133751922048));
#48996=CARTESIAN_POINT('Ctrl Pts',(-5.90695594955463,0.000339959333261384,
65.5616248077954));
#48997=CARTESIAN_POINT('Ctrl Pts',(-5.90644028591556,-1.00980241019597,
65.6089919865318));
#48998=CARTESIAN_POINT('Ctrl Pts',(-5.66090486185914,-2.02017988351609,
65.6563591652682));
#48999=CARTESIAN_POINT('Ctrl Pts',(-5.17176652053277,-2.8942319183674,65.7037263440046));
#49000=CARTESIAN_POINT('Ctrl Pts',(-4.21338291968193,-4.60678860370172,
65.7965342952203));
#49001=CARTESIAN_POINT('Ctrl Pts',(-2.31981370056542,-5.79599527792531,
65.8893422464361));
#49002=CARTESIAN_POINT('Ctrl Pts',(-0.360971707099837,-5.91552590788628,
65.9821501976517));
#49003=CARTESIAN_POINT('Ctrl Pts',(1.59787028636575,-6.03505653784725,66.0749581488675));
#49004=CARTESIAN_POINT('Ctrl Pts',(3.62198505418061,-5.08491112354539,66.1677661000831));
#49005=CARTESIAN_POINT('Ctrl Pts',(4.7814866347922,-3.5015900533192,66.2605740512988));
#49006=CARTESIAN_POINT('Ctrl Pts',(5.94098821540385,-1.91826898309292,66.3533820025146));
#49007=CARTESIAN_POINT('Ctrl Pts',(6.23587660881247,0.298227743057843,66.4461899537303));
#49008=CARTESIAN_POINT('Ctrl Pts',(5.53067897443825,2.12963316604222,66.538997904946));
#49009=CARTESIAN_POINT('Ctrl Pts',(4.82548134006407,3.96103858902649,66.6318058561617));
#49010=CARTESIAN_POINT('Ctrl Pts',(3.12019767790724,5.40735270884429,66.7246138073774));
#49011=CARTESIAN_POINT('Ctrl Pts',(1.19824173659399,5.80413336174183,66.8174217585931));
#49012=CARTESIAN_POINT('Ctrl Pts',(-0.723714204719369,6.2009140146394,66.9102297098088));
#49013=CARTESIAN_POINT('Ctrl Pts',(-2.86234242518905,5.54816120061654,67.0030376610246));
#49014=CARTESIAN_POINT('Ctrl Pts',(-4.23514905104094,4.14575202534684,67.0958456122403));
#49015=CARTESIAN_POINT('Ctrl Pts',(-5.29907768179141,3.05888134341762,67.1677720107587));
#49016=CARTESIAN_POINT('Ctrl Pts',(-5.90303169463259,1.52174535067564,67.239698409277));
#49017=CARTESIAN_POINT('Ctrl Pts',(-5.91720892724047,-0.00544236320477147,
67.3116248077954));
#49018=CARTESIAN_POINT('Origin',(0.,0.,-10.));
#49019=CARTESIAN_POINT('',(-5.92650388951378,-0.000281712456556837,69.3133751922048));
#49020=CARTESIAN_POINT('',(-5.92557665873441,0.00216209314576762,69.0616248077954));
#49021=CARTESIAN_POINT('',(-5.91675,-7.2459289488551E-16,-10.));
#49022=CARTESIAN_POINT('Ctrl Pts',(-5.92650388951378,-0.000281712456556837,
69.3133751922048));
#49023=CARTESIAN_POINT('Ctrl Pts',(-5.92515963032167,1.94687933134679,69.2212929998269));
#49024=CARTESIAN_POINT('Ctrl Pts',(-4.87255319916288,3.89528559185528,69.129210807449));
#49025=CARTESIAN_POINT('Ctrl Pts',(-3.24273233348756,4.96067868676048,69.0371286150711));
#49026=CARTESIAN_POINT('Ctrl Pts',(-1.60038780688532,6.0342583389466,68.9443388564943));
#49027=CARTESIAN_POINT('Ctrl Pts',(0.628075950420943,6.21120241451497,68.8515490979176));
#49028=CARTESIAN_POINT('Ctrl Pts',(2.41926162893542,5.41025130568684,68.7587593393408));
#49029=CARTESIAN_POINT('Ctrl Pts',(4.21044730744979,4.60930019685875,68.6659695807641));
#49030=CARTESIAN_POINT('Ctrl Pts',(5.56435490717254,2.83045390363422,68.5731798221873));
#49031=CARTESIAN_POINT('Ctrl Pts',(5.85921735187489,0.890627892788898,68.4803900636105));
#49032=CARTESIAN_POINT('Ctrl Pts',(6.15407979657726,-1.04919811805653,68.3876003050338));
#49033=CARTESIAN_POINT('Ctrl Pts',(5.3898970862593,-3.15000384652261,68.294810546457));
#49034=CARTESIAN_POINT('Ctrl Pts',(3.91761167046192,-4.44701751957263,68.2020207878803));
#49035=CARTESIAN_POINT('Ctrl Pts',(2.44532625466471,-5.7440311926225,68.1092310293035));
#49036=CARTESIAN_POINT('Ctrl Pts',(0.26493813338821,-6.23725281025625,68.0164412707268));
#49037=CARTESIAN_POINT('Ctrl Pts',(-1.62223358747919,-5.70017580497126,
67.92365151215));
#49038=CARTESIAN_POINT('Ctrl Pts',(-3.5094053083468,-5.16309879968621,67.8308617535733));
#49039=CARTESIAN_POINT('Ctrl Pts',(-5.10336062880535,-3.5957231714821,67.7380719949965));
#49040=CARTESIAN_POINT('Ctrl Pts',(-5.67209321441677,-1.71784882538965,
67.6452822364198));
#49041=CARTESIAN_POINT('Ctrl Pts',(-5.83943641317296,-1.16530531392642,
67.6179798883481));
#49042=CARTESIAN_POINT('Ctrl Pts',(-5.91801943955699,-0.585879917401179,
67.5906775402765));
#49043=CARTESIAN_POINT('Ctrl Pts',(-5.91318264661351,-0.00517381203793133,
67.5633751922048));
#49044=CARTESIAN_POINT('Ctrl Pts',(-5.91720892724047,-0.00544236320477147,
67.3116248077954));
#49045=CARTESIAN_POINT('Ctrl Pts',(-5.92132483789222,-0.44881296680819,
67.3325063604927));
#49046=CARTESIAN_POINT('Ctrl Pts',(-5.87573156645681,-0.891345082322613,
67.3533879131901));
#49047=CARTESIAN_POINT('Ctrl Pts',(-5.77725293116981,-1.3217775567357,67.3742694658874));
#49048=CARTESIAN_POINT('Ctrl Pts',(-5.33956515421279,-3.23483242703241,
67.4670774171031));
#49049=CARTESIAN_POINT('Ctrl Pts',(-3.85720456906464,-4.90887663110927,
67.5598853683188));
#49050=CARTESIAN_POINT('Ctrl Pts',(-2.01117322165947,-5.57484794525198,
67.6526933195345));
#49051=CARTESIAN_POINT('Ctrl Pts',(-0.165141874254405,-6.24081925939465,
67.7455012707502));
#49052=CARTESIAN_POINT('Ctrl Pts',(2.04456023540753,-5.89871768360324,67.8383092219659));
#49053=CARTESIAN_POINT('Ctrl Pts',(3.60278762068745,-4.70570597258494,67.9311171731817));
#49054=CARTESIAN_POINT('Ctrl Pts',(5.16101500596746,-3.51269426156657,68.0239251243974));
#49055=CARTESIAN_POINT('Ctrl Pts',(6.06776766686524,-1.46877241532123,68.1167330756131));
#49056=CARTESIAN_POINT('Ctrl Pts',(5.90648000968226,0.487074158033609,68.2095410268288));
#49057=CARTESIAN_POINT('Ctrl Pts',(5.74519235249929,2.44292073138834,68.3023489780444));
#49058=CARTESIAN_POINT('Ctrl Pts',(4.51586437723545,4.31069203185281,68.3951569292602));
#49059=CARTESIAN_POINT('Ctrl Pts',(2.78325399412311,5.23232687667715,68.4879648804759));
#49060=CARTESIAN_POINT('Ctrl Pts',(1.05064361101067,6.15396172150155,68.5807728316916));
#49061=CARTESIAN_POINT('Ctrl Pts',(-1.18524917995037,6.129460110686,68.6735807829073));
#49062=CARTESIAN_POINT('Ctrl Pts',(-2.89724679431174,5.17007817668657,68.7663887341231));
#49063=CARTESIAN_POINT('Ctrl Pts',(-4.60924440867302,4.21069624268719,68.8591966853388));
#49064=CARTESIAN_POINT('Ctrl Pts',(-5.7973468464346,2.31643398550408,68.9520046365544));
#49065=CARTESIAN_POINT('Ctrl Pts',(-5.91573536484165,0.357522633356556,
69.0448125877702));
#49066=CARTESIAN_POINT('Ctrl Pts',(-5.92288408358054,0.239236616440886,
69.0504166611119));
#49067=CARTESIAN_POINT('Ctrl Pts',(-5.92613244049811,0.120714877752119,
69.0560207344536));
#49068=CARTESIAN_POINT('Ctrl Pts',(-5.92557665873441,0.00216209314576762,
69.0616248077954));
#49069=CARTESIAN_POINT('Origin',(0.,0.,-10.));
#49070=CARTESIAN_POINT('',(-5.91402970906047,0.00531590772330143,71.0633751922048));
#49071=CARTESIAN_POINT('',(-5.91060120235062,0.00437987123653664,70.8116248077954));
#49072=CARTESIAN_POINT('',(-5.91675,-7.2459289488551E-16,-10.));
#49073=CARTESIAN_POINT('Ctrl Pts',(-5.91402970906047,0.00531590772330143,
71.0633751922048));
#49074=CARTESIAN_POINT('Ctrl Pts',(-5.91879269344977,0.555723161917816,
71.0374879765309));
#49075=CARTESIAN_POINT('Ctrl Pts',(-5.84828352000433,1.10493322756756,71.0116007608569));
#49076=CARTESIAN_POINT('Ctrl Pts',(-5.69761784030547,1.63119495026137,70.985713545183));
#49077=CARTESIAN_POINT('Ctrl Pts',(-5.15757397382148,3.5175197992524,70.8929237866062));
#49078=CARTESIAN_POINT('Ctrl Pts',(-3.5876938328729,5.10900849433029,70.8001340280294));
#49079=CARTESIAN_POINT('Ctrl Pts',(-1.70892749224105,5.67478747145548,70.7073442694526));
#49080=CARTESIAN_POINT('Ctrl Pts',(0.16983884839081,6.24056644858066,70.6145545108759));
#49081=CARTESIAN_POINT('Ctrl Pts',(2.35749138870594,5.78063570775315,70.5217647522992));
#49082=CARTESIAN_POINT('Ctrl Pts',(3.84937491879597,4.50621334986148,70.4289749937224));
#49083=CARTESIAN_POINT('Ctrl Pts',(5.341258448886,3.23179099196982,70.3361852351457));
#49084=CARTESIAN_POINT('Ctrl Pts',(6.13737296875093,1.14287701701401,70.2433954765689));
#49085=CARTESIAN_POINT('Ctrl Pts',(5.87211169882839,-0.801217958116352,
70.1506057179922));
#49086=CARTESIAN_POINT('Ctrl Pts',(5.60685042890584,-2.74531293324682,70.0578159594154));
#49087=CARTESIAN_POINT('Ctrl Pts',(4.28021336919569,-4.54458890855182,69.9650262008387));
#49088=CARTESIAN_POINT('Ctrl Pts',(2.50144390233472,-5.37274831193476,69.8722364422619));
#49089=CARTESIAN_POINT('Ctrl Pts',(0.722674435473843,-6.20090771531765,
69.7794466836851));
#49090=CARTESIAN_POINT('Ctrl Pts',(-1.50822743853782,-6.05795054677859,
69.6866569251084));
#49091=CARTESIAN_POINT('Ctrl Pts',(-3.16674473209977,-5.00952830330798,
69.5938671665316));
#49092=CARTESIAN_POINT('Ctrl Pts',(-4.82526202566182,-3.9611060598373,69.5010774079548));
#49093=CARTESIAN_POINT('Ctrl Pts',(-5.91139473877411,-2.00721874143496,
69.4082876493781));
#49094=CARTESIAN_POINT('Ctrl Pts',(-5.92634844738098,-0.0451674678319083,
69.3154978908013));
#49095=CARTESIAN_POINT('Ctrl Pts',(-5.9264624765467,-0.0302058903593066,
69.3147903246025));
#49096=CARTESIAN_POINT('Ctrl Pts',(-5.92651421889824,-0.0152438381698188,
69.3140827584037));
#49097=CARTESIAN_POINT('Ctrl Pts',(-5.92650388951378,-0.000281712456556837,
69.3133751922048));
#49098=CARTESIAN_POINT('Ctrl Pts',(-5.92557665873441,0.00216209314576762,
69.0616248077954));
#49099=CARTESIAN_POINT('Ctrl Pts',(-5.91692824853526,-1.84261436140608,
69.1488286856693));
#49100=CARTESIAN_POINT('Ctrl Pts',(-4.98715113358366,-3.69490823008142,
69.2360325635433));
#49101=CARTESIAN_POINT('Ctrl Pts',(-3.4988016406544,-4.78352740344972,69.3232364414173));
#49102=CARTESIAN_POINT('Ctrl Pts',(-1.91480479900762,-5.94210564099642,
69.416044392633));
#49103=CARTESIAN_POINT('Ctrl Pts',(0.301863483338378,-6.23570166897768,
69.5088523438488));
#49104=CARTESIAN_POINT('Ctrl Pts',(2.13285743372907,-5.52943636436726,69.6016602950645));
#49105=CARTESIAN_POINT('Ctrl Pts',(3.96385138411946,-4.82317105975695,69.6944682462802));
#49106=CARTESIAN_POINT('Ctrl Pts',(5.4091710025548,-3.11704442255529,69.7872761974958));
#49107=CARTESIAN_POINT('Ctrl Pts',(5.80483100296866,-1.19485746730486,69.8800841487115));
#49108=CARTESIAN_POINT('Ctrl Pts',(6.20049100338259,0.727329487945907,69.9728920999272));
#49109=CARTESIAN_POINT('Ctrl Pts',(5.54649138577485,2.86557676124536,70.065700051143));
#49110=CARTESIAN_POINT('Ctrl Pts',(4.14328204209017,4.237565487387,70.1585080023588));
#49111=CARTESIAN_POINT('Ctrl Pts',(2.74007269840573,5.60955421352841,70.2513159535744));
#49112=CARTESIAN_POINT('Ctrl Pts',(0.587653628644554,6.21528439251203,70.34412390479));
#49113=CARTESIAN_POINT('Ctrl Pts',(-1.32514572522024,5.77648129462313,70.4369318560057));
#49114=CARTESIAN_POINT('Ctrl Pts',(-3.23794507908537,5.33767819673415,70.5297398072214));
#49115=CARTESIAN_POINT('Ctrl Pts',(-4.91112471705413,3.85434182197222,70.6225477584372));
#49116=CARTESIAN_POINT('Ctrl Pts',(-5.57601960034418,2.007922497702,70.715355709653));
#49117=CARTESIAN_POINT('Ctrl Pts',(-5.80591667969058,1.3694961530774,70.7474454090338));
#49118=CARTESIAN_POINT('Ctrl Pts',(-5.91527016750582,0.687662107846013,
70.7795351084146));
#49119=CARTESIAN_POINT('Ctrl Pts',(-5.91060120235062,0.00437987123653664,
70.8116248077954));
#49120=CARTESIAN_POINT('Origin',(0.,0.,-10.));
#49121=CARTESIAN_POINT('',(-5.9076390082336,-0.00209472984356585,72.8133751922048));
#49122=CARTESIAN_POINT('',(-5.9096269619093,-0.0038796998163677,72.5616248077954));
#49123=CARTESIAN_POINT('',(-5.91675,-7.2459289488551E-16,-10.));
#49124=CARTESIAN_POINT('Ctrl Pts',(-5.9076390082336,-0.00209472984356585,
72.8133751922048));
#49125=CARTESIAN_POINT('Ctrl Pts',(-5.90409465572661,1.11680292108456,72.760893194658));
#49126=CARTESIAN_POINT('Ctrl Pts',(-5.59900569561517,2.23749243052354,72.7084111971113));
#49127=CARTESIAN_POINT('Ctrl Pts',(-5.00454249156355,3.17461816130069,72.6559291995646));
#49128=CARTESIAN_POINT('Ctrl Pts',(-3.95351357183546,4.83148478947064,72.5631394409879));
#49129=CARTESIAN_POINT('Ctrl Pts',(-1.99792075551665,5.91454372612539,72.4703496824111));
#49130=CARTESIAN_POINT('Ctrl Pts',(-0.035848393374774,5.92641214501808,
72.3775599238344));
#49131=CARTESIAN_POINT('Ctrl Pts',(1.92622396876722,5.93828056391078,72.2847701652576));
#49132=CARTESIAN_POINT('Ctrl Pts',(3.89477587673228,4.87895846504129,72.1919804066808));
#49133=CARTESIAN_POINT('Ctrl Pts',(4.96577166038264,3.23492779469125,72.099190648104));
#49134=CARTESIAN_POINT('Ctrl Pts',(6.03676744403288,1.59089712434139,72.0064008895273));
#49135=CARTESIAN_POINT('Ctrl Pts',(6.21020710336862,-0.637842117488892,
71.9136111309505));
#49136=CARTESIAN_POINT('Ctrl Pts',(5.40644039496903,-2.42776610808628,71.8208213723738));
#49137=CARTESIAN_POINT('Ctrl Pts',(4.60267368656935,-4.21769009868388,71.728031613797));
#49138=CARTESIAN_POINT('Ctrl Pts',(2.82170061043407,-5.56879883804846,71.6352418552203));
#49139=CARTESIAN_POINT('Ctrl Pts',(0.881413334845232,-5.86061059558493,
71.5424520966435));
#49140=CARTESIAN_POINT('Ctrl Pts',(-1.05887394074338,-6.15242235312137,
71.4496623380668));
#49141=CARTESIAN_POINT('Ctrl Pts',(-3.15847541578552,-5.38493712882995,
71.35687257949));
#49142=CARTESIAN_POINT('Ctrl Pts',(-4.45317235729702,-3.91061401523227,
71.2640828209133));
#49143=CARTESIAN_POINT('Ctrl Pts',(-5.38666457674259,-2.84760914408037,
71.1971802780104));
#49144=CARTESIAN_POINT('Ctrl Pts',(-5.90172032162132,-1.41714857828327,
71.1302777351076));
#49145=CARTESIAN_POINT('Ctrl Pts',(-5.91402970906047,0.00531590772330143,
71.0633751922048));
#49146=CARTESIAN_POINT('Ctrl Pts',(-5.91060120235062,0.00437987123653664,
70.8116248077954));
#49147=CARTESIAN_POINT('Ctrl Pts',(-5.90176685963095,-1.28848680303269,
70.8723430596303));
#49148=CARTESIAN_POINT('Ctrl Pts',(-5.48470939396936,-2.58653829127134,
70.9330613114652));
#49149=CARTESIAN_POINT('Ctrl Pts',(-4.70360458874419,-3.6055306423528,70.9937795633001));
#49150=CARTESIAN_POINT('Ctrl Pts',(-3.50968456524259,-5.16306218435938,
71.0865875145158));
#49151=CARTESIAN_POINT('Ctrl Pts',(-1.46523438962779,-6.06862299459407,
71.1793954657315));
#49152=CARTESIAN_POINT('Ctrl Pts',(0.490517813476914,-5.90619502004989,
71.2722034169472));
#49153=CARTESIAN_POINT('Ctrl Pts',(2.44627001658162,-5.74376704550572,71.3650113681629));
#49154=CARTESIAN_POINT('Ctrl Pts',(4.31332424717623,-4.51335028618269,71.4578193193786));
#49155=CARTESIAN_POINT('Ctrl Pts',(5.23394874711508,-2.78020284381785,71.5506272705943));
#49156=CARTESIAN_POINT('Ctrl Pts',(6.15457324705387,-1.04705540145311,71.64343522181));
#49157=CARTESIAN_POINT('Ctrl Pts',(6.12876801633701,1.18882272395339,71.7362431730258));
#49158=CARTESIAN_POINT('Ctrl Pts',(5.16838807532191,2.90026068536445,71.8290511242415));
#49159=CARTESIAN_POINT('Ctrl Pts',(4.20800813430676,4.61169864677561,71.9218590754572));
#49160=CARTESIAN_POINT('Ctrl Pts',(2.31305348299327,5.79869644419127,72.0146670266729));
#49161=CARTESIAN_POINT('Ctrl Pts',(0.354073438076874,5.91594281079937,72.1074749778886));
#49162=CARTESIAN_POINT('Ctrl Pts',(-1.60490660683963,6.03318917740748,72.2002829291043));
#49163=CARTESIAN_POINT('Ctrl Pts',(-3.62791204535904,5.0806841132079,72.29309088032));
#49164=CARTESIAN_POINT('Ctrl Pts',(-4.78556654599306,3.49601203860518,72.3858988315358));
#49165=CARTESIAN_POINT('Ctrl Pts',(-5.51621503257378,2.49585331041722,72.4444741569556));
#49166=CARTESIAN_POINT('Ctrl Pts',(-5.90215555477039,1.24387420073254,72.5030494823755));
#49167=CARTESIAN_POINT('Ctrl Pts',(-5.9096269619093,-0.0038796998163677,
72.5616248077954));
#49168=CARTESIAN_POINT('Origin',(0.,0.,-10.));
#49169=CARTESIAN_POINT('',(-5.92173242987796,-0.00453640779018327,74.5633751922048));
#49170=CARTESIAN_POINT('',(-5.92478692091682,-0.00290426967806841,74.3116248077954));
#49171=CARTESIAN_POINT('',(-5.91675,-7.2459289488551E-16,-10.));
#49172=CARTESIAN_POINT('Ctrl Pts',(-5.92173242987796,-0.00453640779018327,
74.5633751922048));
#49173=CARTESIAN_POINT('Ctrl Pts',(-5.90751771867388,1.67116708836971,74.4842984127853));
#49174=CARTESIAN_POINT('Ctrl Pts',(-5.1617797014763,3.35793373378459,74.4052216333658));
#49175=CARTESIAN_POINT('Ctrl Pts',(-3.90360669034165,4.4593161837938,74.3261448539462));
#49176=CARTESIAN_POINT('Ctrl Pts',(-2.42724952445859,5.75169319240769,74.2333550953694));
#49177=CARTESIAN_POINT('Ctrl Pts',(-0.245321033219509,6.23805517964,74.1405653367927));
#49178=CARTESIAN_POINT('Ctrl Pts',(1.64015227963515,5.69504578730786,74.0477755782159));
#49179=CARTESIAN_POINT('Ctrl Pts',(3.5256255924898,5.15203639497571,73.9549858196392));
#49180=CARTESIAN_POINT('Ctrl Pts',(5.11464372696003,3.5796556230791,73.8621960610624));
#49181=CARTESIAN_POINT('Ctrl Pts',(5.67746769661407,1.70000193347804,73.7694063024857));
#49182=CARTESIAN_POINT('Ctrl Pts',(6.24029166626812,-0.179651756123031,
73.6766165439089));
#49183=CARTESIAN_POINT('Ctrl Pts',(5.77692147110597,-2.36657836342856,73.5838267853321));
#49184=CARTESIAN_POINT('Ctrl Pts',(4.50015474334161,-3.85645605522809,73.4910370267554));
#49185=CARTESIAN_POINT('Ctrl Pts',(3.22338801557717,-5.34633374702771,73.3982472681786));
#49186=CARTESIAN_POINT('Ctrl Pts',(1.13322475521041,-6.13916252332125,73.3054575096019));
#49187=CARTESIAN_POINT('Ctrl Pts',(-0.810450700374689,-5.87084454590543,
73.2126677510251));
#49188=CARTESIAN_POINT('Ctrl Pts',(-2.75412615595968,-5.60252656848963,
73.1198779924484));
#49189=CARTESIAN_POINT('Ctrl Pts',(-4.55131380676303,-4.27306183736458,
73.0270882338716));
#49190=CARTESIAN_POINT('Ctrl Pts',(-5.37667512059602,-2.49299231195949,
72.9342984752948));
#49191=CARTESIAN_POINT('Ctrl Pts',(-5.7352110960279,-1.71973222218887,72.8939907142648));
#49192=CARTESIAN_POINT('Ctrl Pts',(-5.91036117813064,-0.86144195820518,
72.8536829532348));
#49193=CARTESIAN_POINT('Ctrl Pts',(-5.9076390082336,-0.00209472984356585,
72.8133751922048));
#49194=CARTESIAN_POINT('Ctrl Pts',(-5.9096269619093,-0.0038796998163677,
72.5616248077954));
#49195=CARTESIAN_POINT('Ctrl Pts',(-5.91399340602072,-0.733092761060087,
72.5958574335912));
#49196=CARTESIAN_POINT('Ctrl Pts',(-5.78909470142213,-1.46086271303664,
72.630090059387));
#49197=CARTESIAN_POINT('Ctrl Pts',(-5.52819187461763,-2.13608097637051,
72.6643226851828));
#49198=CARTESIAN_POINT('Ctrl Pts',(-4.82085913985954,-3.96666283173856,
72.7571306363985));
#49199=CARTESIAN_POINT('Ctrl Pts',(-3.11389010759454,-5.41098745746912,
72.8499385876142));
#49200=CARTESIAN_POINT('Ctrl Pts',(-1.19147279183569,-5.80552667089866,
72.9427465388299));
#49201=CARTESIAN_POINT('Ctrl Pts',(0.730944523923385,-6.20006588432824,
73.0355544900457));
#49202=CARTESIAN_POINT('Ctrl Pts',(2.86881012317626,-5.54481968545648,73.1283624412614));
#49203=CARTESIAN_POINT('Ctrl Pts',(4.23998048321321,-4.14081065036442,73.2211703924771));
#49204=CARTESIAN_POINT('Ctrl Pts',(5.61115084325,-2.73680161527252,73.3139783436929));
#49205=CARTESIAN_POINT('Ctrl Pts',(6.21562596407094,-0.584029743960555,
73.4067862949085));
#49206=CARTESIAN_POINT('Ctrl Pts',(5.77570769441674,1.32851344323482,73.4995942461242));
#49207=CARTESIAN_POINT('Ctrl Pts',(5.33578942476254,3.2410566304302,73.5924021973399));
#49208=CARTESIAN_POINT('Ctrl Pts',(3.85147776463294,4.9133711335092,73.6852101485556));
#49209=CARTESIAN_POINT('Ctrl Pts',(2.00467109117049,5.57718935992186,73.7780180997714));
#49210=CARTESIAN_POINT('Ctrl Pts',(0.157864417707936,6.24100758633457,73.8708260509871));
#49211=CARTESIAN_POINT('Ctrl Pts',(-2.05143726908759,5.8963295360811,73.9636340022028));
#49212=CARTESIAN_POINT('Ctrl Pts',(-3.60827243835276,4.70150160595785,74.0564419534185));
#49213=CARTESIAN_POINT('Ctrl Pts',(-5.03515320694838,3.6064100837908,74.1415029048774));
#49214=CARTESIAN_POINT('Ctrl Pts',(-5.91394845174191,1.79717487807919,74.2265638563364));
#49215=CARTESIAN_POINT('Ctrl Pts',(-5.92478692091682,-0.00290426967806841,
74.3116248077954));
#49216=CARTESIAN_POINT('Origin',(0.,0.,-10.));
#49217=CARTESIAN_POINT('',(-5.92221425476728,0.00435283123465607,76.3133751922048));
#49218=CARTESIAN_POINT('',(-5.91860112252369,0.00530505955111227,76.0616248077954));
#49219=CARTESIAN_POINT('',(-5.91675,-7.2459289488551E-16,-10.));
#49220=CARTESIAN_POINT('Ctrl Pts',(-5.92221425476728,0.00435283123465607,
76.3133751922048));
#49221=CARTESIAN_POINT('Ctrl Pts',(-5.92446422127454,0.277271243771341,
76.3004933894893));
#49222=CARTESIAN_POINT('Ctrl Pts',(-5.90723714835,0.549904061635848,76.2876115867737));
#49223=CARTESIAN_POINT('Ctrl Pts',(-5.86956287631793,0.819681438655091,
76.2747297840581));
#49224=CARTESIAN_POINT('Ctrl Pts',(-5.59818885487094,2.76293256862564,76.1819400254814));
#49225=CARTESIAN_POINT('Ctrl Pts',(-4.26589973965931,4.55802745107444,76.0891502669046));
#49226=CARTESIAN_POINT('Ctrl Pts',(-2.48453455723552,5.3805886345109,75.9963605083278));
#49227=CARTESIAN_POINT('Ctrl Pts',(-0.703169374811634,6.20314981794741,
75.903570749751));
#49228=CARTESIAN_POINT('Ctrl Pts',(1.52727187482435,6.05317730237141,75.8107809911743));
#49229=CARTESIAN_POINT('Ctrl Pts',(3.18248374071698,4.99954430523397,75.7179912325975));
#49230=CARTESIAN_POINT('Ctrl Pts',(4.83769560660942,3.94591130809665,75.6252014740208));
#49231=CARTESIAN_POINT('Ctrl Pts',(5.91767808875851,1.98861782939818,75.532411715444));
#49232=CARTESIAN_POINT('Ctrl Pts',(5.92646118859023,0.0265292302760358,
75.4396219568673));
#49233=CARTESIAN_POINT('Ctrl Pts',(5.93524428842194,-1.93555936884622,75.3468321982905));
#49234=CARTESIAN_POINT('Ctrl Pts',(4.87282800593588,-3.90244308839225,75.2540424397138));
#49235=CARTESIAN_POINT('Ctrl Pts',(3.22711525698444,-4.97085235528712,75.161252681137));
#49236=CARTESIAN_POINT('Ctrl Pts',(1.58140250803301,-6.039261622182,75.0684629225603));
#49237=CARTESIAN_POINT('Ctrl Pts',(-0.647606707383809,-6.20919643642597,
74.9756731639835));
#49238=CARTESIAN_POINT('Ctrl Pts',(-2.43626458417193,-5.40261611590486,
74.8828834054067));
#49239=CARTESIAN_POINT('Ctrl Pts',(-4.22492246096005,-4.59603579538375,
74.79009364683));
#49240=CARTESIAN_POINT('Ctrl Pts',(-5.57322899911938,-2.8129403400976,74.6973038882532));
#49241=CARTESIAN_POINT('Ctrl Pts',(-5.86198934793559,-0.872196597456742,
74.6045141296765));
#49242=CARTESIAN_POINT('Ctrl Pts',(-5.90466393514745,-0.585382848821439,
74.5908011505193));
#49243=CARTESIAN_POINT('Ctrl Pts',(-5.9241974523523,-0.295125975109717,
74.577088171362));
#49244=CARTESIAN_POINT('Ctrl Pts',(-5.92173242987796,-0.00453640779018327,
74.5633751922048));
#49245=CARTESIAN_POINT('Ctrl Pts',(-5.92478692091682,-0.00290426967806841,
74.3116248077954));
#49246=CARTESIAN_POINT('Ctrl Pts',(-5.92577404387537,-0.166848035655527,
74.3193718075521));
#49247=CARTESIAN_POINT('Ctrl Pts',(-5.91956162748079,-0.330715853842254,
74.3271188073088));
#49248=CARTESIAN_POINT('Ctrl Pts',(-5.90590802266303,-0.493961302173379,
74.3348658070656));
#49249=CARTESIAN_POINT('Ctrl Pts',(-5.74233978597349,-2.44961847018869,
74.4276737582813));
#49250=CARTESIAN_POINT('Ctrl Pts',(-4.51083466085957,-4.3159549962264,74.5204817094971));
#49251=CARTESIAN_POINT('Ctrl Pts',(-2.77715074840922,-5.2355688383222,74.6132896607128));
#49252=CARTESIAN_POINT('Ctrl Pts',(-1.04346683595887,-6.155182680418,74.7060976119285));
#49253=CARTESIAN_POINT('Ctrl Pts',(1.19239586382801,-6.12807383857193,74.7989055631442));
#49254=CARTESIAN_POINT('Ctrl Pts',(2.90327359050187,-5.16669621701284,74.8917135143599));
#49255=CARTESIAN_POINT('Ctrl Pts',(4.61415131717573,-4.20531859545374,74.9845214655756));
#49256=CARTESIAN_POINT('Ctrl Pts',(5.80004407073672,-2.30967219418159,75.0773294167913));
#49257=CARTESIAN_POINT('Ctrl Pts',(5.91614824568895,-0.350624122432983,
75.170137368007));
#49258=CARTESIAN_POINT('Ctrl Pts',(6.03225242064119,1.60842394931563,75.2629453192228));
#49259=CARTESIAN_POINT('Ctrl Pts',(5.07856801698493,3.63087369154057,75.3557532704385));
#49260=CARTESIAN_POINT('Ctrl Pts',(3.49322124812066,4.78760406172844,75.4485612216541));
#49261=CARTESIAN_POINT('Ctrl Pts',(1.90787447925649,5.94433443191625,75.5413691728698));
#49262=CARTESIAN_POINT('Ctrl Pts',(-0.30913465481563,6.23534543006683,75.6341771240855));
#49263=CARTESIAN_POINT('Ctrl Pts',(-2.13930379287229,5.52694550561181,75.7269850753013));
#49264=CARTESIAN_POINT('Ctrl Pts',(-3.96947293092905,4.81854558115675,75.819793026517));
#49265=CARTESIAN_POINT('Ctrl Pts',(-5.4128020729704,3.11073473409595,75.9126009777328));
#49266=CARTESIAN_POINT('Ctrl Pts',(-5.80622036529553,1.18808771133609,76.0054089289485));
#49267=CARTESIAN_POINT('Ctrl Pts',(-5.88565448980684,0.799890756653038,
76.0241475552308));
#49268=CARTESIAN_POINT('Ctrl Pts',(-5.92228725593392,0.402935648692027,
76.0428861815131));
#49269=CARTESIAN_POINT('Ctrl Pts',(-5.91860112252369,0.00530505955111227,
76.0616248077954));
#49270=CARTESIAN_POINT('Origin',(0.,0.,-10.));
#49271=CARTESIAN_POINT('',(-5.90783837446273,0.00236323016111234,78.0633751922048));
#49272=CARTESIAN_POINT('',(-5.9069646967222,0.000416249466083529,77.8116248077954));
#49273=CARTESIAN_POINT('',(-5.91675,-7.2459289488551E-16,-10.));
#49274=CARTESIAN_POINT('Ctrl Pts',(-5.90783837446273,0.00236323016111234,
78.0633751922048));
#49275=CARTESIAN_POINT('Ctrl Pts',(-5.91085192024158,0.843919154698636,
78.0238986076164));
#49276=CARTESIAN_POINT('Ctrl Pts',(-5.74312714104647,1.68432885304078,77.9844220230281));
#49277=CARTESIAN_POINT('Ctrl Pts',(-5.39877847795077,2.44475703617782,77.9449454384397));
#49278=CARTESIAN_POINT('Ctrl Pts',(-4.5893865397156,4.23214437639491,77.8521556798629));
#49279=CARTESIAN_POINT('Ctrl Pts',(-2.80417311428585,5.57764537943121,77.7593659212861));
#49280=CARTESIAN_POINT('Ctrl Pts',(-0.862977703412722,5.86335360551774,
77.6665761627094));
#49281=CARTESIAN_POINT('Ctrl Pts',(1.07821770746029,6.14906183160425,77.5737864041326));
#49282=CARTESIAN_POINT('Ctrl Pts',(3.17539510377643,5.37497728074138,77.480996645556));
#49283=CARTESIAN_POINT('Ctrl Pts',(4.4654489838702,3.89658971311811,77.3882068869792));
#49284=CARTESIAN_POINT('Ctrl Pts',(5.7555028639639,2.41820214549493,77.2954171284024));
#49285=CARTESIAN_POINT('Ctrl Pts',(6.23843322783498,0.235511561111468,77.2026273698256));
#49286=CARTESIAN_POINT('Ctrl Pts',(5.69245965233818,-1.64910555345231,77.1098376112489));
#49287=CARTESIAN_POINT('Ctrl Pts',(5.14648607684132,-3.5337226680163,77.0170478526721));
#49288=CARTESIAN_POINT('Ctrl Pts',(3.57160856197623,-5.12026631276067,76.9242580940954));
#49289=CARTESIAN_POINT('Ctrl Pts',(1.69107217117025,-5.68013388326533,76.8314683355187));
#49290=CARTESIAN_POINT('Ctrl Pts',(-0.189464219635722,-6.24000145377,76.7386785769419));
#49291=CARTESIAN_POINT('Ctrl Pts',(-2.37565948638272,-5.77319295003497,
76.6458888183651));
#49292=CARTESIAN_POINT('Ctrl Pts',(-3.86352765591502,-4.49408500942128,
76.5530990597883));
#49293=CARTESIAN_POINT('Ctrl Pts',(-5.14483828590118,-3.39255287453919,
76.4731911039271));
#49294=CARTESIAN_POINT('Ctrl Pts',(-5.9082573398602,-1.68860528528188,76.393283148066));
#49295=CARTESIAN_POINT('Ctrl Pts',(-5.92221425476728,0.00435283123465607,
76.3133751922048));
#49296=CARTESIAN_POINT('Ctrl Pts',(-5.91860112252369,0.00530505955111227,
76.0616248077954));
#49297=CARTESIAN_POINT('Ctrl Pts',(-5.90403071542999,-1.5664339178317,76.1356941327288));
#49298=CARTESIAN_POINT('Ctrl Pts',(-5.25950470490065,-3.14872683292577,
76.2097634576621));
#49299=CARTESIAN_POINT('Ctrl Pts',(-4.13833785100994,-4.24239403769839,
76.2838327825955));
#49300=CARTESIAN_POINT('Ctrl Pts',(-2.73352960179007,-5.61274556551441,
76.3766407338112));
#49301=CARTESIAN_POINT('Ctrl Pts',(-0.580405660741316,-6.21596542268728,
76.469448685027));
#49302=CARTESIAN_POINT('Ctrl Pts',(1.33188070963397,-5.77493213081377,76.5622566362427));
#49303=CARTESIAN_POINT('Ctrl Pts',(3.24416708000904,-5.33389883894032,76.6550645874584));
#49304=CARTESIAN_POINT('Ctrl Pts',(4.91561587971071,-3.84861239802078,76.7478725386741));
#49305=CARTESIAN_POINT('Ctrl Pts',(5.57835722358738,-2.00141900317022,76.8406804898898));
#49306=CARTESIAN_POINT('Ctrl Pts',(6.24109856746405,-0.154225608319656,
76.9334884411055));
#49307=CARTESIAN_POINT('Ctrl Pts',(5.89513245551572,2.05487474046193,77.0262963923212));
#49308=CARTESIAN_POINT('Ctrl Pts',(4.69939702494141,3.61101300775449,77.1191043435369));
#49309=CARTESIAN_POINT('Ctrl Pts',(3.50366159436703,5.16715127504713,77.2119122947526));
#49310=CARTESIAN_POINT('Ctrl Pts',(1.45815684516657,6.07032746085066,77.3047202459683));
#49311=CARTESIAN_POINT('Ctrl Pts',(-0.49740462295242,5.90561901761923,77.397528197184));
#49312=CARTESIAN_POINT('Ctrl Pts',(-2.45296609107141,5.7409105743878,77.4903361483998));
#49313=CARTESIAN_POINT('Ctrl Pts',(-4.31858427810893,4.5083175021214,77.5831440996155));
#49314=CARTESIAN_POINT('Ctrl Pts',(-5.23718714974778,2.77409770893476,77.6759520508312));
#49315=CARTESIAN_POINT('Ctrl Pts',(-5.68481181450939,1.92903225408464,77.7211763031526));
#49316=CARTESIAN_POINT('Ctrl Pts',(-5.90756756517641,0.964855466841043,
77.766400555474));
#49317=CARTESIAN_POINT('Ctrl Pts',(-5.9069646967222,0.000416249466083529,
77.8116248077954));
#49318=CARTESIAN_POINT('Origin',(0.,0.,-10.));
#49319=CARTESIAN_POINT('',(-5.91352838726915,-0.0052379771925426,79.8133751922048));
#49320=CARTESIAN_POINT('',(-5.91706824557423,-0.00544986776190025,79.5616248077954));
#49321=CARTESIAN_POINT('',(-5.91675,-7.2459289488551E-16,-10.));
#49322=CARTESIAN_POINT('Ctrl Pts',(-5.91352838726915,-0.0052379771925426,
79.8133751922048));
#49323=CARTESIAN_POINT('Ctrl Pts',(-5.90162685186426,1.39985609417491,79.7473038257436));
#49324=CARTESIAN_POINT('Ctrl Pts',(-5.40046356538693,2.81257996585592,79.6812324592824));
#49325=CARTESIAN_POINT('Ctrl Pts',(-4.4880041631094,3.87058970337054,79.6151610928213));
#49326=CARTESIAN_POINT('Ctrl Pts',(-3.20655817245923,5.35644467162761,79.5223713342445));
#49327=CARTESIAN_POINT('Ctrl Pts',(-1.11391184920308,6.14269608769454,79.4295815756678));
#49328=CARTESIAN_POINT('Ctrl Pts',(0.828910150132987,5.86826669323505,79.3367918170911));
#49329=CARTESIAN_POINT('Ctrl Pts',(2.77173214946938,5.59383729877552,79.2440020585143));
#49330=CARTESIAN_POINT('Ctrl Pts',(4.56472982488564,4.25872709378915,79.1512122999375));
#49331=CARTESIAN_POINT('Ctrl Pts',(5.38448884400271,2.47607065907574,79.0584225413607));
#49332=CARTESIAN_POINT('Ctrl Pts',(6.20424786311968,0.693414224362538,78.965632782784));
#49333=CARTESIAN_POINT('Ctrl Pts',(6.05076822593769,-1.53678844007761,78.8728430242073));
#49334=CARTESIAN_POINT('Ctrl Pts',(4.99453375667845,-3.19034145089906,78.7800532656305));
#49335=CARTESIAN_POINT('Ctrl Pts',(3.93829928741921,-4.84389446172052,78.6872635070538));
#49336=CARTESIAN_POINT('Ctrl Pts',(1.97930998608272,-5.92079781892327,78.594473748477));
#49337=CARTESIAN_POINT('Ctrl Pts',(0.017210001578922,-5.92649557797616,
78.5016839899002));
#49338=CARTESIAN_POINT('Ctrl Pts',(-1.94488998292488,-5.93219333702905,
78.4088942313235));
#49339=CARTESIAN_POINT('Ctrl Pts',(-3.91010065059599,-4.86668549793206,
78.3161044727467));
#49340=CARTESIAN_POINT('Ctrl Pts',(-4.97592075891125,-3.21929473968469,
78.22331471417));
#49341=CARTESIAN_POINT('Ctrl Pts',(-5.58829710029315,-2.272771853232,78.1700015401816));
#49342=CARTESIAN_POINT('Ctrl Pts',(-5.90376857733856,-1.13415903724546,
78.1166883661932));
#49343=CARTESIAN_POINT('Ctrl Pts',(-5.90783837446273,0.00236323016111234,
78.0633751922048));
#49344=CARTESIAN_POINT('Ctrl Pts',(-5.9069646967222,0.000416249466083529,
77.8116248077954));
#49345=CARTESIAN_POINT('Ctrl Pts',(-5.90633037532328,-1.01433983749622,
77.8592085066897));
#49346=CARTESIAN_POINT('Ctrl Pts',(-5.65842326778303,-2.0293864519967,77.906792205584));
#49347=CARTESIAN_POINT('Ctrl Pts',(-5.16500260233514,-2.90628550869862,
77.9543759044783));
#49348=CARTESIAN_POINT('Ctrl Pts',(-4.20262762704341,-4.61660241903885,
78.047183855694));
#49349=CARTESIAN_POINT('Ctrl Pts',(-2.3062901202197,-5.80138972561238,78.1399918069097));
#49350=CARTESIAN_POINT('Ctrl Pts',(-0.347174687598445,-5.91635166944049,
78.2327997581254));
#49351=CARTESIAN_POINT('Ctrl Pts',(1.6119407450227,-6.03131361326859,78.3256077093412));
#49352=CARTESIAN_POINT('Ctrl Pts',(3.63383410344128,-5.07645019435141,78.4184156605569));
#49353=CARTESIAN_POINT('Ctrl Pts',(4.78963994996363,-3.49042927014899,78.5112236117726));
#49354=CARTESIAN_POINT('Ctrl Pts',(5.94544579648597,-1.90440834594658,78.6040315629883));
#49355=CARTESIAN_POINT('Ctrl Pts',(6.23516413111195,0.312770083541336,78.696839514204));
#49356=CARTESIAN_POINT('Ctrl Pts',(5.52569725777374,2.1425258821382,78.7896474654197));
#49357=CARTESIAN_POINT('Ctrl Pts',(4.8162303844355,3.97228168073516,78.8824554166354));
#49358=CARTESIAN_POINT('Ctrl Pts',(3.10757830313311,5.41461484844123,78.9752633678512));
#49359=CARTESIAN_POINT('Ctrl Pts',(1.18470222695776,5.80691208592327,79.0680713190669));
#49360=CARTESIAN_POINT('Ctrl Pts',(-0.738173849217586,6.1992093234053,79.1608792702826));
#49361=CARTESIAN_POINT('Ctrl Pts',(-2.87527392026577,5.54147063066327,79.2536872214982));
#49362=CARTESIAN_POINT('Ctrl Pts',(-4.24480615002276,4.13586364486661,79.346495172714));
#49363=CARTESIAN_POINT('Ctrl Pts',(-5.30300200846101,3.04979392073473,79.4182050510744));
#49364=CARTESIAN_POINT('Ctrl Pts',(-5.90294586434624,1.51723318368911,79.4899149294349));
#49365=CARTESIAN_POINT('Ctrl Pts',(-5.91706824557423,-0.00544986776190025,
79.5616248077954));
#49366=CARTESIAN_POINT('Origin',(0.,0.,-10.));
#49367=CARTESIAN_POINT('',(-5.92652005161158,-4.92410581365288E-5,81.5633751922047));
#49368=CARTESIAN_POINT('',(-5.92564501137359,0.00208360169631917,81.3116248077953));
#49369=CARTESIAN_POINT('',(-5.91675,-7.2459289488551E-16,-10.));
#49370=CARTESIAN_POINT('Ctrl Pts',(-5.92652005161158,-4.92410581365288E-5,
81.5633751922047));
#49371=CARTESIAN_POINT('Ctrl Pts',(-5.9262796163795,1.95944564602974,81.4707090438708));
#49372=CARTESIAN_POINT('Ctrl Pts',(-4.85833414818282,3.91916492820066,81.378042895537));
#49373=CARTESIAN_POINT('Ctrl Pts',(-3.21146626212954,4.9809768587225,81.285376747203));
#49374=CARTESIAN_POINT('Ctrl Pts',(-1.56240156804075,6.04420517303622,81.1925869886263));
#49375=CARTESIAN_POINT('Ctrl Pts',(0.667131059078623,6.20712904518559,81.0997972300494));
#49376=CARTESIAN_POINT('Ctrl Pts',(2.45324344310461,5.39492749059611,81.0070074714726));
#49377=CARTESIAN_POINT('Ctrl Pts',(4.2393558271304,4.58272593600671,80.9142177128958));
#49378=CARTESIAN_POINT('Ctrl Pts',(5.58204796806278,2.79539895467876,80.8214279543191));
#49379=CARTESIAN_POINT('Ctrl Pts',(5.86470336495774,0.853756675510454,80.7286381957424));
#49380=CARTESIAN_POINT('Ctrl Pts',(6.14735876185272,-1.08788560365796,80.6358484371657));
#49381=CARTESIAN_POINT('Ctrl Pts',(5.3699774147099,-3.1838431806669,80.5430586785889));
#49382=CARTESIAN_POINT('Ctrl Pts',(3.88956310091184,-4.47157074236229,80.4502689200121));
#49383=CARTESIAN_POINT('Ctrl Pts',(2.40914878711369,-5.75929830405776,80.3574791614354));
#49384=CARTESIAN_POINT('Ctrl Pts',(0.225701506660258,-6.23879585043983,
80.2646894028585));
#49385=CARTESIAN_POINT('Ctrl Pts',(-1.65805474957566,-5.68985944179072,
80.1718996442818));
#49386=CARTESIAN_POINT('Ctrl Pts',(-3.54181100581147,-5.14092303314164,
80.079109885705));
#49387=CARTESIAN_POINT('Ctrl Pts',(-5.12587623782969,-3.56355266946152,
79.9863201271284));
#49388=CARTESIAN_POINT('Ctrl Pts',(-5.68278602481674,-1.68213822739774,
79.8935303685516));
#49389=CARTESIAN_POINT('Ctrl Pts',(-5.84314568400726,-1.14039343178604,
79.866811976436));
#49390=CARTESIAN_POINT('Ctrl Pts',(-5.91834121174604,-0.573439550262532,
79.8400935843204));
#49391=CARTESIAN_POINT('Ctrl Pts',(-5.91352838726915,-0.0052379771925426,
79.8133751922048));
#49392=CARTESIAN_POINT('Ctrl Pts',(-5.91706824557423,-0.00544986776190025,
79.5616248077954));
#49393=CARTESIAN_POINT('Ctrl Pts',(-5.92122325231597,-0.453445021141946,
79.5827228806506));
#49394=CARTESIAN_POINT('Ctrl Pts',(-5.87466834302196,-0.900585141668491,
79.6038209535059));
#49395=CARTESIAN_POINT('Ctrl Pts',(-5.77415460407802,-1.33524752327236,
79.6249190263611));
#49396=CARTESIAN_POINT('Ctrl Pts',(-5.33200643991055,-3.2472764267639,79.7177269775768));
#49397=CARTESIAN_POINT('Ctrl Pts',(-3.84574572310957,-4.91785895489578,
79.8105349287925));
#49398=CARTESIAN_POINT('Ctrl Pts',(-1.99816623480639,-5.57952319094383,
79.9033428800082));
#49399=CARTESIAN_POINT('Ctrl Pts',(-0.150586746503413,-6.24118742699181,
79.9961508312239));
#49400=CARTESIAN_POINT('Ctrl Pts',(2.05831151330152,-5.89393337095641,80.0889587824397));
#49401=CARTESIAN_POINT('Ctrl Pts',(3.61375234962716,-4.69729084640972,80.1817667336554));
#49402=CARTESIAN_POINT('Ctrl Pts',(5.16919318595289,-3.50064832186295,80.2745746848711));
#49403=CARTESIAN_POINT('Ctrl Pts',(6.07117659879901,-1.4546173288047,80.3673826360867));
#49404=CARTESIAN_POINT('Ctrl Pts',(5.90532800501674,0.500847774643518,80.4601905873024));
#49405=CARTESIAN_POINT('Ctrl Pts',(5.73947941123448,2.45631287809162,80.5529985385181));
#49406=CARTESIAN_POINT('Ctrl Pts',(4.50579881082393,4.32121209192987,80.6458064897339));
#49407=CARTESIAN_POINT('Ctrl Pts',(2.77104372643263,5.23880368084153,80.7386144409496));
#49408=CARTESIAN_POINT('Ctrl Pts',(1.03628864204112,6.15639526975329,80.8314223921654));
#49409=CARTESIAN_POINT('Ctrl Pts',(-1.19954092633104,6.12667923373836,80.924230343381));
#49410=CARTESIAN_POINT('Ctrl Pts',(-2.90929643893171,5.16330723186405,81.0170382945967));
#49411=CARTESIAN_POINT('Ctrl Pts',(-4.61905195153228,4.1999352299898,81.1098462458124));
#49412=CARTESIAN_POINT('Ctrl Pts',(-5.80273340836125,2.30290726225611,81.2026541970281));
#49413=CARTESIAN_POINT('Ctrl Pts',(-5.9165530819849,0.343725134744857,81.2954621482438));
#49414=CARTESIAN_POINT('Ctrl Pts',(-5.92316037734029,0.229993522631114,
81.3008497014276));
#49415=CARTESIAN_POINT('Ctrl Pts',(-5.92616238070294,0.116052459261064,
81.3062372546115));
#49416=CARTESIAN_POINT('Ctrl Pts',(-5.92564501137359,0.00208360169631917,
81.3116248077953));
#49417=CARTESIAN_POINT('Origin',(0.,0.,-10.));
#49418=CARTESIAN_POINT('',(-5.91367641053724,0.00526281327289491,83.3133751922047));
#49419=CARTESIAN_POINT('',(-5.91070653272951,0.00442589000008243,83.0616248077953));
#49420=CARTESIAN_POINT('',(-5.91675,-7.2459289488551E-16,-10.));
#49421=CARTESIAN_POINT('Ctrl Pts',(-5.91367641053724,0.00526281327289491,
83.3133751922047));
#49422=CARTESIAN_POINT('Ctrl Pts',(-5.91847631819128,0.568171225327802,
83.2869040205747));
#49423=CARTESIAN_POINT('Ctrl Pts',(-5.84469124069181,1.12984655758661,83.2604328489447));
#49424=CARTESIAN_POINT('Ctrl Pts',(-5.6872451620954,1.66699984587517,83.2339616773148));
#49425=CARTESIAN_POINT('Ctrl Pts',(-5.13534727763322,3.54989058587421,83.141171918738));
#49426=CARTESIAN_POINT('Ctrl Pts',(-3.55548796545528,5.13147348829515,83.0483821601613));
#49427=CARTESIAN_POINT('Ctrl Pts',(-1.67320012425186,5.68542411471026,82.9555924015846));
#49428=CARTESIAN_POINT('Ctrl Pts',(0.209087716951782,6.23937474112543,82.8628026430078));
#49429=CARTESIAN_POINT('Ctrl Pts',(2.39380408718108,5.76569309153457,82.770012884431));
#49430=CARTESIAN_POINT('Ctrl Pts',(3.87764218013329,4.48191221944122,82.6772231258543));
#49431=CARTESIAN_POINT('Ctrl Pts',(5.36148027308533,3.19813134734802,82.5844333672775));
#49432=CARTESIAN_POINT('Ctrl Pts',(6.1444400887605,1.10425125275282,82.4916436087007));
#49433=CARTESIAN_POINT('Ctrl Pts',(5.86695599986163,-0.838136811990138,
82.398853850124));
#49434=CARTESIAN_POINT('Ctrl Pts',(5.58947191096278,-2.78052487673298,82.3060640915472));
#49435=CARTESIAN_POINT('Ctrl Pts',(4.25154391748981,-4.57142091162344,82.2132743329705));
#49436=CARTESIAN_POINT('Ctrl Pts',(2.4676006384095,-5.38837573942708,82.1204845743937));
#49437=CARTESIAN_POINT('Ctrl Pts',(0.683657359328989,-6.20533056723082,
82.027694815817));
#49438=CARTESIAN_POINT('Ctrl Pts',(-1.54630120535912,-6.04834418794753,
81.9349050572403));
#49439=CARTESIAN_POINT('Ctrl Pts',(-3.19819127241771,-4.98951085828627,
81.8421152986635));
#49440=CARTESIAN_POINT('Ctrl Pts',(-4.85228191134336,-3.92926699962938,
81.7492019298439));
#49441=CARTESIAN_POINT('Ctrl Pts',(-5.92676112829165,-1.96477178987861,
81.6562885610243));
#49442=CARTESIAN_POINT('Ctrl Pts',(-5.92652005161158,-4.92410581365288E-5,
81.5633751922047));
#49443=CARTESIAN_POINT('Ctrl Pts',(-5.92564501137359,0.00208360169631917,
81.3116248077953));
#49444=CARTESIAN_POINT('Ctrl Pts',(-5.91724998840898,-1.8472165447024,81.3990452058272));
#49445=CARTESIAN_POINT('Ctrl Pts',(-4.9822221455073,-3.70383476033302,81.4864656038591));
#49446=CARTESIAN_POINT('Ctrl Pts',(-3.48763610563928,-4.79167421000652,
81.573886001891));
#49447=CARTESIAN_POINT('Ctrl Pts',(-1.9009415652512,-5.94655513995829,81.6666939531067));
#49448=CARTESIAN_POINT('Ctrl Pts',(0.316405405943797,-6.23498071257269,
81.7595019043224));
#49449=CARTESIAN_POINT('Ctrl Pts',(2.14574724307293,-5.52444713152776,81.8523098555381));
#49450=CARTESIAN_POINT('Ctrl Pts',(3.97508908020207,-4.81391355048283,81.9451178067538));
#49451=CARTESIAN_POINT('Ctrl Pts',(5.41642578326554,-3.10442081577871,82.0379257579695));
#49452=CARTESIAN_POINT('Ctrl Pts',(5.80760183254679,-1.18131633985124,82.1307337091853));
#49453=CARTESIAN_POINT('Ctrl Pts',(6.19877788182802,0.741788136076126,82.223541660401));
#49454=CARTESIAN_POINT('Ctrl Pts',(5.53979327732711,2.87850435322667,82.3163496116167));
#49455=CARTESIAN_POINT('Ctrl Pts',(4.13338803277648,4.24721681936542,82.4091575628324));
#49456=CARTESIAN_POINT('Ctrl Pts',(2.72698278822586,5.61592928550417,82.5019655140481));
#49457=CARTESIAN_POINT('Ctrl Pts',(0.573156903625285,6.21663800063106,82.5947734652638));
#49458=CARTESIAN_POINT('Ctrl Pts',(-1.33861388300644,5.77337511447358,82.6875814164795));
#49459=CARTESIAN_POINT('Ctrl Pts',(-3.25038466963839,5.33011222831604,82.7803893676952));
#49460=CARTESIAN_POINT('Ctrl Pts',(-4.92010035830155,3.84287774087407,82.873197318911));
#49461=CARTESIAN_POINT('Ctrl Pts',(-5.58068726159464,1.99491278718537,82.9660052701267));
#49462=CARTESIAN_POINT('Ctrl Pts',(-5.80755365057478,1.36026330516377,82.9978784493496));
#49463=CARTESIAN_POINT('Ctrl Pts',(-5.91539810822109,0.683067383672749,
83.0297516285724));
#49464=CARTESIAN_POINT('Ctrl Pts',(-5.91070653272951,0.00442589000008243,
83.0616248077953));
#49465=CARTESIAN_POINT('Origin',(0.,0.,-10.));
#49466=CARTESIAN_POINT('',(-5.90777653442157,-0.00228402886370327,85.0633751922047));
#49467=CARTESIAN_POINT('',(-5.90953574780485,-0.00382487655214481,84.8116248077953));
#49468=CARTESIAN_POINT('',(-5.91675,-7.2459289488551E-16,-10.));
#49469=CARTESIAN_POINT('Ctrl Pts',(-5.90777653442157,-0.00228402886370327,
85.0633751922047));
#49470=CARTESIAN_POINT('Ctrl Pts',(-5.9038637091048,1.12899760163664,85.010309238702));
#49471=CARTESIAN_POINT('Ctrl Pts',(-5.59150136727689,2.26227968995058,84.9572432851992));
#49472=CARTESIAN_POINT('Ctrl Pts',(-4.9844756224772,3.20603318586317,84.9041773316965));
#49473=CARTESIAN_POINT('Ctrl Pts',(-3.92304605055994,4.85625622457871,84.8113875731197));
#49474=CARTESIAN_POINT('Ctrl Pts',(-1.96067963993461,5.92699335102708,84.7185978145429));
#49475=CARTESIAN_POINT('Ctrl Pts',(0.0014285604354887,5.92652039388547,
84.6258080559661));
#49476=CARTESIAN_POINT('Ctrl Pts',(1.96353676080559,5.92604743674386,84.5330182973894));
#49477=CARTESIAN_POINT('Ctrl Pts',(3.92538675092045,4.85436439601227,84.4402285388127));
#49478=CARTESIAN_POINT('Ctrl Pts',(4.98602064221901,3.20362984367597,84.3474387802359));
#49479=CARTESIAN_POINT('Ctrl Pts',(6.04665453351756,1.55289529133967,84.2546490216591));
#49480=CARTESIAN_POINT('Ctrl Pts',(6.2060723259998,-0.67689077260134,84.1618592630823));
#49481=CARTESIAN_POINT('Ctrl Pts',(5.39106316336296,-2.46172378396852,84.0690695045056));
#49482=CARTESIAN_POINT('Ctrl Pts',(4.57605400072608,-4.2465567953358,83.9762797459288));
#49483=CARTESIAN_POINT('Ctrl Pts',(2.78661788297001,-5.58643675412919,83.8834899873521));
#49484=CARTESIAN_POINT('Ctrl Pts',(0.844533536547844,-5.86603862291848,
83.7907002287754));
#49485=CARTESIAN_POINT('Ctrl Pts',(-1.09755080987421,-6.14564049170775,
83.6979104701987));
#49486=CARTESIAN_POINT('Ctrl Pts',(-3.19228338496234,-5.36496427049303,
83.6051207116218));
#49487=CARTESIAN_POINT('Ctrl Pts',(-4.47768144413318,-3.88252687109706,
83.5123309530451));
#49488=CARTESIAN_POINT('Ctrl Pts',(-5.3963796308283,-2.82300095926192,83.4460123660983));
#49489=CARTESIAN_POINT('Ctrl Pts',(-5.90165113649419,-1.40499930091568,
83.3796937791515));
#49490=CARTESIAN_POINT('Ctrl Pts',(-5.91367641053724,0.00526281327289491,
83.3133751922047));
#49491=CARTESIAN_POINT('Ctrl Pts',(-5.91070653272951,0.00442589000008243,
83.0616248077953));
#49492=CARTESIAN_POINT('Ctrl Pts',(-5.90173723346798,-1.29299299603636,
83.1225595797881));
#49493=CARTESIAN_POINT('Ctrl Pts',(-5.48145609199123,-2.59569535386845,
83.183494351781));
#49494=CARTESIAN_POINT('Ctrl Pts',(-4.69518307107893,-3.61649046303929,
83.2444291237738));
#49495=CARTESIAN_POINT('Ctrl Pts',(-3.49763385934694,-5.1712333396409,83.3372370749895));
#49496=CARTESIAN_POINT('Ctrl Pts',(-1.45107731795962,-6.07202367290896,
83.4300450262052));
#49497=CARTESIAN_POINT('Ctrl Pts',(0.504290756076211,-5.90503498495449,
83.522852977421));
#49498=CARTESIAN_POINT('Ctrl Pts',(2.45965883011204,-5.73804629700002,83.6156609286367));
#49499=CARTESIAN_POINT('Ctrl Pts',(4.32383843679622,-4.50327858782326,83.7084688798523));
#49500=CARTESIAN_POINT('Ctrl Pts',(5.24041843105424,-2.76798880194039,83.801276831068));
#49501=CARTESIAN_POINT('Ctrl Pts',(6.15699842531226,-1.03269901605751,83.8940847822837));
#49502=CARTESIAN_POINT('Ctrl Pts',(6.1259788071438,1.20311284653135,83.9868927334994));
#49503=CARTESIAN_POINT('Ctrl Pts',(5.16161010617607,2.9123063801773,84.0797006847152));
#49504=CARTESIAN_POINT('Ctrl Pts',(4.1972414052084,4.62149991382316,84.1725086359309));
#49505=CARTESIAN_POINT('Ctrl Pts',(2.2995236214415,5.80407511852627,84.2653165871466));
#49506=CARTESIAN_POINT('Ctrl Pts',(0.34027546504553,5.91675248325366,84.3581245383623));
#49507=CARTESIAN_POINT('Ctrl Pts',(-1.61897269135055,6.02942984798107,84.450932489578));
#49508=CARTESIAN_POINT('Ctrl Pts',(-3.63975122037582,5.0722093727326,84.5437404407937));
#49509=CARTESIAN_POINT('Ctrl Pts',(-4.793706841166,3.4848417555405,84.6365483920094));
#49510=CARTESIAN_POINT('Ctrl Pts',(-5.51932862758084,2.48668506274214,84.6949071972713));
#49511=CARTESIAN_POINT('Ctrl Pts',(-5.90220409926062,1.23936489192517,84.7532660025333));
#49512=CARTESIAN_POINT('Ctrl Pts',(-5.90953574780485,-0.00382487655214481,
84.8116248077953));
#49513=CARTESIAN_POINT('Origin',(0.,0.,-10.));
#49514=CARTESIAN_POINT('',(-5.92207245583525,-0.00440905045111684,86.8133751922048));
#49515=CARTESIAN_POINT('',(-5.92469646081808,-0.00297539080508188,86.5616248077953));
#49516=CARTESIAN_POINT('',(-5.91675,-7.2459289488551E-16,-10.));
#49517=CARTESIAN_POINT('Ctrl Pts',(-5.92207245583525,-0.00440905045111684,
86.8133751922048));
#49518=CARTESIAN_POINT('Ctrl Pts',(-5.90803226273657,1.68341667196022,86.7337144568292));
#49519=CARTESIAN_POINT('Ctrl Pts',(-5.14989886133249,3.38225938529491,86.6540537214536));
#49520=CARTESIAN_POINT('Ctrl Pts',(-3.87548104107258,4.48378107407268,86.574392986078));
#49521=CARTESIAN_POINT('Ctrl Pts',(-2.39102422165811,5.76684645235311,86.4816032275013));
#49522=CARTESIAN_POINT('Ctrl Pts',(-0.206079747760587,6.23947481532992,
86.3888134689245));
#49523=CARTESIAN_POINT('Ctrl Pts',(1.6759408202332,5.6846168197163,86.2960237103478));
#49524=CARTESIAN_POINT('Ctrl Pts',(3.5579613882271,5.12975882410264,86.203233951771));
#49525=CARTESIAN_POINT('Ctrl Pts',(5.13705805031723,3.54741446989843,86.1104441931943));
#49526=CARTESIAN_POINT('Ctrl Pts',(5.68804814642293,1.66425788383293,86.0176544346175));
#49527=CARTESIAN_POINT('Ctrl Pts',(6.2390382425286,-0.218898702232475,85.9248646760407));
#49528=CARTESIAN_POINT('Ctrl Pts',(5.76192177264996,-2.40286752015914,85.8320749174639));
#49529=CARTESIAN_POINT('Ctrl Pts',(4.47580919348121,-3.88468506876354,85.7392851588872));
#49530=CARTESIAN_POINT('Ctrl Pts',(3.18969661431247,-5.36650261736794,85.6464954003104));
#49531=CARTESIAN_POINT('Ctrl Pts',(1.09458792585362,-6.14616889665008,85.5537056417338));
#49532=CARTESIAN_POINT('Ctrl Pts',(-0.847361401410383,-5.86563079943881,
85.460915883157));
#49533=CARTESIAN_POINT('Ctrl Pts',(-2.7893107286745,-5.58509270222752,85.3681261245802));
#49534=CARTESIAN_POINT('Ctrl Pts',(-4.57810069474375,-4.24435022852271,
85.2753363660034));
#49535=CARTESIAN_POINT('Ctrl Pts',(-5.39224931117372,-2.45912451617885,
85.1825466074266));
#49536=CARTESIAN_POINT('Ctrl Pts',(-5.74079080364409,-1.69485958761427,
85.1428228023527));
#49537=CARTESIAN_POINT('Ctrl Pts',(-5.91070557460482,-0.849132299881903,
85.1030989972787));
#49538=CARTESIAN_POINT('Ctrl Pts',(-5.90777653442157,-0.00228402886370327,
85.0633751922047));
#49539=CARTESIAN_POINT('Ctrl Pts',(-5.90953574780485,-0.00382487655214481,
84.8116248077953));
#49540=CARTESIAN_POINT('Ctrl Pts',(-5.91386361280565,-0.737678587063048,
84.8460739537491));
#49541=CARTESIAN_POINT('Ctrl Pts',(-5.78733212812688,-1.47009304673082,
84.8805230997029));
#49542=CARTESIAN_POINT('Ctrl Pts',(-5.52319512729882,-2.14896787458142,
84.9149722456566));
#49543=CARTESIAN_POINT('Ctrl Pts',(-4.81159508008634,-3.97789512837534,
85.0077801968723));
#49544=CARTESIAN_POINT('Ctrl Pts',(-3.10126227310632,-5.41823487682758,
85.1005881480879));
#49545=CARTESIAN_POINT('Ctrl Pts',(-1.17793005116786,-5.80828960493156,
85.1933960993036));
#49546=CARTESIAN_POINT('Ctrl Pts',(0.745402170770599,-6.19834433303554,
85.2862040505193));
#49547=CARTESIAN_POINT('Ctrl Pts',(2.8817338076675,-5.53811404079126,85.3790120017351));
#49548=CARTESIAN_POINT('Ctrl Pts',(4.24962604490735,-4.13091101558063,85.4718199529508));
#49549=CARTESIAN_POINT('Ctrl Pts',(5.61751828214736,-2.72370799036984,85.5646279041665));
#49550=CARTESIAN_POINT('Ctrl Pts',(6.21697111973009,-0.569532232192492,
85.6574358553822));
#49551=CARTESIAN_POINT('Ctrl Pts',(5.77259366226549,1.34197978769155,85.7502438065979));
#49552=CARTESIAN_POINT('Ctrl Pts',(5.32821620480093,3.25349180757538,85.8430517578136));
#49553=CARTESIAN_POINT('Ctrl Pts',(3.84000845228928,4.92234008916595,85.9358597090294));
#49554=CARTESIAN_POINT('Ctrl Pts',(1.99165866141347,5.58184943514397,86.0286676602451));
#49555=CARTESIAN_POINT('Ctrl Pts',(0.143308870537557,6.24135878112202,86.1214756114608));
#49556=CARTESIAN_POINT('Ctrl Pts',(-2.06518295870255,5.89152919148742,86.2142835626764));
#49557=CARTESIAN_POINT('Ctrl Pts',(-3.61922734706008,4.69307369966558,86.3070915138921));
#49558=CARTESIAN_POINT('Ctrl Pts',(-5.03992471856324,3.5974534073171,86.3919359451932));
#49559=CARTESIAN_POINT('Ctrl Pts',(-5.91366772982529,1.79259413194367,86.4767803764943));
#49560=CARTESIAN_POINT('Ctrl Pts',(-5.92469646081808,-0.00297539080508188,
86.5616248077953));
#49561=CARTESIAN_POINT('Origin',(0.,0.,-10.));
#49562=CARTESIAN_POINT('',(-5.92187722747348,0.00448342927688694,88.5633751922048));
#49563=CARTESIAN_POINT('',(-5.91874116782466,0.00528482168223352,88.3116248077953));
#49564=CARTESIAN_POINT('',(-5.91675,-7.2459289488551E-16,-10.));
#49565=CARTESIAN_POINT('Ctrl Pts',(-5.92187722747348,0.00448342927688694,
88.5633751922048));
#49566=CARTESIAN_POINT('Ctrl Pts',(-5.92427836346706,0.289816032030938,
88.5499094335332));
#49567=CARTESIAN_POINT('Ctrl Pts',(-5.9054462137803,0.574830296895836,88.5364436748616));
#49568=CARTESIAN_POINT('Ctrl Pts',(-5.86429109524329,0.856583895585025,
88.52297791619));
#49569=CARTESIAN_POINT('Ctrl Pts',(-5.58069968339791,2.79808968356919,88.4301881576132));
#49570=CARTESIAN_POINT('Ctrl Pts',(-4.23714604467594,4.58476915772875,88.3373983990364));
#49571=CARTESIAN_POINT('Ctrl Pts',(-2.45064231334397,5.39610954966386,88.2446086404596));
#49572=CARTESIAN_POINT('Ctrl Pts',(-0.664138582012099,6.20744994159892,
88.1518188818829));
#49573=CARTESIAN_POINT('Ctrl Pts',(1.56531524192973,6.04345125130962,88.0590291233061));
#49574=CARTESIAN_POINT('Ctrl Pts',(3.21386717184441,4.97942806170208,87.9662393647294));
#49575=CARTESIAN_POINT('Ctrl Pts',(4.8624191017591,3.91540487209454,87.8734496061526));
#49576=CARTESIAN_POINT('Ctrl Pts',(5.93006913764664,1.95135718316875,87.7806598475759));
#49577=CARTESIAN_POINT('Ctrl Pts',(5.92651082034749,-0.0107478476657502,
87.6878700889991));
#49578=CARTESIAN_POINT('Ctrl Pts',(5.92295250304835,-1.97285287850036,87.5950803304223));
#49579=CARTESIAN_POINT('Ctrl Pts',(4.84818583256239,-3.93301525124367,87.5022905718456));
#49580=CARTESIAN_POINT('Ctrl Pts',(3.19578550370114,-4.99105209692896,87.4095008132688));
#49581=CARTESIAN_POINT('Ctrl Pts',(1.54338517483998,-6.0490889426142,87.316711054692));
#49582=CARTESIAN_POINT('Ctrl Pts',(-0.686648812396377,-6.20500026124158,
87.2239212961153));
#49583=CARTESIAN_POINT('Ctrl Pts',(-2.47019803780075,-5.38718550580641,
87.1311315375386));
#49584=CARTESIAN_POINT('Ctrl Pts',(-4.25374726320513,-4.56937075037125,
87.0383417789618));
#49585=CARTESIAN_POINT('Ctrl Pts',(-5.59081172677752,-2.77782992087354,
86.9455520203851));
#49586=CARTESIAN_POINT('Ctrl Pts',(-5.867359376098,-0.83530830933267,86.8527622618084));
#49587=CARTESIAN_POINT('Ctrl Pts',(-5.90648869984939,-0.560456734138262,
86.8396332386071));
#49588=CARTESIAN_POINT('Ctrl Pts',(-5.92438644427727,-0.282582519031695,
86.826504215406));
#49589=CARTESIAN_POINT('Ctrl Pts',(-5.92207245583525,-0.00440905045111684,
86.8133751922048));
#49590=CARTESIAN_POINT('Ctrl Pts',(-5.92469646081808,-0.00297539080508188,
86.5616248077953));
#49591=CARTESIAN_POINT('Ctrl Pts',(-5.92573162031586,-0.171508003179695,
86.56958832771));
#49592=CARTESIAN_POINT('Ctrl Pts',(-5.9191664849481,-0.339958775180508,
86.5775518476247));
#49593=CARTESIAN_POINT('Ctrl Pts',(-5.90473995753208,-0.507733566080088,
86.5855153675394));
#49594=CARTESIAN_POINT('Ctrl Pts',(-5.73661123217162,-2.46300394599478,
86.6783233187551));
#49595=CARTESIAN_POINT('Ctrl Pts',(-4.5007568339759,-4.32646331181517,86.7711312699708));
#49596=CARTESIAN_POINT('Ctrl Pts',(-2.76493293649683,-5.24203139983684,
86.8639392211865));
#49597=CARTESIAN_POINT('Ctrl Pts',(-1.02910903901766,-6.15759948785856,
86.9567471724022));
#49598=CARTESIAN_POINT('Ctrl Pts',(1.20668435774482,-6.12527629808141,87.0495551236178));
#49599=CARTESIAN_POINT('Ctrl Pts',(2.9153153314122,-5.15991122584811,87.1423630748336));
#49600=CARTESIAN_POINT('Ctrl Pts',(4.62394630507958,-4.19454615361481,87.2351710260493));
#49601=CARTESIAN_POINT('Ctrl Pts',(5.80541485565174,-2.29613919892545,87.327978977265));
#49602=CARTESIAN_POINT('Ctrl Pts',(5.91694987317906,-0.336825679672146,
87.4207869284808));
#49603=CARTESIAN_POINT('Ctrl Pts',(6.02848489070638,1.62248783958105,87.5135948796964));
#49604=CARTESIAN_POINT('Ctrl Pts',(5.07008637518878,3.64270792339829,87.6064028309121));
#49605=CARTESIAN_POINT('Ctrl Pts',(3.4820462208031,4.7957378427507,87.6992107821278));
#49606=CARTESIAN_POINT('Ctrl Pts',(1.89400606641742,5.94876776210311,87.7920187333436));
#49607=CARTESIAN_POINT('Ctrl Pts',(-0.323675726836286,6.23460751699098,
87.8848266845593));
#49608=CARTESIAN_POINT('Ctrl Pts',(-2.15218777556883,5.52194124551253,87.977634635775));
#49609=CARTESIAN_POINT('Ctrl Pts',(-3.98069982430137,4.80927497403408,88.0704425869907));
#49610=CARTESIAN_POINT('Ctrl Pts',(-5.42004212851265,3.09810267618934,88.1632505382064));
#49611=CARTESIAN_POINT('Ctrl Pts',(-5.80897540284391,1.1745433620581,88.2560584894221));
#49612=CARTESIAN_POINT('Ctrl Pts',(-5.88659659034037,0.790649856316099,
88.2745805955465));
#49613=CARTESIAN_POINT('Ctrl Pts',(-5.92237998049169,0.398296974565935,
88.2931027016709));
#49614=CARTESIAN_POINT('Ctrl Pts',(-5.91874116782466,0.00528482168223352,
88.3116248077953));
#49615=CARTESIAN_POINT('Origin',(0.,0.,-10.));
#49616=CARTESIAN_POINT('',(-5.9076957588592,0.00217524021099064,90.3133751922047));
#49617=CARTESIAN_POINT('',(-5.90697520874472,0.000492460854587244,90.0616248077953));
#49618=CARTESIAN_POINT('',(-5.91675,-7.2459289488551E-16,-10.));
#49619=CARTESIAN_POINT('Ctrl Pts',(-5.9076957588592,0.00217524021099064,
90.3133751922047));
#49620=CARTESIAN_POINT('Ctrl Pts',(-5.91050674814863,0.856231332472319,
90.2733146516603));
#49621=CARTESIAN_POINT('Ctrl Pts',(-5.73758377480165,1.70920259929656,90.2332541111159));
#49622=CARTESIAN_POINT('Ctrl Pts',(-5.38329452751489,2.47866618364667,90.1931935705715));
#49623=CARTESIAN_POINT('Ctrl Pts',(-4.56267620146798,4.26092721295859,90.1004038119948));
#49624=CARTESIAN_POINT('Ctrl Pts',(-2.76903509011887,5.59517287519017,90.007614053418));
#49625=CARTESIAN_POINT('Ctrl Pts',(-0.826081016675218,5.86866562123062,
89.9148242948413));
#49626=CARTESIAN_POINT('Ctrl Pts',(1.11687305676854,6.14215836727109,89.8220345362645));
#49627=CARTESIAN_POINT('Ctrl Pts',(3.20914009230686,5.35489819712032,89.7292447776878));
#49628=CARTESIAN_POINT('Ctrl Pts',(4.48986961709886,3.86842562825989,89.636455019111));
#49629=CARTESIAN_POINT('Ctrl Pts',(5.77059914189078,2.38195305939954,89.5436652605342));
#49630=CARTESIAN_POINT('Ctrl Pts',(6.23979115593646,0.196268091829603,89.4508755019574));
#49631=CARTESIAN_POINT('Ctrl Pts',(5.68197442115233,-1.684877650542,89.3580857433807));
#49632=CARTESIAN_POINT('Ctrl Pts',(5.1241576863682,-3.5660233929136,89.265295984804));
#49633=CARTESIAN_POINT('Ctrl Pts',(3.53933220275425,-5.14262991008687,89.1725062262272));
#49634=CARTESIAN_POINT('Ctrl Pts',(1.65531152825281,-5.6906581134662,89.0797164676505));
#49635=CARTESIAN_POINT('Ctrl Pts',(-0.228709146248734,-6.23868631684556,
88.9869267090737));
#49636=CARTESIAN_POINT('Ctrl Pts',(-2.4119250116378,-5.75813620643085,88.8941369504969));
#49637=CARTESIAN_POINT('Ctrl Pts',(-3.89171835184781,-4.46969510031906,
88.8013471919202));
#49638=CARTESIAN_POINT('Ctrl Pts',(-5.15676234569935,-3.3682340797641,88.722023192015));
#49639=CARTESIAN_POINT('Ctrl Pts',(-5.90773263183859,-1.67635193290292,
88.6426991921099));
#49640=CARTESIAN_POINT('Ctrl Pts',(-5.92187722747348,0.00448342927688694,
88.5633751922048));
#49641=CARTESIAN_POINT('Ctrl Pts',(-5.91874116782466,0.00528482168223352,
88.3116248077953));
#49642=CARTESIAN_POINT('Ctrl Pts',(-5.90414713233627,-1.57095276771637,
88.3859106528866));
#49643=CARTESIAN_POINT('Ctrl Pts',(-5.25543187432754,-3.15779498565621,
88.4601964979779));
#49644=CARTESIAN_POINT('Ctrl Pts',(-4.12843259412039,-4.25203382583027,
88.5344823430692));
#49645=CARTESIAN_POINT('Ctrl Pts',(-2.72043226661461,-5.61910536916916,
88.6272902942849));
#49646=CARTESIAN_POINT('Ctrl Pts',(-0.56590736715238,-6.2173021254292,88.7200982455007));
#49647=CARTESIAN_POINT('Ctrl Pts',(1.34534523618347,-5.77181024771941,88.8129061967164));
#49648=CARTESIAN_POINT('Ctrl Pts',(3.2565978395191,-5.32631837000967,88.9057141479321));
#49649=CARTESIAN_POINT('Ctrl Pts',(4.92457814672832,-3.83713785832991,88.9985220991478));
#49650=CARTESIAN_POINT('Ctrl Pts',(5.58300971119721,-1.98840385859563,89.0913300503635));
#49651=CARTESIAN_POINT('Ctrl Pts',(6.24144127566621,-0.13966985886104,89.1841380015792));
#49652=CARTESIAN_POINT('Ctrl Pts',(5.89032409739495,2.06861762892818,89.276945952795));
#49653=CARTESIAN_POINT('Ctrl Pts',(4.69096273288672,3.62196300075916,89.3697539040107));
#49654=CARTESIAN_POINT('Ctrl Pts',(3.49160136837863,5.17530837258996,89.4625618552264));
#49655=CARTESIAN_POINT('Ctrl Pts',(1.44399581763367,6.07371162846243,89.555369806442));
#49656=CARTESIAN_POINT('Ctrl Pts',(-0.511176203484458,5.90444292284984,
89.6481777576577));
#49657=CARTESIAN_POINT('Ctrl Pts',(-2.4663482246027,5.73517421723724,89.7409857088734));
#49658=CARTESIAN_POINT('Ctrl Pts',(-4.32908671609423,4.49823355013946,89.8337936600891));
#49659=CARTESIAN_POINT('Ctrl Pts',(-5.24364258664101,2.76187613114078,89.9266016113049));
#49660=CARTESIAN_POINT('Ctrl Pts',(-5.68716154305487,1.91981994273608,89.9716093434683));
#49661=CARTESIAN_POINT('Ctrl Pts',(-5.90768511163,0.960309975045309,90.0166170756318));
#49662=CARTESIAN_POINT('Ctrl Pts',(-5.90697520874472,0.000492460854587244,
90.0616248077953));
#49663=CARTESIAN_POINT('Origin',(0.,0.,-10.));
#49664=CARTESIAN_POINT('',(-5.91387952939735,-0.00529439012957766,92.0633751922047));
#49665=CARTESIAN_POINT('',(-5.9169276701952,-0.00545620570378101,91.8116248077953));
#49666=CARTESIAN_POINT('',(-5.91675,-7.2459289488551E-16,-10.));
#49667=CARTESIAN_POINT('Ctrl Pts',(-5.91387952939735,-0.00529439012957766,
92.0633751922047));
#49668=CARTESIAN_POINT('Ctrl Pts',(-5.90168899007384,1.41200501326097,91.9967198697875));
#49669=CARTESIAN_POINT('Ctrl Pts',(-5.39078924113146,2.8371923802721,91.9300645473704));
#49670=CARTESIAN_POINT('Ctrl Pts',(-4.46356995507357,3.89874201199438,91.8634092249532));
#49671=CARTESIAN_POINT('Ctrl Pts',(-3.17280350790947,5.37650748476838,91.7706194663764));
#49672=CARTESIAN_POINT('Ctrl Pts',(-1.07525317628989,6.14958091583901,91.6778297077997));
#49673=CARTESIAN_POINT('Ctrl Pts',(0.865804271709872,5.86293689058771,91.5850399492229));
#49674=CARTESIAN_POINT('Ctrl Pts',(2.80686171970985,5.57629286533638,91.4922501906461));
#49675=CARTESIAN_POINT('Ctrl Pts',(4.59142628408996,4.22993138376282,91.3994604320693));
#49676=CARTESIAN_POINT('Ctrl Pts',(5.39995644535267,2.44215405087794,91.3066706734926));
#49677=CARTESIAN_POINT('Ctrl Pts',(6.20848660661528,0.654376717993263,91.2138809149158));
#49678=CARTESIAN_POINT('Ctrl Pts',(6.04098236476071,-1.57481646620264,91.1210911563391));
#49679=CARTESIAN_POINT('Ctrl Pts',(4.97436818844188,-3.22169321099058,91.0283013977624));
#49680=CARTESIAN_POINT('Ctrl Pts',(3.90775401212288,-4.86856995577879,90.9355116391856));
#49681=CARTESIAN_POINT('Ctrl Pts',(1.94202990133927,-5.93313026115881,90.8427218806088));
#49682=CARTESIAN_POINT('Ctrl Pts',(-0.020067108320463,-5.92648659250057,
90.749932122032));
#49683=CARTESIAN_POINT('Ctrl Pts',(-1.98216411797986,-5.91984292384233,
90.6571423634553));
#49684=CARTESIAN_POINT('Ctrl Pts',(-3.94063402651538,-4.84199528114619,
90.5643526048786));
#49685=CARTESIAN_POINT('Ctrl Pts',(-4.99607121041088,-3.18793326160208,
90.4715628463019));
#49686=CARTESIAN_POINT('Ctrl Pts',(-5.59583974351959,-2.24798689030669,
90.4188336282695));
#49687=CARTESIAN_POINT('Ctrl Pts',(-5.90399582707808,-1.12196610408279,
90.3661044102371));
#49688=CARTESIAN_POINT('Ctrl Pts',(-5.9076957588592,0.00217524021099064,
90.3133751922047));
#49689=CARTESIAN_POINT('Ctrl Pts',(-5.90697520874472,0.000492460854587244,
90.0616248077953));
#49690=CARTESIAN_POINT('Ctrl Pts',(-5.90622126021652,-1.01887655027118,
90.1094250268476));
#49691=CARTESIAN_POINT('Ctrl Pts',(-5.6559295087634,-2.03859245500849,90.1572252458998));
#49692=CARTESIAN_POINT('Ctrl Pts',(-5.15821059145769,-2.91832329161354,
90.2050254649521));
#49693=CARTESIAN_POINT('Ctrl Pts',(-4.19184947612554,-4.62639112446941,
90.2978334161678));
#49694=CARTESIAN_POINT('Ctrl Pts',(-2.29275399585916,-5.80675261928172,
90.3906413673834));
#49695=CARTESIAN_POINT('Ctrl Pts',(-0.333375779798765,-5.91714525169392,
90.4834493185991));
#49696=CARTESIAN_POINT('Ctrl Pts',(1.62600243626174,-6.02753788410612,90.5762572698148));
#49697=CARTESIAN_POINT('Ctrl Pts',(3.64566338811639,-5.06796165411809,90.6690652210306));
#49698=CARTESIAN_POINT('Ctrl Pts',(4.79776721406981,-3.47924950237795,90.7618731722463));
#49699=CARTESIAN_POINT('Ctrl Pts',(5.94987104002329,-1.89053735063771,90.854681123462));
#49700=CARTESIAN_POINT('Ctrl Pts',(6.23441774007554,0.327310722854481,90.9474890746777));
#49701=CARTESIAN_POINT('Ctrl Pts',(5.52068548659514,2.1554069449406,91.0402970258934));
#49702=CARTESIAN_POINT('Ctrl Pts',(4.80695323311482,3.98350316702652,91.1331049771091));
#49703=CARTESIAN_POINT('Ctrl Pts',(3.09494202610193,5.42184753770625,91.2259129283248));
#49704=CARTESIAN_POINT('Ctrl Pts',(1.17115627367356,5.80965922605064,91.3187208795405));
#49705=CARTESIAN_POINT('Ctrl Pts',(-0.752629478754913,6.19747091439506,
91.4115288307563));
#49706=CARTESIAN_POINT('Ctrl Pts',(-2.88818977659902,5.53474992040405,91.5043367819719));
#49707=CARTESIAN_POINT('Ctrl Pts',(-4.25444016131426,4.12595276923969,91.5971447331876));
#49708=CARTESIAN_POINT('Ctrl Pts',(-5.30691278752029,3.04070481318033,91.6686380913902));
#49709=CARTESIAN_POINT('Ctrl Pts',(-5.90286273979908,1.51272152196721,91.7401314495928));
#49710=CARTESIAN_POINT('Ctrl Pts',(-5.9169276701952,-0.00545620570378101,
91.8116248077953));
#49711=CARTESIAN_POINT('Origin',(0.,0.,-10.));
#49712=CARTESIAN_POINT('',(-5.92651347487416,0.000183341992167018,93.8133751922047));
#49713=CARTESIAN_POINT('',(-5.92571112046846,0.00200453863705335,93.5616248077953));
#49714=CARTESIAN_POINT('',(-5.91675,-7.2459289488551E-16,-10.));
#49715=CARTESIAN_POINT('Ctrl Pts',(-5.92651347487416,0.000183341992167018,
93.8133751922047));
#49716=CARTESIAN_POINT('Ctrl Pts',(-5.92651787928802,0.00991772496236695,
93.8129148464915));
#49717=CARTESIAN_POINT('Ctrl Pts',(-5.92649597763976,0.0196520875258746,
93.8124545007783));
#49718=CARTESIAN_POINT('Ctrl Pts',(-5.92644771040461,0.0293863193554934,
93.811994155065));
#49719=CARTESIAN_POINT('Ctrl Pts',(-5.91671870681498,1.99147045622047,93.7192043964883));
#49720=CARTESIAN_POINT('Ctrl Pts',(-4.83579275707057,3.94824305789768,93.6264146379115));
#49721=CARTESIAN_POINT('Ctrl Pts',(-3.18007313679368,5.00107797025487,93.5336248793348));
#49722=CARTESIAN_POINT('Ctrl Pts',(-1.52435351651669,6.05391288261212,93.440835120758));
#49723=CARTESIAN_POINT('Ctrl Pts',(0.70615977429284,6.20281010564926,93.3480453621812));
#49724=CARTESIAN_POINT('Ctrl Pts',(2.48712820056795,5.37939023810924,93.2552556036045));
#49725=CARTESIAN_POINT('Ctrl Pts',(4.26809662684306,4.55597037056921,93.1624658450277));
#49726=CARTESIAN_POINT('Ctrl Pts',(5.59952018858376,2.76023341245207,93.069676086451));
#49727=CARTESIAN_POINT('Ctrl Pts',(5.86995735508652,0.816851681390876,92.9768863278743));
#49728=CARTESIAN_POINT('Ctrl Pts',(6.14039452158924,-1.1265300496701,92.8840965692975));
#49729=CARTESIAN_POINT('Ctrl Pts',(5.3498452928543,-3.2175565536751,92.7913068107207));
#49730=CARTESIAN_POINT('Ctrl Pts',(3.86136065010522,-4.49594705815631,92.6985170521439));
#49731=CARTESIAN_POINT('Ctrl Pts',(2.37287600735604,-5.77433756263759,92.6057272935672));
#49732=CARTESIAN_POINT('Ctrl Pts',(0.186455950592636,-6.240092067595,92.5129375349904));
#49733=CARTESIAN_POINT('Ctrl Pts',(-1.69381031470308,-5.67931797293749,
92.4201477764137));
#49734=CARTESIAN_POINT('Ctrl Pts',(-3.57407657999879,-5.11854387827999,
92.3273580178369));
#49735=CARTESIAN_POINT('Ctrl Pts',(-5.14818905382682,-3.53124118400757,
92.2345682592602));
#49736=CARTESIAN_POINT('Ctrl Pts',(-5.69325400938658,-1.64636107963258,
92.1417785006834));
#49737=CARTESIAN_POINT('Ctrl Pts',(-5.84677273281456,-1.11548052221118,
92.1156440645238));
#49738=CARTESIAN_POINT('Ctrl Pts',(-5.91865923580559,-0.560993761667654,
92.0895096283643));
#49739=CARTESIAN_POINT('Ctrl Pts',(-5.91387952939735,-0.00529439012957766,
92.0633751922047));
#49740=CARTESIAN_POINT('Ctrl Pts',(-5.9169276701952,-0.00545620570378101,
91.8116248077953));
#49741=CARTESIAN_POINT('Ctrl Pts',(-5.92112090261132,-0.458076437856095,
91.8329394008085));
#49742=CARTESIAN_POINT('Ctrl Pts',(-5.87359397348391,-0.909825114097263,
91.8542539938217));
#49743=CARTESIAN_POINT('Ctrl Pts',(-5.77102487110158,-1.34871022733847,
91.8755685868349));
#49744=CARTESIAN_POINT('Ctrl Pts',(-5.32441872458721,-3.25970276441396,
91.9683765380506));
#49745=CARTESIAN_POINT('Ctrl Pts',(-3.83426595997241,-4.9268145302274,92.0611844892662));
#49746=CARTESIAN_POINT('Ctrl Pts',(-1.98514837983892,-5.58416808935971,
92.1539924404818));
#49747=CARTESIAN_POINT('Ctrl Pts',(-0.136030799705217,-6.24152164849209,
92.2468003916975));
#49748=CARTESIAN_POINT('Ctrl Pts',(2.07205159594715,-5.88911700094308,92.3396083429134));
#49749=CARTESIAN_POINT('Ctrl Pts',(3.62469742320657,-4.68885017145995,92.4324162941291));
#49750=CARTESIAN_POINT('Ctrl Pts',(5.17734325046581,-3.48858334197697,92.5252242453448));
#49751=CARTESIAN_POINT('Ctrl Pts',(6.07455250933224,-1.44045433055982,92.6180321965605));
#49752=CARTESIAN_POINT('Ctrl Pts',(5.90414388100869,0.514618667119702,92.7108401477762));
#49753=CARTESIAN_POINT('Ctrl Pts',(5.73373525268511,2.46969166479956,92.8036480989918));
#49754=CARTESIAN_POINT('Ctrl Pts',(4.49570873717139,4.33170864874189,92.8964560502076));
#49755=CARTESIAN_POINT('Ctrl Pts',(2.75881838691105,5.2452519909192,92.9892640014233));
#49756=CARTESIAN_POINT('Ctrl Pts',(1.02192803665091,6.15879533309641,93.0820719526391));
#49757=CARTESIAN_POINT('Ctrl Pts',(-1.21382614835559,6.1238650335088,93.1748799038548));
#49758=CARTESIAN_POINT('Ctrl Pts',(-2.9213302597588,5.15650820358292,93.2676878550704));
#49759=CARTESIAN_POINT('Ctrl Pts',(-4.628834371162,4.18915137365705,93.3604958062862));
#49760=CARTESIAN_POINT('Ctrl Pts',(-5.80808840896181,2.28936801339296,93.4533037575018));
#49761=CARTESIAN_POINT('Ctrl Pts',(-5.91733861873187,0.329925766597139,
93.5461117087175));
#49762=CARTESIAN_POINT('Ctrl Pts',(-5.92342577436248,0.220750416448644,
93.5512827417434));
#49763=CARTESIAN_POINT('Ctrl Pts',(-5.92619115980276,0.111389858447922,
93.5564537747694));
#49764=CARTESIAN_POINT('Ctrl Pts',(-5.92571112046846,0.00200453863705335,
93.5616248077953));
#49765=CARTESIAN_POINT('Origin',(0.,0.,-10.));
#49766=CARTESIAN_POINT('',(-5.91332833078945,0.00520191486789418,95.5633751922047));
#49767=CARTESIAN_POINT('',(-5.91081306495006,0.00447103847887896,95.3116248077953));
#49768=CARTESIAN_POINT('',(-5.91675,-7.2459289488551E-16,-10.));
#49769=CARTESIAN_POINT('Ctrl Pts',(-5.91332833078945,0.00520191486789418,
95.5633751922047));
#49770=CARTESIAN_POINT('Ctrl Pts',(-5.91815610750766,0.5806138957877,95.5363200646187));
#49771=CARTESIAN_POINT('Ctrl Pts',(-5.84101679508192,1.15475888064953,95.5092649370326));
#49772=CARTESIAN_POINT('Ctrl Pts',(-5.67664748164019,1.70273879062923,95.4822098094466));
#49773=CARTESIAN_POINT('Ctrl Pts',(-5.11291741371888,3.58212092957008,95.3894200508698));
#49774=CARTESIAN_POINT('Ctrl Pts',(-3.52314143366452,5.15373546779132,95.2966302922931));
#49775=CARTESIAN_POINT('Ctrl Pts',(-1.63740656010343,5.69583582776537,95.2038405337164));
#49776=CARTESIAN_POINT('Ctrl Pts',(0.248328313457552,6.2379361877394,95.1110507751396));
#49777=CARTESIAN_POINT('Ctrl Pts',(2.43002208052523,5.75052236946637,95.0182610165629));
#49778=CARTESIAN_POINT('Ctrl Pts',(3.90575603183626,4.45743377288996,94.9254712579861));
#49779=CARTESIAN_POINT('Ctrl Pts',(5.38148998314738,3.16434517631346,94.8326814994093));
#49780=CARTESIAN_POINT('Ctrl Pts',(6.15126411870176,1.06558180143349,94.7398917408325));
#49781=CARTESIAN_POINT('Ctrl Pts',(5.86156818882048,-0.875022506986626,
94.6471019822558));
#49782=CARTESIAN_POINT('Ctrl Pts',(5.57187225893923,-2.81562681540652,94.554312223679));
#49783=CARTESIAN_POINT('Ctrl Pts',(4.22270626362261,-4.59807205736659,94.4615224651023));
#49784=CARTESIAN_POINT('Ctrl Pts',(2.43365974976944,-5.40378998872806,94.3687327065256));
#49785=CARTESIAN_POINT('Ctrl Pts',(0.644613235916068,-6.20950792008962,
94.2759429479488));
#49786=CARTESIAN_POINT('Ctrl Pts',(-1.58431379647396,-6.03849854085236,
94.183153189372));
#49787=CARTESIAN_POINT('Ctrl Pts',(-3.22951128395157,-4.96929601520727,
94.0903634307953));
#49788=CARTESIAN_POINT('Ctrl Pts',(-4.86654666795568,-3.90539798444189,
93.9980340179318));
#49789=CARTESIAN_POINT('Ctrl Pts',(-5.92563010193588,-1.95219687661127,
93.9057046050682));
#49790=CARTESIAN_POINT('Ctrl Pts',(-5.92651347487416,0.000183341992167018,
93.8133751922047));
#49791=CARTESIAN_POINT('Ctrl Pts',(-5.92571112046846,0.00200453863705335,
93.5616248077953));
#49792=CARTESIAN_POINT('Ctrl Pts',(-5.91757557624406,-1.85182085280855,
93.6492617259851));
#49793=CARTESIAN_POINT('Ctrl Pts',(-4.97727862618378,-3.7127584114918,93.7368986441749));
#49794=CARTESIAN_POINT('Ctrl Pts',(-3.47645160121493,-4.79979495443404,
93.8245355623647));
#49795=CARTESIAN_POINT('Ctrl Pts',(-1.88706799218794,-5.95097229534155,
93.9173435135804));
#49796=CARTESIAN_POINT('Ctrl Pts',(0.33094560760626,-6.23422584382928,94.0101514647961));
#49797=CARTESIAN_POINT('Ctrl Pts',(2.15862538160178,-5.51942785097377,94.1029594160118));
#49798=CARTESIAN_POINT('Ctrl Pts',(3.98630515559761,-4.80462985811814,94.1957673672275));
#49799=CARTESIAN_POINT('Ctrl Pts',(5.4236511037946,-3.09178032391887,94.2885753184432));
#49800=CARTESIAN_POINT('Ctrl Pts',(5.8103410743193,-1.16776878716565,94.3813832696589));
#49801=CARTESIAN_POINT('Ctrl Pts',(6.19703104484399,0.756242749587451,94.4741912208746));
#49802=CARTESIAN_POINT('Ctrl Pts',(5.53306503769651,2.89141628889448,94.5669991720904));
#49803=CARTESIAN_POINT('Ctrl Pts',(4.12347154178058,4.25684505054225,94.6598071233061));
#49804=CARTESIAN_POINT('Ctrl Pts',(2.71387804586473,5.62227381218994,94.7526150745219));
#49805=CARTESIAN_POINT('Ctrl Pts',(0.558657061180529,6.21795779617846,94.8454230257375));
#49806=CARTESIAN_POINT('Ctrl Pts',(-1.35207476001135,5.77023753267928,94.9382309769532));
#49807=CARTESIAN_POINT('Ctrl Pts',(-3.26280658120333,5.32251726918006,95.0310389281689));
#49808=CARTESIAN_POINT('Ctrl Pts',(-4.92904923890296,3.83139275819302,95.1238468793846));
#49809=CARTESIAN_POINT('Ctrl Pts',(-5.58532456923768,1.98189222625001,95.2166548306003));
#49810=CARTESIAN_POINT('Ctrl Pts',(-5.80917914325876,1.35103024714942,95.2483114896653));
#49811=CARTESIAN_POINT('Ctrl Pts',(-5.91552580469876,0.678471851738488,
95.2799681487303));
#49812=CARTESIAN_POINT('Ctrl Pts',(-5.91081306495006,0.00447103847887897,
95.3116248077953));
#49813=CARTESIAN_POINT('Origin',(0.,0.,-10.));
#49814=CARTESIAN_POINT('',(-5.90792603807066,-0.00247015932851979,97.3133751922047));
#49815=CARTESIAN_POINT('',(-5.90944591666731,-0.00376931072489263,97.0616248077952));
#49816=CARTESIAN_POINT('',(-5.91675,-7.2459289488551E-16,-10.));
#49817=CARTESIAN_POINT('Ctrl Pts',(-5.90792603807066,-0.00247015932851979,
97.3133751922047));
#49818=CARTESIAN_POINT('Ctrl Pts',(-5.90364159030541,1.14118819633865,97.2597252827458));
#49819=CARTESIAN_POINT('Ctrl Pts',(-5.58390646962752,2.28706147908161,97.206075373287));
#49820=CARTESIAN_POINT('Ctrl Pts',(-4.96421155454115,3.23732137139418,97.1524254638282));
#49821=CARTESIAN_POINT('Ctrl Pts',(-3.89242332335584,4.88083553353004,97.0596357052514));
#49822=CARTESIAN_POINT('Ctrl Pts',(-1.923360954755,5.93920848862016,96.9668459466748));
#49823=CARTESIAN_POINT('Ctrl Pts',(0.0387054577278374,5.92639417415577,
96.8740561880981));
#49824=CARTESIAN_POINT('Ctrl Pts',(2.00077187021056,5.91357985969138,96.7812664295213));
#49825=CARTESIAN_POINT('Ctrl Pts',(3.95584232657529,4.82957827567259,96.6884766709445));
#49826=CARTESIAN_POINT('Ctrl Pts',(5.00607236408032,3.17220514871227,96.5956869123677));
#49827=CARTESIAN_POINT('Ctrl Pts',(6.0563024015854,1.51483202175186,96.502897153791));
#49828=CARTESIAN_POINT('Ctrl Pts',(6.20169202023064,-0.71591264815017,96.4101073952143));
#49829=CARTESIAN_POINT('Ctrl Pts',(5.37547264724376,-2.49558406764019,96.3173176366375));
#49830=CARTESIAN_POINT('Ctrl Pts',(4.54925327425696,-4.27525548713001,96.2245278780607));
#49831=CARTESIAN_POINT('Ctrl Pts',(2.75142490963826,-5.60385365620792,96.1317381194839));
#49832=CARTESIAN_POINT('Ctrl Pts',(0.807620326302736,-5.87123457447137,
96.0389483609071));
#49833=CARTESIAN_POINT('Ctrl Pts',(-1.13618425703301,-6.13861549273485,
95.9461586023304));
#49834=CARTESIAN_POINT('Ctrl Pts',(-3.22596505908562,-5.34477916018357,
95.8533688437537));
#49835=CARTESIAN_POINT('Ctrl Pts',(-4.50201338221775,-3.85428612407767,
95.7605790851769));
#49836=CARTESIAN_POINT('Ctrl Pts',(-5.40599855185311,-2.79838285171782,
95.6948444541862));
#49837=CARTESIAN_POINT('Ctrl Pts',(-5.90159849805931,-1.39285078745819,
95.6291098231954));
#49838=CARTESIAN_POINT('Ctrl Pts',(-5.91332833078945,0.00520191486789418,
95.5633751922047));
#49839=CARTESIAN_POINT('Ctrl Pts',(-5.91081306495006,0.00447103847887897,
95.3116248077953));
#49840=CARTESIAN_POINT('Ctrl Pts',(-5.90170944714215,-1.29749896905956,
95.3727760999461));
#49841=CARTESIAN_POINT('Ctrl Pts',(-5.47818989466327,-2.60485132995615,
95.4339273920968));
#49842=CARTESIAN_POINT('Ctrl Pts',(-4.68673601610343,-3.62743061347276,
95.4950786842475));
#49843=CARTESIAN_POINT('Ctrl Pts',(-3.48556412966475,-5.17937636835338,
95.5878866354632));
#49844=CARTESIAN_POINT('Ctrl Pts',(-1.43691235381768,-6.07539132521594,
95.6806945866788));
#49845=CARTESIAN_POINT('Ctrl Pts',(0.518060955814923,-5.90384283211033,
95.7735025378945));
#49846=CARTESIAN_POINT('Ctrl Pts',(2.47303426544775,-5.7322943390047,95.8663104891102));
#49847=CARTESIAN_POINT('Ctrl Pts',(4.33432910886597,-4.49318239593063,95.9591184403261));
#49848=CARTESIAN_POINT('Ctrl Pts',(5.24685961212369,-2.7557597048483,96.0519263915418));
#49849=CARTESIAN_POINT('Ctrl Pts',(6.15939011538146,-1.01833701376587,96.1447343427575));
#49850=CARTESIAN_POINT('Ctrl Pts',(6.12315627847846,1.21739642532511,96.2375422939731));
#49851=CARTESIAN_POINT('Ctrl Pts',(5.15480406280235,2.92433623482607,96.3303502451888));
#49852=CARTESIAN_POINT('Ctrl Pts',(4.18645184712642,4.63127604432674,96.4231581964045));
#49853=CARTESIAN_POINT('Ctrl Pts',(2.28598125267787,5.80942222423782,96.5159661476203));
#49854=CARTESIAN_POINT('Ctrl Pts',(0.326475641240406,5.91752997422717,96.608774098836));
#49855=CARTESIAN_POINT('Ctrl Pts',(-1.63302997019728,6.02563772421653,96.7015820500518));
#49856=CARTESIAN_POINT('Ctrl Pts',(-3.65157059862376,5.0637070442839,96.7943900012675));
#49857=CARTESIAN_POINT('Ctrl Pts',(-4.80182106315389,3.47365251826545,96.8871979524832));
#49858=CARTESIAN_POINT('Ctrl Pts',(-5.52242947626645,2.47751584708868,96.9453402375872));
#49859=CARTESIAN_POINT('Ctrl Pts',(-5.90225427633181,1.23485523424981,97.0034825226912));
#49860=CARTESIAN_POINT('Ctrl Pts',(-5.90944591666731,-0.00376931072489263,
97.0616248077952));
#49861=CARTESIAN_POINT('Origin',(0.,0.,-10.));
#49862=CARTESIAN_POINT('',(-5.92240521329814,-0.00427408358304571,99.0633751922047));
#49863=CARTESIAN_POINT('',(-5.92460418473688,-0.00304573894302621,98.8116248077953));
#49864=CARTESIAN_POINT('',(-5.91675,-7.2459289488551E-16,-10.));
#49865=CARTESIAN_POINT('Ctrl Pts',(-5.92240521329814,-0.00427408358304571,
99.0633751922047));
#49866=CARTESIAN_POINT('Ctrl Pts',(-5.90857090463864,1.69567528425797,98.9831305008731));
#49867=CARTESIAN_POINT('Ctrl Pts',(-5.13791585564116,3.40656874746623,98.9028858095415));
#49868=CARTESIAN_POINT('Ctrl Pts',(-3.84720206766997,4.50806857428337,98.8226411182099));
#49869=CARTESIAN_POINT('Ctrl Pts',(-2.35470432370565,5.78177156081904,98.7298513596331));
#49870=CARTESIAN_POINT('Ctrl Pts',(-0.166830309248996,6.24064760113001,
98.6370616010563));
#49871=CARTESIAN_POINT('Ctrl Pts',(1.71166305624391,5.67396295386347,98.5442718424796));
#49872=CARTESIAN_POINT('Ctrl Pts',(3.59015642173671,5.10727830659696,98.4514820839028));
#49873=CARTESIAN_POINT('Ctrl Pts',(5.15926913826582,3.5150329717531,98.358692325326));
#49874=CARTESIAN_POINT('Ctrl Pts',(5.69840356221848,1.62844799180725,98.2659025667493));
#49875=CARTESIAN_POINT('Ctrl Pts',(6.23753798617111,-0.258136988138488,
98.1731128081725));
#49876=CARTESIAN_POINT('Ctrl Pts',(5.74669411754747,-2.43906161318616,98.0803230495959));
#49877=CARTESIAN_POINT('Ctrl Pts',(4.45128656894101,-3.91276039403012,97.9875332910191));
#49878=CARTESIAN_POINT('Ctrl Pts',(3.1558790203344,-5.38645917487425,97.8947435324424));
#49879=CARTESIAN_POINT('Ctrl Pts',(1.05590779174478,-6.15293211151451,97.8019537738655));
#49880=CARTESIAN_POINT('Ctrl Pts',(-0.884238578620319,-5.86018499332614,
97.7091640152888));
#49881=CARTESIAN_POINT('Ctrl Pts',(-2.82438494898531,-5.56743787513778,
97.616374256712));
#49882=CARTESIAN_POINT('Ctrl Pts',(-4.60470646112579,-4.21547070212091,
97.5235844981354));
#49883=CARTESIAN_POINT('Ctrl Pts',(-5.40761017031105,-2.42515943102177,
97.4307947395586));
#49884=CARTESIAN_POINT('Ctrl Pts',(-5.74628472357815,-1.66998435459344,
97.3916548904407));
#49885=CARTESIAN_POINT('Ctrl Pts',(-5.91105172161379,-0.836816683578498,
97.3525150413227));
#49886=CARTESIAN_POINT('Ctrl Pts',(-5.90792603807066,-0.00247015932851979,
97.3133751922047));
#49887=CARTESIAN_POINT('Ctrl Pts',(-5.90944591666731,-0.00376931072489263,
97.0616248077952));
#49888=CARTESIAN_POINT('Ctrl Pts',(-5.91373372548356,-0.742263589664,97.0962904739069));
#49889=CARTESIAN_POINT('Ctrl Pts',(-5.78555797945132,-1.4793231280736,97.1309561400185));
#49890=CARTESIAN_POINT('Ctrl Pts',(-5.51816833907535,-2.16184308445984,
97.1656218061302));
#49891=CARTESIAN_POINT('Ctrl Pts',(-4.80230484983295,-3.98910578906286,
97.2584297573459));
#49892=CARTESIAN_POINT('Ctrl Pts',(-3.08861757071432,-5.4254528261647,97.3512377085617));
#49893=CARTESIAN_POINT('Ctrl Pts',(-1.16438090368592,-5.8110209474181,97.4440456597775));
#49894=CARTESIAN_POINT('Ctrl Pts',(0.759855763342594,-6.19658906867151,
97.5368536109932));
#49895=CARTESIAN_POINT('Ctrl Pts',(2.89464181828089,-5.53137827407635,97.6296615622089));
#49896=CARTESIAN_POINT('Ctrl Pts',(4.25924849269672,-4.12098891258653,97.7224695134245));
#49897=CARTESIAN_POINT('Ctrl Pts',(5.62385516711231,-2.71059955109695,97.8152774646402));
#49898=CARTESIAN_POINT('Ctrl Pts',(6.21828246100573,-0.555031622713001,
97.9080854158559));
#49899=CARTESIAN_POINT('Ctrl Pts',(5.76944823271977,1.35543883306,98.0008933670716));
#49900=CARTESIAN_POINT('Ctrl Pts',(5.32061400443376,3.26590928883322,98.0937013182874));
#49901=CARTESIAN_POINT('Ctrl Pts',(3.82851825396813,4.93128227199544,98.1865092695031));
#49902=CARTESIAN_POINT('Ctrl Pts',(1.9786353989358,5.586479150438,98.2793172207188));
#49903=CARTESIAN_POINT('Ctrl Pts',(0.128752543903576,6.24167602888052,98.3721251719345));
#49904=CARTESIAN_POINT('Ctrl Pts',(-2.07891741569531,5.88669680260349,98.4649331231502));
#49905=CARTESIAN_POINT('Ctrl Pts',(-3.63016257062835,4.68462026753603,98.5577410743659));
#49906=CARTESIAN_POINT('Ctrl Pts',(-5.04468185925873,3.58849407506693,98.642368985509));
#49907=CARTESIAN_POINT('Ctrl Pts',(-5.91339068653511,1.7880151987318,98.7269968966522));
#49908=CARTESIAN_POINT('Ctrl Pts',(-5.92460418473688,-0.00304573894302621,
98.8116248077953));
#49909=CARTESIAN_POINT('Origin',(0.,0.,-10.));
#49910=CARTESIAN_POINT('',(-5.92153330141852,0.0046063294329908,100.813375192205));
#49911=CARTESIAN_POINT('',(-5.91888098557728,0.00526341932157319,100.561624807795));
#49912=CARTESIAN_POINT('',(-5.91675,-7.2459289488551E-16,-10.));
#49913=CARTESIAN_POINT('Ctrl Pts',(-5.92153330141852,0.0046063294329908,
100.813375192205));
#49914=CARTESIAN_POINT('Ctrl Pts',(-5.92408513419437,0.302357637627171,
100.799325477577));
#49915=CARTESIAN_POINT('Ctrl Pts',(-5.90357534973135,0.599756241770384,
100.785275762949));
#49916=CARTESIAN_POINT('Ctrl Pts',(-5.85878730752478,0.893452463823286,
100.771226048322));
#49917=CARTESIAN_POINT('Ctrl Pts',(-5.5629897248965,2.83313609879042,100.678436289745));
#49918=CARTESIAN_POINT('Ctrl Pts',(-4.20822471714898,4.61132947896263,100.585646531168));
#49919=CARTESIAN_POINT('Ctrl Pts',(-2.41665311565404,5.41141698065534,100.492856772592));
#49920=CARTESIAN_POINT('Ctrl Pts',(-0.625081514159094,6.21150448234805,
100.400067014015));
#49921=CARTESIAN_POINT('Ctrl Pts',(1.60329668108328,6.03348610556126,100.307277255438));
#49922=CARTESIAN_POINT('Ctrl Pts',(3.24512345400804,4.95911481901481,100.214487496861));
#49923=CARTESIAN_POINT('Ctrl Pts',(4.8869502269329,3.8847435324683,100.121697738284));
#49924=CARTESIAN_POINT('Ctrl Pts',(5.94222557754009,1.91401933616202,100.028907979708));
#49925=CARTESIAN_POINT('Ctrl Pts',(5.92632598388641,-0.0480245003946693,
99.936118221131));
#49926=CARTESIAN_POINT('Ctrl Pts',(5.91042639023273,-2.01006833695136,99.8433284625543));
#49927=CARTESIAN_POINT('Ctrl Pts',(4.82335185231836,-3.96343181375821,99.7505387039774));
#49928=CARTESIAN_POINT('Ctrl Pts',(3.16432931681224,-5.01105437953809,99.6577489454007));
#49929=CARTESIAN_POINT('Ctrl Pts',(1.50530678130631,-6.05867694531785,99.5649591868239));
#49930=CARTESIAN_POINT('Ctrl Pts',(-0.725663751791567,-6.20055860007054,
99.4721694282471));
#49931=CARTESIAN_POINT('Ctrl Pts',(-2.50403376395513,-5.37154176460521,
99.3793796696704));
#49932=CARTESIAN_POINT('Ctrl Pts',(-4.2824037761188,-4.54252492913983,99.2865899110937));
#49933=CARTESIAN_POINT('Ctrl Pts',(-5.60817326734847,-2.74260960345641,
99.1938001525169));
#49934=CARTESIAN_POINT('Ctrl Pts',(-5.87249727622737,-0.798386974234585,
99.1010103939402));
#49935=CARTESIAN_POINT('Ctrl Pts',(-5.90823357424942,-0.535530340084027,
99.088465326695));
#49936=CARTESIAN_POINT('Ctrl Pts',(-5.92456800225705,-0.270035952424749,
99.0759202594499));
#49937=CARTESIAN_POINT('Ctrl Pts',(-5.92240521329814,-0.00427408358304571,
99.0633751922047));
#49938=CARTESIAN_POINT('Ctrl Pts',(-5.92460418473688,-0.00304573894302621,
98.8116248077953));
#49939=CARTESIAN_POINT('Ctrl Pts',(-5.92568806904178,-0.176167703608292,
98.8198048478679));
#49940=CARTESIAN_POINT('Ctrl Pts',(-5.91876042483355,-0.349201677025623,
98.8279848879405));
#49941=CARTESIAN_POINT('Ctrl Pts',(-5.90353977625702,-0.521503068400942,
98.8361649280131));
#49942=CARTESIAN_POINT('Ctrl Pts',(-5.73085147668537,-2.4763760254123,98.9289728792288));
#49943=CARTESIAN_POINT('Ctrl Pts',(-4.49065452727481,-4.3369480955771,99.0217808304444));
#49944=CARTESIAN_POINT('Ctrl Pts',(-2.75270008599051,-5.24846544970891,
99.1145887816601));
#49945=CARTESIAN_POINT('Ctrl Pts',(-1.01474564470621,-6.15998280384072,
99.2073967328758));
#49946=CARTESIAN_POINT('Ctrl Pts',(1.22096628845165,-6.12244544193971,99.3002046840917));
#49947=CARTESIAN_POINT('Ctrl Pts',(2.92734121579234,-5.15309816969595,99.3930126353074));
#49948=CARTESIAN_POINT('Ctrl Pts',(4.63371614313303,-4.1837508974522,99.4858205865231));
#49949=CARTESIAN_POINT('Ctrl Pts',(5.81075406465631,-2.28259371486558,99.5786285377386));
#49950=CARTESIAN_POINT('Ctrl Pts',(5.91771931811476,-0.323025404901408,
99.6714364889544));
#49951=CARTESIAN_POINT('Ctrl Pts',(6.02468457157323,1.63654290506288,99.7642444401701));
#49952=CARTESIAN_POINT('Ctrl Pts',(5.06157715696692,3.65452234240463,99.8570523913859));
#49953=CARTESIAN_POINT('Ctrl Pts',(3.47085225448103,4.80384553954062,99.9498603426016));
#49954=CARTESIAN_POINT('Ctrl Pts',(1.88012735199531,5.95316873667648,100.042668293817));
#49955=CARTESIAN_POINT('Ctrl Pts',(-0.338215038369973,6.23383569360659,
100.135476245033));
#49956=CARTESIAN_POINT('Ctrl Pts',(-2.16506005241971,5.5169069513285,100.228284196249));
#49957=CARTESIAN_POINT('Ctrl Pts',(-3.99190506646955,4.79997820905036,100.321092147464));
#49958=CARTESIAN_POINT('Ctrl Pts',(-5.42725270420401,3.08545376756384,100.41390009868));
#49959=CARTESIAN_POINT('Ctrl Pts',(-5.81169884511591,1.16099262438603,100.506708049896));
#49960=CARTESIAN_POINT('Ctrl Pts',(-5.88752760536498,0.781408887926776,
100.525013635862));
#49961=CARTESIAN_POINT('Ctrl Pts',(-5.92247184496295,0.393657724318832,
100.543319221829));
#49962=CARTESIAN_POINT('Ctrl Pts',(-5.91888098557728,0.00526341932157319,
100.561624807795));
#49963=CARTESIAN_POINT('Origin',(0.,0.,-10.));
#49964=CARTESIAN_POINT('',(-5.90756520705438,0.00198423502760892,102.563375192205));
#49965=CARTESIAN_POINT('',(-5.90698748410082,0.000568579071646174,102.311624807795));
#49966=CARTESIAN_POINT('',(-5.91675,-7.2459289488551E-16,-10.));
#49967=CARTESIAN_POINT('Ctrl Pts',(-5.90756520705438,0.00198423502760892,
102.563375192205));
#49968=CARTESIAN_POINT('Ctrl Pts',(-5.91016349010236,0.868537566628739,
102.522730695704));
#49969=CARTESIAN_POINT('Ctrl Pts',(-5.73195451304473,1.73407369185386,102.482086199204));
#49970=CARTESIAN_POINT('Ctrl Pts',(-5.36759759991338,2.51247726861946,102.441441702703));
#49971=CARTESIAN_POINT('Ctrl Pts',(-4.53578535185495,4.28954147613377,102.348651944127));
#49972=CARTESIAN_POINT('Ctrl Pts',(-2.73378751570448,5.61247901132398,102.25586218555));
#49973=CARTESIAN_POINT('Ctrl Pts',(-0.789151648018449,5.87374545723213,
102.163072426973));
#49974=CARTESIAN_POINT('Ctrl Pts',(1.15548421966758,6.13501190314029,102.070282668396));
#49975=CARTESIAN_POINT('Ctrl Pts',(3.24275811888915,5.3346072597664,101.97749290982));
#49976=CARTESIAN_POINT('Ctrl Pts',(4.51411261938045,3.8401084983989,101.884703151243));
#49977=CARTESIAN_POINT('Ctrl Pts',(5.78546711987161,2.34560973703157,101.791913392666));
#49978=CARTESIAN_POINT('Ctrl Pts',(6.24090222163271,0.157016857670822,101.699123634089));
#49979=CARTESIAN_POINT('Ctrl Pts',(5.67126439624579,-1.72058308947875,101.606333875513));
#49980=CARTESIAN_POINT('Ctrl Pts',(5.10162657085884,-3.59818303662842,101.513544116936));
#49981=CARTESIAN_POINT('Ctrl Pts',(3.50691581832374,-5.16479005156688,101.420754358359));
#49982=CARTESIAN_POINT('Ctrl Pts',(1.61948539689627,-5.70095720639658,101.327964599782));
#49983=CARTESIAN_POINT('Ctrl Pts',(-0.267945024531298,-6.23712436122631,
101.235174841205));
#49984=CARTESIAN_POINT('Ctrl Pts',(-2.44809511485127,-5.74285165594717,
101.142385082629));
#49985=CARTESIAN_POINT('Ctrl Pts',(-3.91975508125673,-4.4451283584265,101.049595324052));
#49986=CARTESIAN_POINT('Ctrl Pts',(-5.16858439399879,-3.34389918132894,
100.970855280103));
#49987=CARTESIAN_POINT('Ctrl Pts',(-5.90723184190519,-1.66410735724864,
100.892115236154));
#49988=CARTESIAN_POINT('Ctrl Pts',(-5.92153330141852,0.0046063294329908,
100.813375192205));
#49989=CARTESIAN_POINT('Ctrl Pts',(-5.91888098557728,0.00526341932157319,
100.561624807795));
#49990=CARTESIAN_POINT('Ctrl Pts',(-5.90426645654772,-1.57547234213497,
100.636127173045));
#49991=CARTESIAN_POINT('Ctrl Pts',(-5.25134533554264,-3.16686128469683,
100.710629538294));
#49992=CARTESIAN_POINT('Ctrl Pts',(-4.1185048825022,-4.26165048695995,100.785131903543));
#49993=CARTESIAN_POINT('Ctrl Pts',(-2.70732013488725,-5.6254346102588,100.877939854759));
#49994=CARTESIAN_POINT('Ctrl Pts',(-0.551405995568029,-6.21860501198742,
100.970747805974));
#49995=CARTESIAN_POINT('Ctrl Pts',(1.35880244534019,-5.76865697149153,101.06355575719));
#49996=CARTESIAN_POINT('Ctrl Pts',(3.26901088624852,-5.31870893099562,101.156363708406));
#49997=CARTESIAN_POINT('Ctrl Pts',(4.93351362874569,-3.82564244827511,101.249171659622));
#49998=CARTESIAN_POINT('Ctrl Pts',(5.58763183256818,-1.97537789900341,101.341979610837));
#49999=CARTESIAN_POINT('Ctrl Pts',(6.24175003639059,-0.12511334973192,101.434787562053));
#50000=CARTESIAN_POINT('Ctrl Pts',(5.88548370153838,2.08234926609087,101.527595513269));
#50001=CARTESIAN_POINT('Ctrl Pts',(4.68250292647658,3.63289329374517,101.620403464484));
#50002=CARTESIAN_POINT('Ctrl Pts',(3.47952215141465,5.18343732139964,101.7132114157));
#50003=CARTESIAN_POINT('Ctrl Pts',(1.42982693614302,6.0770627608857,101.806019366916));
#50004=CARTESIAN_POINT('Ctrl Pts',(-0.524945003706648,5.90323471355187,
101.898827318132));
#50005=CARTESIAN_POINT('Ctrl Pts',(-2.47971694355631,5.72940666621803,101.991635269347));
#50006=CARTESIAN_POINT('Ctrl Pts',(-4.33956560798389,4.4881251320643,102.084443220563));
#50007=CARTESIAN_POINT('Ctrl Pts',(-5.25006950312836,2.74963953137896,102.177251171779));
#50008=CARTESIAN_POINT('Ctrl Pts',(-5.68949923371802,1.91060714149341,102.222042383784));
#50009=CARTESIAN_POINT('Ctrl Pts',(-5.90780326507992,0.955763720222844,
102.26683359579));
#50010=CARTESIAN_POINT('Ctrl Pts',(-5.90698748410082,0.000568579071646174,
102.311624807795));
#50011=CARTESIAN_POINT('Origin',(0.,0.,-10.));
#50012=CARTESIAN_POINT('',(-5.91423563825394,-0.00534293135961927,104.313375192205));
#50013=CARTESIAN_POINT('',(-5.9167872280184,-0.00546137831681672,104.061624807795));
#50014=CARTESIAN_POINT('',(-5.91675,-7.2459289488551E-16,-10.));
#50015=CARTESIAN_POINT('Ctrl Pts',(-5.91423563825394,-0.00534293135961927,
104.313375192205));
#50016=CARTESIAN_POINT('Ctrl Pts',(-5.90176787237235,1.42415486201049,104.246135913831));
#50017=CARTESIAN_POINT('Ctrl Pts',(-5.38101863511829,2.86179473551728,104.178896635458));
#50018=CARTESIAN_POINT('Ctrl Pts',(-4.43895915657409,3.92674007622001,104.111657357085));
#50019=CARTESIAN_POINT('Ctrl Pts',(-3.13892331898171,5.39635758925651,104.018867598508));
#50020=CARTESIAN_POINT('Ctrl Pts',(-1.036551963558,6.15622245053065,103.926077839931));
#50021=CARTESIAN_POINT('Ctrl Pts',(0.902664139812632,5.85737513487242,103.833288081355));
#50022=CARTESIAN_POINT('Ctrl Pts',(2.84188024318338,5.55852781921417,103.740498322778));
#50023=CARTESIAN_POINT('Ctrl Pts',(4.61794109450092,4.20096832662347,103.647708564201));
#50024=CARTESIAN_POINT('Ctrl Pts',(5.41521041034822,2.40814082469893,103.554918805624));
#50025=CARTESIAN_POINT('Ctrl Pts',(6.21247972619543,0.615313322774602,103.462129047048));
#50026=CARTESIAN_POINT('Ctrl Pts',(6.03095750657248,-1.61278218848366,103.369339288471));
#50027=CARTESIAN_POINT('Ctrl Pts',(4.95400582123115,-3.25291751250062,103.276549529894));
#50028=CARTESIAN_POINT('Ctrl Pts',(3.87705413588976,-4.89305283651766,103.183759771317));
#50029=CARTESIAN_POINT('Ctrl Pts',(1.90467298483,-5.94522797329356,103.090970012741));
#50030=CARTESIAN_POINT('Ctrl Pts',(-0.0573434243123933,-5.92624313976515,
102.998180254164));
#50031=CARTESIAN_POINT('Ctrl Pts',(-2.01935983345479,-5.90725830623673,
102.905390495587));
#50032=CARTESIAN_POINT('Ctrl Pts',(-3.9710115006797,-4.81711350240401,102.81260073701));
#50033=CARTESIAN_POINT('Ctrl Pts',(-5.01602400430896,-3.1564456605685,102.719810978434));
#50034=CARTESIAN_POINT('Ctrl Pts',(-5.60329194972236,-2.22319654813983,
102.667665716357));
#50035=CARTESIAN_POINT('Ctrl Pts',(-5.90423171390891,-1.10976900268225,
102.615520454281));
#50036=CARTESIAN_POINT('Ctrl Pts',(-5.90756520705438,0.00198423502760892,
102.563375192205));
#50037=CARTESIAN_POINT('Ctrl Pts',(-5.90698748410082,0.000568579071646174,
102.311624807795));
#50038=CARTESIAN_POINT('Ctrl Pts',(-5.90611295669304,-1.023412553249,102.359641547005));
#50039=CARTESIAN_POINT('Ctrl Pts',(-5.65342357388983,-2.04779788585592,
102.407658286216));
#50040=CARTESIAN_POINT('Ctrl Pts',(-5.1513905248428,-2.93034520163755,102.455675025426));
#50041=CARTESIAN_POINT('Ctrl Pts',(-4.18104852555142,-4.63615466675218,
102.548482976641));
#50042=CARTESIAN_POINT('Ctrl Pts',(-2.27920540110728,-5.81208392976454,
102.641290927857));
#50043=CARTESIAN_POINT('Ctrl Pts',(-0.31957505875301,-5.91790665033028,
102.734098879073));
#50044=CARTESIAN_POINT('Ctrl Pts',(1.64005528360104,-6.02372937089601,102.826906830289));
#50045=CARTESIAN_POINT('Ctrl Pts',(3.65747284386519,-5.05944554901537,102.919714781504));
#50046=CARTESIAN_POINT('Ctrl Pts',(4.80586838290561,-3.46805081081413,103.01252273272));
#50047=CARTESIAN_POINT('Ctrl Pts',(5.95426392194624,-1.87665607261261,103.105330683936));
#50048=CARTESIAN_POINT('Ctrl Pts',(6.23363743976279,0.341849581909771,103.198138635151));
#50049=CARTESIAN_POINT('Ctrl Pts',(5.51564368816192,2.16827628438813,103.290946586367));
#50050=CARTESIAN_POINT('Ctrl Pts',(4.79764993656108,3.99470298686638,103.383754537583));
#50051=CARTESIAN_POINT('Ctrl Pts',(3.08228891554294,5.42905073730067,103.476562488799));
#50052=CARTESIAN_POINT('Ctrl Pts',(1.15760395041781,5.8123747671823,103.569370440014));
#50053=CARTESIAN_POINT('Ctrl Pts',(-0.767081014707224,6.19569879706391,
103.66217839123));
#50054=CARTESIAN_POINT('Ctrl Pts',(-2.90108992393922,5.52799910639299,103.754986342446));
#50055=CARTESIAN_POINT('Ctrl Pts',(-4.26405103251585,4.11601945237153,103.847794293661));
#50056=CARTESIAN_POINT('Ctrl Pts',(-5.31081003241397,3.03161403447703,103.919071131706));
#50057=CARTESIAN_POINT('Ctrl Pts',(-5.90278230389148,1.50821034789738,103.990347969751));
#50058=CARTESIAN_POINT('Ctrl Pts',(-5.9167872280184,-0.00546137831681672,
104.061624807795));
#50059=CARTESIAN_POINT('Origin',(0.,0.,-10.));
#50060=CARTESIAN_POINT('',(-5.92648446538136,0.00041551144474657,106.063375192205));
#50061=CARTESIAN_POINT('',(-5.9257749495935,0.00192492296004073,105.811624807795));
#50062=CARTESIAN_POINT('',(-5.91675,-7.2459289488551E-16,-10.));
#50063=CARTESIAN_POINT('Ctrl Pts',(-5.92648446538136,0.00041551144474657,
106.063375192205));
#50064=CARTESIAN_POINT('Ctrl Pts',(-5.92650674114986,0.0224984077431825,
106.062330890535));
#50065=CARTESIAN_POINT('Ctrl Pts',(-5.9263940289506,0.0445810701819271,
106.061286588866));
#50066=CARTESIAN_POINT('Ctrl Pts',(-5.92614564199684,0.0666622064383869,
106.060242287197));
#50067=CARTESIAN_POINT('Ctrl Pts',(-5.90407561553706,2.0286463367465,105.96745252862));
#50068=CARTESIAN_POINT('Ctrl Pts',(-4.8108632413548,3.97858136859802,105.874662770043));
#50069=CARTESIAN_POINT('Ctrl Pts',(-3.14855419947414,5.02098122610502,105.781873011467));
#50070=CARTESIAN_POINT('Ctrl Pts',(-1.48624515759367,6.06338108361191,105.68908325289));
#50071=CARTESIAN_POINT('Ctrl Pts',(0.745160551985173,6.19824576677453,105.596293494313));
#50072=CARTESIAN_POINT('Ctrl Pts',(2.52091456075547,5.36364016292073,105.503503735736));
#50073=CARTESIAN_POINT('Ctrl Pts',(4.29666856952576,4.52903455906694,105.410713977159));
#50074=CARTESIAN_POINT('Ctrl Pts',(5.61677087748763,2.72495866819665,105.317924218583));
#50075=CARTESIAN_POINT('Ctrl Pts',(5.87497911439927,0.779914370490588,105.225134460006));
#50076=CARTESIAN_POINT('Ctrl Pts',(6.13318735131092,-1.16512992721559,105.132344701429));
#50077=CARTESIAN_POINT('Ctrl Pts',(5.32950151717242,-3.25114263175742,105.039554942853));
#50078=CARTESIAN_POINT('Ctrl Pts',(3.83300543380504,-4.52014550256365,104.946765184276));
#50079=CARTESIAN_POINT('Ctrl Pts',(2.33650935043775,-5.7891483733698,104.853975425699));
#50080=CARTESIAN_POINT('Ctrl Pts',(0.147203017841625,-6.2411414104402,104.761185667122));
#50081=CARTESIAN_POINT('Ctrl Pts',(-1.72949886827872,-5.6685518154594,104.668395908546));
#50082=CARTESIAN_POINT('Ctrl Pts',(-3.60620075439917,-5.09596222047856,
104.575606149969));
#50083=CARTESIAN_POINT('Ctrl Pts',(-5.1702981940439,-3.49878999344632,104.482816391392));
#50084=CARTESIAN_POINT('Ctrl Pts',(-5.7034967539857,-1.61051879753076,104.390026632815));
#50085=CARTESIAN_POINT('Ctrl Pts',(-5.85031769046941,-1.09056663308795,
104.364476152612));
#50086=CARTESIAN_POINT('Ctrl Pts',(-5.91897330666809,-0.548542619906705,
104.338925672408));
#50087=CARTESIAN_POINT('Ctrl Pts',(-5.91423563825394,-0.00534293135961927,
104.313375192205));
#50088=CARTESIAN_POINT('Ctrl Pts',(-5.9167872280184,-0.00546137831681672,
104.061624807795));
#50089=CARTESIAN_POINT('Ctrl Pts',(-5.92101779736746,-0.462707212097632,
104.083155920966));
#50090=CARTESIAN_POINT('Ctrl Pts',(-5.87250845240857,-0.919064997863135,
104.104687034137));
#50091=CARTESIAN_POINT('Ctrl Pts',(-5.76786374926362,-1.36216559570815,
104.126218147308));
#50092=CARTESIAN_POINT('Ctrl Pts',(-5.31680204951344,-3.27211137239461,
104.219026098524));
#50093=CARTESIAN_POINT('Ctrl Pts',(-3.8227653420916,-4.93574330839516,104.31183404974));
#50094=CARTESIAN_POINT('Ctrl Pts',(-1.9721197275602,-5.58878261523637,104.404642000956));
#50095=CARTESIAN_POINT('Ctrl Pts',(-0.121474113029111,-6.24182192207747,
104.497449952171));
#50096=CARTESIAN_POINT('Ctrl Pts',(2.08578040861131,-5.88426859975954,104.590257903387));
#50097=CARTESIAN_POINT('Ctrl Pts',(3.6356227818944,-4.68038399364526,104.683065854603));
#50098=CARTESIAN_POINT('Ctrl Pts',(5.18546515517775,-3.47649938753077,104.775873805818));
#50099=CARTESIAN_POINT('Ctrl Pts',(6.07789538010348,-1.42628349761935,104.868681757034));
#50100=CARTESIAN_POINT('Ctrl Pts',(5.90292764409852,0.528386760562654,104.96148970825));
#50101=CARTESIAN_POINT('Ctrl Pts',(5.72795990809357,2.48305701874455,105.054297659466));
#50102=CARTESIAN_POINT('Ctrl Pts',(4.4855942111583,4.34218164519717,105.147105610681));
#50103=CARTESIAN_POINT('Ctrl Pts',(2.74657804205345,5.25167177183706,105.239913561897));
#50104=CARTESIAN_POINT('Ctrl Pts',(1.0075618729488,6.16116189847685,105.332721513113));
#50105=CARTESIAN_POINT('Ctrl Pts',(-1.22810476832518,6.1210175253041,105.425529464328));
#50106=CARTESIAN_POINT('Ctrl Pts',(-2.93334819133995,5.14968112882371,105.518337415544));
#50107=CARTESIAN_POINT('Ctrl Pts',(-4.63859161435491,4.1783447323432,105.61114536676));
#50108=CARTESIAN_POINT('Ctrl Pts',(-5.81341181911044,2.27581631255488,105.703953317976));
#50109=CARTESIAN_POINT('Ctrl Pts',(-5.91809197081005,0.316124603968129,
105.796761269191));
#50110=CARTESIAN_POINT('Ctrl Pts',(-5.92368027603418,0.21150729844301,105.801715782059));
#50111=CARTESIAN_POINT('Ctrl Pts',(-5.92621877557426,0.106727082537521,
105.806670294927));
#50112=CARTESIAN_POINT('Ctrl Pts',(-5.9257749495935,0.00192492296004073,
105.811624807795));
#50113=CARTESIAN_POINT('Origin',(0.,0.,-10.));
#50114=CARTESIAN_POINT('',(-5.91298589814417,0.00513333739083355,107.813375192205));
#50115=CARTESIAN_POINT('',(-5.91092078228077,0.00451530674276642,107.561624807795));
#50116=CARTESIAN_POINT('',(-5.91675,-7.2459289488551E-16,-10.));
#50117=CARTESIAN_POINT('Ctrl Pts',(-5.91298589814417,0.00513333739083355,
107.813375192205));
#50118=CARTESIAN_POINT('Ctrl Pts',(-5.91783226872518,0.593051106927172,
107.785736108663));
#50119=CARTESIAN_POINT('Ctrl Pts',(-5.83726005077582,1.17967014789196,107.758097025121));
#50120=CARTESIAN_POINT('Ctrl Pts',(-5.66582521821169,1.73841037059773,107.730457941578));
#50121=CARTESIAN_POINT('Ctrl Pts',(-5.09028526946242,3.61420955522335,107.637668183002));
#50122=CARTESIAN_POINT('Ctrl Pts',(-3.49065551721405,5.17579355207652,107.544878424425));
#50123=CARTESIAN_POINT('Ctrl Pts',(-1.60154821588312,5.70602219870611,107.452088665848));
#50124=CARTESIAN_POINT('Ctrl Pts',(0.2875590854477,6.23625084533567,107.359298907272));
#50125=CARTESIAN_POINT('Ctrl Pts',(2.46614393586105,5.73512414174176,107.266509148695));
#50126=CARTESIAN_POINT('Ctrl Pts',(3.93371536164864,4.43277897863799,107.173719390118));
#50127=CARTESIAN_POINT('Ctrl Pts',(5.40128678743632,3.13043381553414,107.080929631541));
#50128=CARTESIAN_POINT('Ctrl Pts',(6.15784478859817,1.02687019292034,106.988139872964));
#50129=CARTESIAN_POINT('Ctrl Pts',(5.85594847886084,-0.91187358381125,106.895350114388));
#50130=CARTESIAN_POINT('Ctrl Pts',(5.55405216912353,-2.85061736054273,106.802560355811));
#50131=CARTESIAN_POINT('Ctrl Pts',(4.19370154848718,-4.624541291392,106.709770597234));
#50132=CARTESIAN_POINT('Ctrl Pts',(2.39962257920517,-5.41899045000949,106.616980838657));
#50133=CARTESIAN_POINT('Ctrl Pts',(0.605543609923058,-6.21343960862703,
106.524191080081));
#50134=CARTESIAN_POINT('Ctrl Pts',(-1.62226370800443,-6.02841399501274,
106.431401321504));
#50135=CARTESIAN_POINT('Ctrl Pts',(-3.26070352759948,-4.94888457382324,
106.338611562927));
#50136=CARTESIAN_POINT('Ctrl Pts',(-4.88070353805124,-3.8815047087256,106.24686610602));
#50137=CARTESIAN_POINT('Ctrl Pts',(-5.92452746328279,-1.93964210828605,
106.155120649112));
#50138=CARTESIAN_POINT('Ctrl Pts',(-5.92648446538136,0.00041551144474657,
106.063375192205));
#50139=CARTESIAN_POINT('Ctrl Pts',(-5.9257749495935,0.00192492296004073,
105.811624807795));
#50140=CARTESIAN_POINT('Ctrl Pts',(-5.9179050258539,-1.8564273127613,105.899478246143));
#50141=CARTESIAN_POINT('Ctrl Pts',(-4.9723205622003,-3.7216791642822,105.987331684491));
#50142=CARTESIAN_POINT('Ctrl Pts',(-3.46524818821572,-4.80788959256222,
106.075185122838));
#50143=CARTESIAN_POINT('Ctrl Pts',(-1.87318415527777,-5.95535708312111,
106.167993074054));
#50144=CARTESIAN_POINT('Ctrl Pts',(0.345484009241598,-6.23343706685349,
106.26080102527));
#50145=CARTESIAN_POINT('Ctrl Pts',(2.17149177927208,-5.5143785500049,106.353608976486));
#50146=CARTESIAN_POINT('Ctrl Pts',(3.99749954930236,-4.79532003315639,106.446416927701));
#50147=CARTESIAN_POINT('Ctrl Pts',(5.43084692484366,-3.07912301572704,106.539224878917));
#50148=CARTESIAN_POINT('Ctrl Pts',(5.81304871338755,-1.15421488293286,106.632032830133));
#50149=CARTESIAN_POINT('Ctrl Pts',(6.1952505019314,0.770693249861093,106.724840781348));
#50150=CARTESIAN_POINT('Ctrl Pts',(5.52630670347817,2.90431249801998,106.817648732564));
#50151=CARTESIAN_POINT('Ctrl Pts',(4.11353262303918,4.26645012854864,106.91045668378));
#50152=CARTESIAN_POINT('Ctrl Pts',(2.70075854260003,5.62858775907746,107.003264634996));
#50153=CARTESIAN_POINT('Ctrl Pts',(0.544154180174869,6.21924377197597,107.096072586211));
#50154=CARTESIAN_POINT('Ctrl Pts',(-1.36552828302161,5.76706856630545,107.188880537427));
#50155=CARTESIAN_POINT('Ctrl Pts',(-3.27521074621809,5.31489336063493,107.281688488643));
#50156=CARTESIAN_POINT('Ctrl Pts',(-4.93797131018577,3.81988693639561,107.374496439858));
#50157=CARTESIAN_POINT('Ctrl Pts',(-5.58993149805126,1.96886088571407,107.467304391074));
#50158=CARTESIAN_POINT('Ctrl Pts',(-5.81079316561159,1.3417969823343,107.498744529981));
#50159=CARTESIAN_POINT('Ctrl Pts',(-5.91565324474178,0.673875513844714,
107.530184668888));
#50160=CARTESIAN_POINT('Ctrl Pts',(-5.91092078228077,0.00451530674276642,
107.561624807795));
#50161=CARTESIAN_POINT('Origin',(0.,0.,-10.));
#50162=CARTESIAN_POINT('',(-5.90808735901173,-0.00265285794674774,109.563375192205));
#50163=CARTESIAN_POINT('',(-5.90935748219384,-0.00371301381819065,109.311624807795));
#50164=CARTESIAN_POINT('',(-5.91675,-7.2459289488551E-16,-10.));
#50165=CARTESIAN_POINT('Ctrl Pts',(-5.90808735901173,-0.00265285794674774,
109.563375192205));
#50166=CARTESIAN_POINT('Ctrl Pts',(-5.90342863114805,1.15337485265749,109.50914132679));
#50167=CARTESIAN_POINT('Ctrl Pts',(-5.57622077201164,2.31183763756103,109.454907461375));
#50168=CARTESIAN_POINT('Ctrl Pts',(-4.94375108945386,3.26848148005295,109.40067359596));
#50169=CARTESIAN_POINT('Ctrl Pts',(-3.86164660173687,4.90522174390387,109.307883837383));
#50170=CARTESIAN_POINT('Ctrl Pts',(-1.8859661764013,5.95118865564213,109.215094078807));
#50171=CARTESIAN_POINT('Ctrl Pts',(0.0759808237317083,5.92603349082254,
109.12230432023));
#50172=CARTESIAN_POINT('Ctrl Pts',(2.03792782386472,5.90087832600295,109.029514561653));
#50173=CARTESIAN_POINT('Ctrl Pts',(3.98614139879518,4.8046010846255,108.936724803076));
#50174=CARTESIAN_POINT('Ctrl Pts',(5.02592603266835,3.14065495304274,108.843935044499));
#50175=CARTESIAN_POINT('Ctrl Pts',(6.06571066654153,1.47670882145997,108.751145285923));
#50176=CARTESIAN_POINT('Ctrl Pts',(6.19706635935743,-0.754906200328122,
108.658355527346));
#50177=CARTESIAN_POINT('Ctrl Pts',(5.35966946341301,-2.52934561949991,108.565565768769));
#50178=CARTESIAN_POINT('Ctrl Pts',(4.5222725674686,-4.30378503867169,108.472776010193));
#50179=CARTESIAN_POINT('Ctrl Pts',(2.71612308276388,-5.62104885522717,108.379986251616));
#50180=CARTESIAN_POINT('Ctrl Pts',(0.770675164491407,-5.8761982446784,108.287196493039));
#50181=CARTESIAN_POINT('Ctrl Pts',(-1.17477275378118,-6.13134763412965,
108.194406734462));
#50182=CARTESIAN_POINT('Ctrl Pts',(-3.25951910562152,-5.32438259647652,
108.101616975886));
#50183=CARTESIAN_POINT('Ctrl Pts',(-4.52616720891648,-3.82589289145091,
108.008827217309));
#50184=CARTESIAN_POINT('Ctrl Pts',(-5.41552159701752,-2.77375505520261,
107.943676542274));
#50185=CARTESIAN_POINT('Ctrl Pts',(-5.90156206369103,-1.38070275561479,
107.878525867239));
#50186=CARTESIAN_POINT('Ctrl Pts',(-5.91298589814417,0.00513333739083355,
107.813375192205));
#50187=CARTESIAN_POINT('Ctrl Pts',(-5.91092078228077,0.00451530674276642,
107.561624807795));
#50188=CARTESIAN_POINT('Ctrl Pts',(-5.90168351812861,-1.30200473369831,
107.622992620104));
#50189=CARTESIAN_POINT('Ctrl Pts',(-5.4749107893125,-2.61400620915615,107.684360432413));
#50190=CARTESIAN_POINT('Ctrl Pts',(-4.67826346976177,-3.63835103414898,
107.745728244721));
#50191=CARTESIAN_POINT('Ctrl Pts',(-3.47347544184374,-5.18749122620678,
107.838536195937));
#50192=CARTESIAN_POINT('Ctrl Pts',(-1.4227395742447,-6.07872593319865,107.931344147153));
#50193=CARTESIAN_POINT('Ctrl Pts',(0.53182833779797,-5.90261856800144,108.024152098368));
#50194=CARTESIAN_POINT('Ctrl Pts',(2.48639624984053,-5.72651120280424,108.116960049584));
#50195=CARTESIAN_POINT('Ctrl Pts',(4.3447962063266,-4.48306176541808,108.2097680008));
#50196=CARTESIAN_POINT('Ctrl Pts',(5.25327225528971,-2.74351561905591,108.302575952015));
#50197=CARTESIAN_POINT('Ctrl Pts',(6.16174830425282,-1.00396947269373,108.395383903231));
#50198=CARTESIAN_POINT('Ctrl Pts',(6.12030044569285,1.23167338264468,108.488191854447));
#50199=CARTESIAN_POINT('Ctrl Pts',(5.14796998221979,2.93635018387868,108.580999805663));
#50200=CARTESIAN_POINT('Ctrl Pts',(4.17563951874667,4.64102698511278,108.673807756878));
#50201=CARTESIAN_POINT('Ctrl Pts',(2.27242645036048,5.81473773224261,108.766615708094));
#50202=CARTESIAN_POINT('Ctrl Pts',(0.312674041719707,5.91827527949106,108.85942365931));
#50203=CARTESIAN_POINT('Ctrl Pts',(-1.64707836692096,6.02181282673951,108.952231610525));
#50204=CARTESIAN_POINT('Ctrl Pts',(-3.66337011581607,5.05517717410668,109.045039561741));
#50205=CARTESIAN_POINT('Ctrl Pts',(-4.80990916782254,3.4624443876396,109.137847512957));
#50206=CARTESIAN_POINT('Ctrl Pts',(-5.52551759100319,2.4683456730104,109.195773277903));
#50207=CARTESIAN_POINT('Ctrl Pts',(-5.90230606863383,1.23034521762944,109.253699042849));
#50208=CARTESIAN_POINT('Ctrl Pts',(-5.90935748219384,-0.00371301381819065,
109.311624807795));
#50209=CARTESIAN_POINT('Origin',(0.,0.,-10.));
#50210=CARTESIAN_POINT('',(-5.92273005567057,-0.00413167202517661,111.313375192205));
#50211=CARTESIAN_POINT('',(-5.92451012806985,-0.0031152991902449,111.061624807795));
#50212=CARTESIAN_POINT('',(-5.91675,-7.2459289488551E-16,-10.));
#50213=CARTESIAN_POINT('Ctrl Pts',(-5.92273005567057,-0.00413167202517661,
111.313375192205));
#50214=CARTESIAN_POINT('Ctrl Pts',(-5.9091339542178,1.70794336761187,111.232546544917));
#50215=CARTESIAN_POINT('Ctrl Pts',(-5.12583041727858,3.43086149514118,111.151717897629));
#50216=CARTESIAN_POINT('Ctrl Pts',(-3.81877088892424,4.53217772354859,111.070889250342));
#50217=CARTESIAN_POINT('Ctrl Pts',(-2.31829126751189,5.79646792732884,110.978099491765));
#50218=CARTESIAN_POINT('Ctrl Pts',(-0.127574270496055,6.24157349064171,
110.885309733188));
#50219=CARTESIAN_POINT('Ctrl Pts',(1.7473175744012,5.66308461124448,110.792519974611));
#50220=CARTESIAN_POINT('Ctrl Pts',(3.62220941929823,5.08459573184732,110.699730216035));
#50221=CARTESIAN_POINT('Ctrl Pts',(5.18127611207678,3.48251240974035,110.606940457458));
#50222=CARTESIAN_POINT('Ctrl Pts',(5.70853353431331,1.59257367413433,110.514150698881));
#50223=CARTESIAN_POINT('Ctrl Pts',(6.23579095654991,-0.297365061471903,
110.421360940304));
#50224=CARTESIAN_POINT('Ctrl Pts',(5.73123910824425,-2.47515921057725,110.328571181728));
#50225=CARTESIAN_POINT('Ctrl Pts',(4.42658783989949,-3.94068092029528,110.235781423151));
#50226=CARTESIAN_POINT('Ctrl Pts',(3.12193657155488,-5.40620263001315,110.142991664574));
#50227=CARTESIAN_POINT('Ctrl Pts',(1.01718588317135,-6.15945190034387,110.050201905997));
#50228=CARTESIAN_POINT('Ctrl Pts',(-0.921080773046223,-5.85450734301785,
109.957412147421));
#50229=CARTESIAN_POINT('Ctrl Pts',(-2.85934742926401,-5.54956278569179,
109.864622388844));
#50230=CARTESIAN_POINT('Ctrl Pts',(-4.63113005331579,-4.18642440070869,
109.771832630267));
#50231=CARTESIAN_POINT('Ctrl Pts',(-5.42275709029251,-2.39109840023526,
109.67904287169));
#50232=CARTESIAN_POINT('Ctrl Pts',(-5.75169304109037,-1.64510661701725,
109.640486978528));
#50233=CARTESIAN_POINT('Ctrl Pts',(-5.91139933783546,-0.824495088097872,
109.601931085367));
#50234=CARTESIAN_POINT('Ctrl Pts',(-5.90808735901173,-0.00265285794674774,
109.563375192205));
#50235=CARTESIAN_POINT('Ctrl Pts',(-5.90935748219384,-0.00371301381819065,
109.311624807795));
#50236=CARTESIAN_POINT('Ctrl Pts',(-5.91360375708538,-0.746847768048513,
109.346506994065));
#50237=CARTESIAN_POINT('Ctrl Pts',(-5.78377224693165,-1.48855295325666,
109.381389180334));
#50238=CARTESIAN_POINT('Ctrl Pts',(-5.51311153728789,-2.17470653597755,
109.416271366604));
#50239=CARTESIAN_POINT('Ctrl Pts',(-4.79298849962897,-4.00029475282613,
109.50907931782));
#50240=CARTESIAN_POINT('Ctrl Pts',(-3.07595606919342,-5.4326412662218,109.601887269035));
#50241=CARTESIAN_POINT('Ctrl Pts',(-1.15082542308427,-5.81372068350237,
109.694695220251));
#50242=CARTESIAN_POINT('Ctrl Pts',(0.774305223024769,-6.19480010078292,
109.787503171467));
#50243=CARTESIAN_POINT('Ctrl Pts',(2.90753408480728,-5.52461242194847,109.880311122683));
#50244=CARTESIAN_POINT('Ctrl Pts',(4.26884777424252,-4.11104439535077,109.973119073898));
#50245=CARTESIAN_POINT('Ctrl Pts',(5.63016146367777,-2.69747636875307,110.065927025114));
#50246=CARTESIAN_POINT('Ctrl Pts',(6.21955998076569,-0.540527994391874,
110.15873497633));
#50247=CARTESIAN_POINT('Ctrl Pts',(5.76627142288757,1.36889050613647,110.251542927545));
#50248=CARTESIAN_POINT('Ctrl Pts',(5.31298286500946,3.2783090066647,110.344350878761));
#50249=CARTESIAN_POINT('Ctrl Pts',(3.81700723216561,4.94019763336027,110.437158829977));
#50250=CARTESIAN_POINT('Ctrl Pts',(1.96560137457252,5.59107848062241,110.529966781192));
#50251=CARTESIAN_POINT('Ctrl Pts',(0.114195516979119,6.24195932788466,110.622774732408));
#50252=CARTESIAN_POINT('Ctrl Pts',(-2.09264056536353,5.88183239571303,110.715582683624));
#50253=CARTESIAN_POINT('Ctrl Pts',(-3.64107804958066,4.67614135554757,110.80839063484));
#50254=CARTESIAN_POINT('Ctrl Pts',(-5.04942464256389,3.57953210530978,110.892802025825));
#50255=CARTESIAN_POINT('Ctrl Pts',(-5.91311730723571,1.78343805305531,110.97721341681));
#50256=CARTESIAN_POINT('Ctrl Pts',(-5.92451012806985,-0.0031152991902449,
111.061624807795));
#50257=CARTESIAN_POINT('Origin',(0.,0.,-10.));
#50258=CARTESIAN_POINT('',(-5.92118311221449,0.004721389953629,113.063375192205));
#50259=CARTESIAN_POINT('',(-5.91902054661466,0.0052408541572496,112.811624807795));
#50260=CARTESIAN_POINT('',(-5.91675,-7.2459289488551E-16,-10.));
#50261=CARTESIAN_POINT('Ctrl Pts',(-5.92118311221449,0.004721389953629,
113.063375192205));
#50262=CARTESIAN_POINT('Ctrl Pts',(-5.9238846454292,0.314895936846653,113.048741521621));
#50263=CARTESIAN_POINT('Ctrl Pts',(-5.901624485963,0.624681876463416,113.034107851037));
#50264=CARTESIAN_POINT('Ctrl Pts',(-5.85305173090669,0.930285684752532,
113.019474180454));
#50265=CARTESIAN_POINT('Ctrl Pts',(-5.5450596800191,2.86807042776155,112.926684421877));
#50266=CARTESIAN_POINT('Ctrl Pts',(-4.17913690128139,4.63770736398083,112.8338946633));
#50267=CARTESIAN_POINT('Ctrl Pts',(-2.38256830886638,5.42651032188376,112.741104904723));
#50268=CARTESIAN_POINT('Ctrl Pts',(-0.585999716451469,6.21531327978665,
112.648315146147));
#50269=CARTESIAN_POINT('Ctrl Pts',(1.64121468964069,6.02328225937329,112.55552538757));
#50270=CARTESIAN_POINT('Ctrl Pts',(3.27625135062814,4.9386053808168,112.462735628993));
#50271=CARTESIAN_POINT('Ctrl Pts',(4.91128801161559,3.85392850226031,112.369945870416));
#50272=CARTESIAN_POINT('Ctrl Pts',(5.95414692749833,1.87660576556068,112.27715611184));
#50273=CARTESIAN_POINT('Ctrl Pts',(5.92590668651959,-0.0852992531488124,
112.184366353263));
#50274=CARTESIAN_POINT('Ctrl Pts',(5.89766644554085,-2.04720427185831,112.091576594686));
#50275=CARTESIAN_POINT('Ctrl Pts',(4.79832704770064,-3.99369157257767,111.998786836109));
#50276=CARTESIAN_POINT('Ctrl Pts',(3.13274794080624,-5.03085841177226,111.905997077533));
#50277=CARTESIAN_POINT('Ctrl Pts',(1.46716883391174,-6.0680252509669,111.813207318956));
#50278=CARTESIAN_POINT('Ctrl Pts',(-0.764649982037001,-6.19587162863665,
111.720417560379));
#50279=CARTESIAN_POINT('Ctrl Pts',(-2.53777042400616,-5.35568551120816,
111.627627801802));
#50280=CARTESIAN_POINT('Ctrl Pts',(-4.31089086597521,-4.51549939377971,
111.534838043225));
#50281=CARTESIAN_POINT('Ctrl Pts',(-5.62531293396473,-2.70728078125311,
111.442048284649));
#50282=CARTESIAN_POINT('Ctrl Pts',(-5.87740284505506,-0.761434052866085,
111.349258526072));
#50283=CARTESIAN_POINT('Ctrl Pts',(-5.90989862398217,-0.510603685088854,
111.337297414783));
#50284=CARTESIAN_POINT('Ctrl Pts',(-5.92474202157661,-0.257486401710428,
111.325336303494));
#50285=CARTESIAN_POINT('Ctrl Pts',(-5.92273005567057,-0.00413167202517661,
111.313375192205));
#50286=CARTESIAN_POINT('Ctrl Pts',(-5.92451012806985,-0.0031152991902449,
111.061624807795));
#50287=CARTESIAN_POINT('Ctrl Pts',(-5.92564339344094,-0.180827129928352,
111.070021368026));
#50288=CARTESIAN_POINT('Ctrl Pts',(-5.91834344502106,-0.358444558721565,
111.078417928256));
#50289=CARTESIAN_POINT('Ctrl Pts',(-5.90230748536562,-0.535269734243664,
111.086814488487));
#50290=CARTESIAN_POINT('Ctrl Pts',(-5.72506055084205,-2.48973463571031,
111.179622439702));
#50291=CARTESIAN_POINT('Ctrl Pts',(-4.48052779570348,-4.34740929048461,
111.272430390918));
#50292=CARTESIAN_POINT('Ctrl Pts',(-2.74045226342587,-5.25487095294303,
111.365238342134));
#50293=CARTESIAN_POINT('Ctrl Pts',(-1.00037673114817,-6.1623326154015,111.45804629335));
#50294=CARTESIAN_POINT('Ctrl Pts',(1.23524157826863,-6.11958128554399,111.550854244565));
#50295=CARTESIAN_POINT('Ctrl Pts',(2.93935117823326,-5.14625708561272,111.643662195781));
#50296=CARTESIAN_POINT('Ctrl Pts',(4.64346077819779,-4.1729328856815,111.736470146997));
#50297=CARTESIAN_POINT('Ctrl Pts',(5.8160616687102,-2.26903581567664,111.829278098212));
#50298=CARTESIAN_POINT('Ctrl Pts',(5.918456576311,-0.309223373181075,111.922086049428));
#50299=CARTESIAN_POINT('Ctrl Pts',(6.0208514839118,1.6505890693146,112.014894000644));
#50300=CARTESIAN_POINT('Ctrl Pts',(5.05304040860088,3.66631688430099,112.10770195186));
#50301=CARTESIAN_POINT('Ctrl Pts',(3.45963941003865,4.81192710800027,112.200509903075));
#50302=CARTESIAN_POINT('Ctrl Pts',(1.86623841147642,5.95753733169955,112.293317854291));
#50303=CARTESIAN_POINT('Ctrl Pts',(-0.352752510337116,6.23302996411172,
112.386125805507));
#50304=CARTESIAN_POINT('Ctrl Pts',(-2.17792055341265,5.51184265044123,112.478933756722));
#50305=CARTESIAN_POINT('Ctrl Pts',(-4.00308859648809,4.79065533677078,112.571741707938));
#50306=CARTESIAN_POINT('Ctrl Pts',(-5.43443376082557,3.07278807701779,112.664549659154));
#50307=CARTESIAN_POINT('Ctrl Pts',(-5.81439067729846,1.14743557202359,112.75735761037));
#50308=CARTESIAN_POINT('Ctrl Pts',(-5.88844753963049,0.772167852918489,
112.775446676178));
#50309=CARTESIAN_POINT('Ctrl Pts',(-5.92256284181212,0.389017903419475,
112.793535741987));
#50310=CARTESIAN_POINT('Ctrl Pts',(-5.91902054661466,0.00524085415724961,
112.811624807795));
#50311=CARTESIAN_POINT('Origin',(0.,0.,-10.));
#50312=CARTESIAN_POINT('',(-5.90744685829511,0.00179048289942529,114.813375192205));
#50313=CARTESIAN_POINT('',(-5.90700152101349,0.000644589703395199,114.561624807795));
#50314=CARTESIAN_POINT('',(-5.91675,-7.2459289488551E-16,-10.));
#50315=CARTESIAN_POINT('Ctrl Pts',(-5.90744685829511,0.00179048289942529,
114.813375192205));
#50316=CARTESIAN_POINT('Ctrl Pts',(-5.90982243185645,0.880837885823255,
114.772146739748));
#50317=CARTESIAN_POINT('Ctrl Pts',(-5.72623916706124,1.7589420329495,114.730918287292));
#50318=CARTESIAN_POINT('Ctrl Pts',(-5.35168831615744,2.54618895344184,114.689689834835));
#50319=CARTESIAN_POINT('Ctrl Pts',(-4.50871505474855,4.31798603386546,114.596900076258));
#50320=CARTESIAN_POINT('Ctrl Pts',(-2.69843178552914,5.62956310315636,114.504110317682));
#50321=CARTESIAN_POINT('Ctrl Pts',(-0.752191058465522,5.87859291255057,
114.411320559105));
#50322=CARTESIAN_POINT('Ctrl Pts',(1.19404966859809,6.1276227219448,114.318530800528));
#50323=CARTESIAN_POINT('Ctrl Pts',(3.27624785350592,5.31410527144234,114.225741041951));
#50324=CARTESIAN_POINT('Ctrl Pts',(4.5381770315982,3.81163944383515,114.132951283375));
#50325=CARTESIAN_POINT('Ctrl Pts',(5.80010620969055,2.30917361622787,114.040161524798));
#50326=CARTESIAN_POINT('Ctrl Pts',(6.24176638096727,0.117759411515774,113.947371766221));
#50327=CARTESIAN_POINT('Ctrl Pts',(5.66033000133476,-1.75622045766327,113.854582007644));
#50328=CARTESIAN_POINT('Ctrl Pts',(5.07889362170229,-3.63020032684221,113.761792249068));
#50329=CARTESIAN_POINT('Ctrl Pts',(3.4743606911607,-5.18674586048813,113.669002490491));
#50330=CARTESIAN_POINT('Ctrl Pts',(1.58359519447514,-5.71103075459768,113.576212731914));
#50331=CARTESIAN_POINT('Ctrl Pts',(-0.307170302210411,-6.23531564870724,
113.483422973337));
#50332=CARTESIAN_POINT('Ctrl Pts',(-2.48416836503994,-5.72733990328042,
113.390633214761));
#50333=CARTESIAN_POINT('Ctrl Pts',(-3.9476367349359,-4.42038575566771,113.297843456184));
#50334=CARTESIAN_POINT('Ctrl Pts',(-5.18030469794229,-3.31954849808144,
113.219687368191));
#50335=CARTESIAN_POINT('Ctrl Pts',(-5.90675465652134,-1.65187112670505,
113.141531280198));
#50336=CARTESIAN_POINT('Ctrl Pts',(-5.92118311221449,0.004721389953629,
113.063375192205));
#50337=CARTESIAN_POINT('Ctrl Pts',(-5.91902054661466,0.00524085415724961,
112.811624807795));
#50338=CARTESIAN_POINT('Ctrl Pts',(-5.90438870483032,-1.57999266034137,
112.886343693202));
#50339=CARTESIAN_POINT('Ctrl Pts',(-5.2472450749989,-3.17592571538899,112.961062578609));
#50340=CARTESIAN_POINT('Ctrl Pts',(-4.10855477015215,-4.27124396878244,
113.035781464017));
#50341=CARTESIAN_POINT('Ctrl Pts',(-2.69419327792475,-5.63173325435863,
113.128589415232));
#50342=CARTESIAN_POINT('Ctrl Pts',(-0.536901624861667,-6.21987407527553,
113.221397366448));
#50343=CARTESIAN_POINT('Ctrl Pts',(1.37225226391009,-5.76547231928087,113.314205317664));
#50344=CARTESIAN_POINT('Ctrl Pts',(3.28140615268174,-5.31107056328625,113.40701326888));
#50345=CARTESIAN_POINT('Ctrl Pts',(4.94242227716222,-3.81412623038015,113.499821220095));
#50346=CARTESIAN_POINT('Ctrl Pts',(5.59222356256014,-1.96234119524295,113.592629171311));
#50347=CARTESIAN_POINT('Ctrl Pts',(6.2420248479581,-0.110556160105644,113.685437122527));
#50348=CARTESIAN_POINT('Ctrl Pts',(5.88061129427344,2.09606957726296,113.778245073742));
#50349=CARTESIAN_POINT('Ctrl Pts',(4.67401765172385,3.64380382726269,113.871053024958));
#50350=CARTESIAN_POINT('Ctrl Pts',(3.46742400917419,5.19153807726251,113.963860976174));
#50351=CARTESIAN_POINT('Ctrl Pts',(1.41565027775974,6.0803808398934,114.056668927389));
#50352=CARTESIAN_POINT('Ctrl Pts',(-0.538710948729533,5.90199439629684,
114.149476878605));
#50353=CARTESIAN_POINT('Ctrl Pts',(-2.49307217521848,5.72360795270031,114.242284829821));
#50354=CARTESIAN_POINT('Ctrl Pts',(-4.3500208967822,4.47799230287646,114.335092781037));
#50355=CARTESIAN_POINT('Ctrl Pts',(-5.25646786425308,2.73738797620561,114.427900732252));
#50356=CARTESIAN_POINT('Ctrl Pts',(-5.69182489694245,1.90139385637306,114.4724754241));
#50357=CARTESIAN_POINT('Ctrl Pts',(-5.90792200995091,0.951216698938335,
114.517050115948));
#50358=CARTESIAN_POINT('Ctrl Pts',(-5.90700152101349,0.000644589703395199,
114.561624807795));
#50359=CARTESIAN_POINT('Origin',(0.,0.,-10.));
#50360=CARTESIAN_POINT('',(-5.91459626807812,-0.00538349094479307,116.563375192205));
#50361=CARTESIAN_POINT('',(-5.91664694577537,-0.00546538710318724,116.311624807795));
#50362=CARTESIAN_POINT('',(-5.91675,-7.2459289488551E-16,-10.));
#50363=CARTESIAN_POINT('Ctrl Pts',(-5.91459626807812,-0.00538349094479307,
116.563375192205));
#50364=CARTESIAN_POINT('Ctrl Pts',(-5.9018638407151,1.4363059330357,116.495551957875));
#50365=CARTESIAN_POINT('Ctrl Pts',(-5.37115148883914,2.88638679209883,116.427728723546));
#50366=CARTESIAN_POINT('Ctrl Pts',(-4.41417274127812,3.95458278837131,116.359905489217));
#50367=CARTESIAN_POINT('Ctrl Pts',(-3.10491894606437,5.41599419977019,116.26711573064));
#50368=CARTESIAN_POINT('Ctrl Pts',(-0.997809742128125,6.16262042901297,
116.174325972063));
#50369=CARTESIAN_POINT('Ctrl Pts',(0.939488296168799,5.85158164612673,116.081536213487));
#50370=CARTESIAN_POINT('Ctrl Pts',(2.8767863344655,5.54054286324053,115.98874645491));
#50371=CARTESIAN_POINT('Ctrl Pts',(4.64427320712292,4.17183906822554,115.895956696333));
#50372=CARTESIAN_POINT('Ctrl Pts',(5.43025013550231,2.37403232619154,115.803166937756));
#50373=CARTESIAN_POINT('Ctrl Pts',(6.21622706388179,0.576225584157339,115.71037717918));
#50374=CARTESIAN_POINT('Ctrl Pts',(6.02069404798297,-1.650684104896,115.617587420603));
#50375=CARTESIAN_POINT('Ctrl Pts',(4.93344746063551,-3.28401312011301,115.524797662026));
#50376=CARTESIAN_POINT('Ctrl Pts',(3.84620087328818,-4.91734213532984,115.432007903449));
#50377=CARTESIAN_POINT('Ctrl Pts',(1.86724071449241,-5.95709047671048,115.339218144873));
#50378=CARTESIAN_POINT('Ctrl Pts',(-0.0946174716486306,-5.92576522940153,
115.246428386296));
#50379=CARTESIAN_POINT('Ctrl Pts',(-2.05647565779001,-5.89443998209257,
115.153638627719));
#50380=CARTESIAN_POINT('Ctrl Pts',(-4.00123187127666,-4.79204114609361,
115.060848869142));
#50381=CARTESIAN_POINT('Ctrl Pts',(-5.03577835122075,-3.12483318231579,
114.968059110565));
#50382=CARTESIAN_POINT('Ctrl Pts',(-5.61065394704331,-2.19840098219977,
114.916497804445));
#50383=CARTESIAN_POINT('Ctrl Pts',(-5.90447590817912,-1.0975675947347,114.864936498325));
#50384=CARTESIAN_POINT('Ctrl Pts',(-5.90744685829511,0.00179048289942529,
114.813375192205));
#50385=CARTESIAN_POINT('Ctrl Pts',(-5.90700152101349,0.000644589703395199,
114.561624807795));
#50386=CARTESIAN_POINT('Ctrl Pts',(-5.90600548088795,-1.02794785126051,
114.609858067163));
#50387=CARTESIAN_POINT('Ctrl Pts',(-5.65090545221675,-2.05700273779024,
114.658091326531));
#50388=CARTESIAN_POINT('Ctrl Pts',(-5.14454243958478,-2.94235117338353,
114.706324585899));
#50389=CARTESIAN_POINT('Ctrl Pts',(-4.17022483406764,-4.64589299278287,
114.799132537115));
#50390=CARTESIAN_POINT('Ctrl Pts',(-2.26564440965561,-5.81738362806337,
114.891940488331));
#50391=CARTESIAN_POINT('Ctrl Pts',(-0.305772599524579,-5.91863586120825,
114.984748439547));
#50392=CARTESIAN_POINT('Ctrl Pts',(1.65409921060645,-6.01988809435313,115.077556390762));
#50393=CARTESIAN_POINT('Ctrl Pts',(3.66926240645635,-5.05090192536239,115.170364341978));
#50394=CARTESIAN_POINT('Ctrl Pts',(4.8139434124092,-3.45683325636664,115.263172293194));
#50395=CARTESIAN_POINT('Ctrl Pts',(5.95862441836219,-1.86276458737071,115.355980244409));
#50396=CARTESIAN_POINT('Ctrl Pts',(6.23282323441778,0.356386581630305,115.448788195625));
#50397=CARTESIAN_POINT('Ctrl Pts',(5.5105718898964,2.1811338304845,115.541596146841));
#50398=CARTESIAN_POINT('Ctrl Pts',(4.78832054537515,4.00588107933838,115.634404098056));
#50399=CARTESIAN_POINT('Ctrl Pts',(3.06961904027696,5.43622440804573,115.727212049272));
#50400=CARTESIAN_POINT('Ctrl Pts',(1.14404533090283,5.81505869454813,115.820020000488));
#50401=CARTESIAN_POINT('Ctrl Pts',(-0.781528378471534,6.19389298105057,
115.912827951704));
#50402=CARTESIAN_POINT('Ctrl Pts',(-2.91397429212202,5.52121822534809,116.005635902919));
#50403=CARTESIAN_POINT('Ctrl Pts',(-4.27363871135382,4.10606374828964,116.098443854135));
#50404=CARTESIAN_POINT('Ctrl Pts',(-5.31469375657614,3.02252159827662,116.169504172022));
#50405=CARTESIAN_POINT('Ctrl Pts',(-5.90270453950121,1.50369964399586,116.240564489909));
#50406=CARTESIAN_POINT('Ctrl Pts',(-5.91664694577537,-0.00546538710318724,
116.311624807795));
#50407=CARTESIAN_POINT('Origin',(0.,0.,-10.));
#50408=CARTESIAN_POINT('',(-5.92643375485155,0.000646757142401377,118.313375192205));
#50409=CARTESIAN_POINT('',(-5.92583646225612,0.00184477398095578,118.061624807795));
#50410=CARTESIAN_POINT('',(-5.91675,-7.2459289488551E-16,-10.));
#50411=CARTESIAN_POINT('Ctrl Pts',(-5.92643375485155,0.000646757142401377,
118.313375192205));
#50412=CARTESIAN_POINT('Ctrl Pts',(-5.92648696415084,0.0350788317316276,
118.311746934579));
#50413=CARTESIAN_POINT('Ctrl Pts',(-5.92621294326389,0.0695100363376435,
118.310118676954));
#50414=CARTESIAN_POINT('Ctrl Pts',(-5.9256091198181,0.103935456191626,118.308490419329));
#50415=CARTESIAN_POINT('Ctrl Pts',(-5.89119894363559,2.06574195873543,118.215700660752));
#50416=CARTESIAN_POINT('Ctrl Pts',(-4.78574339534727,4.00876227624729,118.122910902175));
#50417=CARTESIAN_POINT('Ctrl Pts',(-3.11691069714255,5.04068583884809,118.030121143598));
#50418=CARTESIAN_POINT('Ctrl Pts',(-1.44807799893782,6.07260940144889,117.937331385022));
#50419=CARTESIAN_POINT('Ctrl Pts',(0.784131849183317,6.19343620913865,117.844541626445));
#50420=CARTESIAN_POINT('Ctrl Pts',(2.554601186991,5.3476778881445,117.751751867868));
#50421=CARTESIAN_POINT('Ctrl Pts',(4.32507052479859,4.50191956715039,117.658962109291));
#50422=CARTESIAN_POINT('Ctrl Pts',(5.63379935229277,2.68957611747247,117.566172350715));
#50423=CARTESIAN_POINT('Ctrl Pts',(5.87976844422231,0.742946204144582,117.473382592138));
#50424=CARTESIAN_POINT('Ctrl Pts',(6.12573753615187,-1.20368370918353,117.380592833561));
#50425=CARTESIAN_POINT('Ctrl Pts',(5.30894689251649,-3.28460008616166,117.287803074984));
#50426=CARTESIAN_POINT('Ctrl Pts',(3.80449857381735,-4.54416511823098,117.195013316408));
#50427=CARTESIAN_POINT('Ctrl Pts',(2.3000502551182,-5.80373015030029,117.102223557831));
#50428=CARTESIAN_POINT('Ctrl Pts',(0.107944261355265,-6.24194383746075,
117.009433799254));
#50429=CARTESIAN_POINT('Ctrl Pts',(-1.76511899837069,-5.65756139529358,
116.916644040677));
#50430=CARTESIAN_POINT('Ctrl Pts',(-3.63818225809653,-5.07317895312644,
116.823854282101));
#50431=CARTESIAN_POINT('Ctrl Pts',(-5.19220278378542,-3.46620038163178,
116.731064523524));
#50432=CARTESIAN_POINT('Ctrl Pts',(-5.71351385338424,-1.57461279910704,
116.638274764947));
#50433=CARTESIAN_POINT('Ctrl Pts',(-5.85378068519037,-1.06565181063473,
116.6133082407));
#50434=CARTESIAN_POINT('Ctrl Pts',(-5.91928322321424,-0.536086196545553,
116.588341716452));
#50435=CARTESIAN_POINT('Ctrl Pts',(-5.91459626807812,-0.00538349094479307,
116.563375192205));
#50436=CARTESIAN_POINT('Ctrl Pts',(-5.91664694577537,-0.00546538710318724,
116.311624807795));
#50437=CARTESIAN_POINT('Ctrl Pts',(-5.920913945254,-0.467337339063882,116.333372441124));
#50438=CARTESIAN_POINT('Ctrl Pts',(-5.87141177430932,-0.92830479119591,
116.355120074453));
#50439=CARTESIAN_POINT('Ctrl Pts',(-5.7646712557571,-1.37561355519936,116.376867707782));
#50440=CARTESIAN_POINT('Ctrl Pts',(-5.30915645611559,-3.28450218321582,
116.469675658998));
#50441=CARTESIAN_POINT('Ctrl Pts',(-3.8112439320195,-4.94464524083455,116.562483610214));
#50442=CARTESIAN_POINT('Ctrl Pts',(-1.9590803488349,-5.59336674347474,116.655291561429));
#50443=CARTESIAN_POINT('Ctrl Pts',(-0.106916765650188,-6.24208824611498,
116.748099512645));
#50444=CARTESIAN_POINT('Ctrl Pts',(2.09949787662346,-5.87938819377639,116.840907463861));
#50445=CARTESIAN_POINT('Ctrl Pts',(3.64652836626847,-4.67189235901254,116.933715415076));
#50446=CARTESIAN_POINT('Ctrl Pts',(5.19355885591348,-3.46439652424869,117.026523366292));
#50447=CARTESIAN_POINT('Ctrl Pts',(6.08120519293021,-1.41210490705985,117.119331317508));
#50448=CARTESIAN_POINT('Ctrl Pts',(5.90167930090155,0.542151980085433,117.212139268724));
#50449=CARTESIAN_POINT('Ctrl Pts',(5.72215340887289,2.49640886723071,117.304947219939));
#50450=CARTESIAN_POINT('Ctrl Pts',(4.47545528779867,4.35263102433215,117.397755171155));
#50451=CARTESIAN_POINT('Ctrl Pts',(2.7343227584359,5.25806298867747,117.490563122371));
#50452=CARTESIAN_POINT('Ctrl Pts',(0.993190229073134,6.16349495302279,117.583371073586));
#50453=CARTESIAN_POINT('Ctrl Pts',(-1.24237670857819,6.11813672461201,117.676179024802));
#50454=CARTESIAN_POINT('Ctrl Pts',(-2.94535016830966,5.14282604471886,117.768986976018));
#50455=CARTESIAN_POINT('Ctrl Pts',(-4.64832362804114,4.1675153648257,117.861794927234));
#50456=CARTESIAN_POINT('Ctrl Pts',(-5.81870360985277,2.26225223345017,117.954602878449));
#50457=CARTESIAN_POINT('Ctrl Pts',(-5.91881313412188,0.302321721923281,
118.047410829665));
#50458=CARTESIAN_POINT('Ctrl Pts',(-5.92392388368571,0.202264169157404,
118.052148822375));
#50459=CARTESIAN_POINT('Ctrl Pts',(-5.92624522588486,0.102064138766616,
118.056886815085));
#50460=CARTESIAN_POINT('Ctrl Pts',(-5.92583646225612,0.00184477398095578,
118.061624807795));
#50461=CARTESIAN_POINT('Origin',(0.,0.,-10.));
#50462=CARTESIAN_POINT('',(-5.91264952969134,0.00505721487104038,120.063375192205));
#50463=CARTESIAN_POINT('',(-5.91102966775968,0.00455868499465235,119.811624807795));
#50464=CARTESIAN_POINT('',(-5.91675,-7.2459289488551E-16,-10.));
#50465=CARTESIAN_POINT('Ctrl Pts',(-5.91264952969134,0.00505721487104038,
120.063375192205));
#50466=CARTESIAN_POINT('Ctrl Pts',(-5.91750501305584,0.605482795756369,
120.035152152707));
#50467=CARTESIAN_POINT('Ctrl Pts',(-5.83342087274394,1.20458030872588,120.006929113208));
#50468=CARTESIAN_POINT('Ctrl Pts',(-5.65477879996619,1.77401317452086,119.97870607371));
#50469=CARTESIAN_POINT('Ctrl Pts',(-5.06745174024911,3.6461551933258,119.885916315134));
#50470=CARTESIAN_POINT('Ctrl Pts',(-3.458031501331,5.19764686847578,119.793126556557));
#50471=CARTESIAN_POINT('Ctrl Pts',(-1.56562651024018,5.71598282453298,119.70033679798));
#50472=CARTESIAN_POINT('Ctrl Pts',(0.326778480850637,6.23431878059017,119.607547039403));
#50473=CARTESIAN_POINT('Ctrl Pts',(2.50216822411417,5.71949901755457,119.514757280827));
#50474=CARTESIAN_POINT('Ctrl Pts',(3.96151906342687,4.40794881209317,119.42196752225));
#50475=CARTESIAN_POINT('Ctrl Pts',(5.42086990273941,3.09639860663192,119.329177763673));
#50476=CARTESIAN_POINT('Ctrl Pts',(6.16418183810132,0.988117958745099,119.236388005096));
#50477=CARTESIAN_POINT('Ctrl Pts',(5.85009709231295,-0.948688584539746,
119.143598246519));
#50478=CARTESIAN_POINT('Ctrl Pts',(5.53601234652456,-2.8854951278247,119.050808487943));
#50479=CARTESIAN_POINT('Ctrl Pts',(4.16453091958576,-4.65082756650766,118.958018729366));
#50480=CARTESIAN_POINT('Ctrl Pts',(2.36549047331626,-5.43397652190135,118.865228970789));
#50481=CARTESIAN_POINT('Ctrl Pts',(0.566450027046652,-6.21712547729509,
118.772439212213));
#50482=CARTESIAN_POINT('Ctrl Pts',(-1.66014943855372,-6.01809094939945,
118.679649453636));
#50483=CARTESIAN_POINT('Ctrl Pts',(-3.29176676931556,-4.92827734166367,
118.586859695059));
#50484=CARTESIAN_POINT('Ctrl Pts',(-4.89475277910877,-3.85758758276841,
118.495698194108));
#50485=CARTESIAN_POINT('Ctrl Pts',(-5.92345471792749,-1.92710690519565,
118.404536693156));
#50486=CARTESIAN_POINT('Ctrl Pts',(-5.92643375485155,0.000646757142401377,
118.313375192205));
#50487=CARTESIAN_POINT('Ctrl Pts',(-5.92583646225612,0.00184477398095578,
118.061624807795));
#50488=CARTESIAN_POINT('Ctrl Pts',(-5.91823835098307,-1.86103595172694,
118.149694766301));
#50489=CARTESIAN_POINT('Ctrl Pts',(-4.96734794015348,-3.7305969993527,118.237764724806));
#50490=CARTESIAN_POINT('Ctrl Pts',(-3.45402592757642,-4.81595808036472,
118.325834683312));
#50491=CARTESIAN_POINT('Ctrl Pts',(-1.85929013003522,-5.95970947944757,
118.418642634528));
#50492=CARTESIAN_POINT('Ctrl Pts',(0.360020531773886,-6.23261438593508,
118.511450585744));
#50493=CARTESIAN_POINT('Ctrl Pts',(2.18434636610108,-5.50929925608524,118.604258536959));
#50494=CARTESIAN_POINT('Ctrl Pts',(4.00867220042817,-4.78598412623543,118.697066488175));
#50495=CARTESIAN_POINT('Ctrl Pts',(5.43801320727335,-3.06644896004871,118.789874439391));
#50496=CARTESIAN_POINT('Ctrl Pts',(5.81572473502421,-1.14065470087481,118.882682390606));
#50497=CARTESIAN_POINT('Ctrl Pts',(6.19343626277509,0.7851395582992,118.975490341822));
#50498=CARTESIAN_POINT('Ctrl Pts',(5.51951831143128,2.91719291046021,119.068298293038));
#50499=CARTESIAN_POINT('Ctrl Pts',(4.10357133061007,4.27603200114264,119.161106244254));
#50500=CARTESIAN_POINT('Ctrl Pts',(2.68762434978902,5.63487109182491,119.253914195469));
#50501=CARTESIAN_POINT('Ctrl Pts',(0.529648339490302,6.2204959210289,119.346722146685));
#50502=CARTESIAN_POINT('Ctrl Pts',(-1.37897437886234,5.76386823258837,119.439530097901));
#50503=CARTESIAN_POINT('Ctrl Pts',(-3.2875970972153,5.30724054414775,119.532338049116));
#50504=CARTESIAN_POINT('Ctrl Pts',(-4.94686652362224,3.80836033806268,119.625146000332));
#50505=CARTESIAN_POINT('Ctrl Pts',(-5.59450802297796,1.95581883645566,119.717953951548));
#50506=CARTESIAN_POINT('Ctrl Pts',(-5.81239572545508,1.33256351398138,119.749177570297));
#50507=CARTESIAN_POINT('Ctrl Pts',(-5.91578041622014,0.669278371866502,
119.780401189046));
#50508=CARTESIAN_POINT('Ctrl Pts',(-5.91102966775968,0.00455868499465235,
119.811624807795));
#50509=CARTESIAN_POINT('Origin',(0.,0.,-10.));
#50510=CARTESIAN_POINT('',(-5.90826032391765,-0.00283186500595667,121.813375192205));
#50511=CARTESIAN_POINT('',(-5.90927045785071,-0.00365599742955411,121.561624807795));
#50512=CARTESIAN_POINT('',(-5.91675,-7.2459289488551E-16,-10.));
#50513=CARTESIAN_POINT('Ctrl Pts',(-5.90826032391765,-0.00283186500595667,
121.813375192205));
#50514=CARTESIAN_POINT('Ctrl Pts',(-5.90322516476143,1.16555772389332,121.758557370834));
#50515=CARTESIAN_POINT('Ctrl Pts',(-5.56844404220564,2.3366080019099,121.703739549463));
#50516=CARTESIAN_POINT('Ctrl Pts',(-4.9230950366585,3.29951227908924,121.648921728092));
#50517=CARTESIAN_POINT('Ctrl Pts',(-3.83071710326124,4.92941389096632,121.556131969515));
#50518=CARTESIAN_POINT('Ctrl Pts',(-1.84849678431158,5.9629333781242,121.463342210938));
#50519=CARTESIAN_POINT('Ctrl Pts',(0.113253183721438,5.92543835814145,121.370552452362));
#50520=CARTESIAN_POINT('Ctrl Pts',(2.07500315175423,5.88794333815871,121.277762693785));
#50521=CARTESIAN_POINT('Ctrl Pts',(4.01628276887011,4.7794338110354,121.184972935208));
#50522=CARTESIAN_POINT('Ctrl Pts',(5.04558086252729,3.10898050488358,121.092183176631));
#50523=CARTESIAN_POINT('Ctrl Pts',(6.07487895618459,1.43852719873157,120.999393418055));
#50524=CARTESIAN_POINT('Ctrl Pts',(6.19219552638293,-0.793869886449118,
120.906603659478));
#50525=CARTESIAN_POINT('Ctrl Pts',(5.34365423708173,-2.56300710385687,120.813813900901));
#50526=CARTESIAN_POINT('Ctrl Pts',(4.49511294778054,-4.33214432126463,120.721024142324));
#50527=CARTESIAN_POINT('Ctrl Pts',(2.68071379897976,-5.63802167089943,120.628234383748));
#50528=CARTESIAN_POINT('Ctrl Pts',(0.733699512763562,-5.88092943716167,
120.535444625171));
#50529=CARTESIAN_POINT('Ctrl Pts',(-1.21331477345253,-6.12383720342389,
120.442654866594));
#50530=CARTESIAN_POINT('Ctrl Pts',(-3.29294419708403,-5.30377538631367,
120.349865108017));
#50531=CARTESIAN_POINT('Ctrl Pts',(-4.5501419686417,-3.79734829652869,120.257075349441));
#50532=CARTESIAN_POINT('Ctrl Pts',(-5.42494902264784,-2.74911779986066,
120.192508630362));
#50533=CARTESIAN_POINT('Ctrl Pts',(-5.90154149044533,-1.36855492960636,
120.127941911283));
#50534=CARTESIAN_POINT('Ctrl Pts',(-5.91264952969134,0.00505721487104038,
120.063375192205));
#50535=CARTESIAN_POINT('Ctrl Pts',(-5.91102966775968,0.00455868499465235,
119.811624807795));
#50536=CARTESIAN_POINT('Ctrl Pts',(-5.9016594639084,-1.30651030166878,119.873209140262));
#50537=CARTESIAN_POINT('Ctrl Pts',(-5.47161876324425,-2.62315998102597,
119.934793472728));
#50538=CARTESIAN_POINT('Ctrl Pts',(-4.66976547813631,-3.64925166567194,
119.996377805195));
#50539=CARTESIAN_POINT('Ctrl Pts',(-3.46136786163473,-5.19557786906385,
120.089185756411));
#50540=CARTESIAN_POINT('Ctrl Pts',(-1.40855905632735,-6.08202747871909,
120.181993707626));
#50541=CARTESIAN_POINT('Ctrl Pts',(0.545592827142654,-5.90136219928656,
120.274801658842));
#50542=CARTESIAN_POINT('Ctrl Pts',(2.49974471061277,-5.72069691985401,120.367609610058));
#50543=CARTESIAN_POINT('Ctrl Pts',(4.35523967224537,-4.4729167513336,120.460417561273));
#50544=CARTESIAN_POINT('Ctrl Pts',(5.25965632567281,-2.7312566111601,120.553225512489));
#50545=CARTESIAN_POINT('Ctrl Pts',(6.16407297910019,-0.989596470986702,
120.646033463705));
#50546=CARTESIAN_POINT('Ctrl Pts',(6.11741132432244,1.2459436408396,120.738841414921));
#50547=CARTESIAN_POINT('Ctrl Pts',(5.14110790159988,2.94834816199279,120.831649366136));
#50548=CARTESIAN_POINT('Ctrl Pts',(4.16480447887727,4.65075268314607,120.924457317352));
#50549=CARTESIAN_POINT('Ctrl Pts',(2.25885928820944,5.82002161362627,121.017265268568));
#50550=CARTESIAN_POINT('Ctrl Pts',(0.298870741548488,5.91898839498991,121.110073219783));
#50551=CARTESIAN_POINT('Ctrl Pts',(-1.66111780511235,6.01795517635354,121.202881170999));
#50552=CARTESIAN_POINT('Ctrl Pts',(-3.67514970776645,5.04661980860101,121.295689122215));
#50553=CARTESIAN_POINT('Ctrl Pts',(-4.81797111117614,3.45121742462712,121.388497073431));
#50554=CARTESIAN_POINT('Ctrl Pts',(-5.5285929841372,2.45917454999816,121.446206318219));
#50555=CARTESIAN_POINT('Ctrl Pts',(-5.9023594588355,1.22583483209864,121.503915563007));
#50556=CARTESIAN_POINT('Ctrl Pts',(-5.90927045785071,-0.00365599742955411,
121.561624807795));
#50557=CARTESIAN_POINT('Origin',(0.,0.,-10.));
#50558=CARTESIAN_POINT('',(-5.92304633245574,-0.00398199821673939,123.563375192205));
#50559=CARTESIAN_POINT('',(-5.92441432658438,-0.0031840572747424,123.311624807795));
#50560=CARTESIAN_POINT('',(-5.91675,-7.2459289488551E-16,-10.));
#50561=CARTESIAN_POINT('Ctrl Pts',(-5.92304633245574,-0.00398199821673939,
123.563375192205));
#50562=CARTESIAN_POINT('Ctrl Pts',(-5.90972172210851,1.72022136801727,123.481962588961));
#50563=CARTESIAN_POINT('Ctrl Pts',(-5.11364227888086,3.45513729943991,123.400549985717));
#50564=CARTESIAN_POINT('Ctrl Pts',(-3.79018862841945,4.55610756923942,123.319137382473));
#50565=CARTESIAN_POINT('Ctrl Pts',(-2.28178649139079,5.81093497267106,123.226347623897));
#50566=CARTESIAN_POINT('Ctrl Pts',(-0.0883131846642343,6.24225244714527,
123.13355786532));
#50567=CARTESIAN_POINT('Ctrl Pts',(1.78290296347007,5.65198222160363,123.040768106743));
#50568=CARTESIAN_POINT('Ctrl Pts',(3.65411911160426,5.06171199606203,122.947978348167));
#50569=CARTESIAN_POINT('Ctrl Pts',(5.20307810114624,3.4498540705047,122.85518858959));
#50570=CARTESIAN_POINT('Ctrl Pts',(5.71843766228389,1.55663635042864,122.762398831013));
#50571=CARTESIAN_POINT('Ctrl Pts',(6.23379722342157,-0.336581369647533,
122.669609072436));
#50572=CARTESIAN_POINT('Ctrl Pts',(5.71555735615491,-2.51115888424216,122.576819313859));
#50573=CARTESIAN_POINT('Ctrl Pts',(4.40171398332094,-3.96844554312672,122.484029555283));
#50574=CARTESIAN_POINT('Ctrl Pts',(3.08787061048711,-5.42573220201112,122.391239796706));
#50575=CARTESIAN_POINT('Ctrl Pts',(0.978423732085748,-6.16572800518541,
122.298450038129));
#50576=CARTESIAN_POINT('Ctrl Pts',(-0.957886527019627,-5.84859807304264,
122.205660279552));
#50577=CARTESIAN_POINT('Ctrl Pts',(-2.89419678612522,-5.53146814089984,
122.112870520976));
#50578=CARTESIAN_POINT('Ctrl Pts',(-4.65737042593512,-4.15721247343991,
122.020080762399));
#50579=CARTESIAN_POINT('Ctrl Pts',(-5.43768947191774,-2.35694277141183,
121.927291003822));
#50580=CARTESIAN_POINT('Ctrl Pts',(-5.75701593928944,-1.62022646642786,
121.889319066616));
#50581=CARTESIAN_POINT('Ctrl Pts',(-5.91174814489485,-0.812167496962084,
121.851347129411));
#50582=CARTESIAN_POINT('Ctrl Pts',(-5.90826032391765,-0.00283186500595667,
121.813375192205));
#50583=CARTESIAN_POINT('Ctrl Pts',(-5.90927045785071,-0.00365599742955411,
121.561624807795));
#50584=CARTESIAN_POINT('Ctrl Pts',(-5.91347372071519,-0.751431121489131,
121.596723514223));
#50585=CARTESIAN_POINT('Ctrl Pts',(-5.78197492207068,-1.49778251843781,
121.63182222065));
#50586=CARTESIAN_POINT('Ctrl Pts',(-5.50802474944973,-2.18755815917475,
121.666920927078));
#50587=CARTESIAN_POINT('Ctrl Pts',(-4.78364608014831,-4.01146195880812,
121.759728878293));
#50588=CARTESIAN_POINT('Ctrl Pts',(-3.06327783737993,-5.43980015787935,
121.852536829509));
#50589=CARTESIAN_POINT('Ctrl Pts',(-1.13726368307564,-5.81638879848899,
121.945344780725));
#50590=CARTESIAN_POINT('Ctrl Pts',(0.788750471228538,-6.19297743909861,
122.038152731941));
#50591=CARTESIAN_POINT('Ctrl Pts',(2.9204105370686,-5.51781652124677,122.130960683156));
#50592=CARTESIAN_POINT('Ctrl Pts',(4.27842383730411,-4.10107751798203,122.223768634372));
#50593=CARTESIAN_POINT('Ctrl Pts',(5.63643713753963,-2.68433851471728,122.316576585588));
#50594=CARTESIAN_POINT('Ctrl Pts',(6.22080367217059,-0.526021426039627,
122.409384536803));
#50595=CARTESIAN_POINT('Ctrl Pts',(5.76306325010652,1.38233473379682,122.502192488019));
#50596=CARTESIAN_POINT('Ctrl Pts',(5.30532282804248,3.29069089363317,122.595000439235));
#50597=CARTESIAN_POINT('Ctrl Pts',(3.80547544928359,4.94908612462835,122.68780839045));
#50598=CARTESIAN_POINT('Ctrl Pts',(1.95255665910373,5.59564740060542,122.780616341666));
#50599=CARTESIAN_POINT('Ctrl Pts',(0.0996378689237742,6.24220867658253,
122.873424292882));
#50600=CARTESIAN_POINT('Ctrl Pts',(-2.10635233267718,5.87693599754143,122.966232244098));
#50601=CARTESIAN_POINT('Ctrl Pts',(-3.65197372433744,4.66763700996177,123.059040195313));
#50602=CARTESIAN_POINT('Ctrl Pts',(-5.05415308196879,3.57056751626948,123.143235066141));
#50603=CARTESIAN_POINT('Ctrl Pts',(-5.91284757783128,1.77886266924099,123.227429936968));
#50604=CARTESIAN_POINT('Ctrl Pts',(-5.92441432658438,-0.0031840572747424,
123.311624807795));
#50605=CARTESIAN_POINT('Origin',(0.,0.,-10.));
#50606=CARTESIAN_POINT('',(-5.92082732894822,0.0048284439233276,125.313375192205));
#50607=CARTESIAN_POINT('',(-5.91915982610221,0.00521712502770736,125.061624807795));
#50608=CARTESIAN_POINT('',(-5.91675,-7.2459289488551E-16,-10.));
#50609=CARTESIAN_POINT('Ctrl Pts',(-5.92082732894822,0.0048284439233276,
125.313375192205));
#50610=CARTESIAN_POINT('Ctrl Pts',(-5.9236770812749,0.327430742195007,125.298157565665));
#50611=CARTESIAN_POINT('Ctrl Pts',(-5.8995936395555,0.64960709265275,125.282939939125));
#50612=CARTESIAN_POINT('Ctrl Pts',(-5.84708469732352,0.9670819991819,125.267722312585));
#50613=CARTESIAN_POINT('Ctrl Pts',(-5.52691045332391,2.90289109885381,125.174932554009));
#50614=CARTESIAN_POINT('Ctrl Pts',(-4.1498837400031,4.66390177683713,125.082142795432));
#50615=CARTESIAN_POINT('Ctrl Pts',(-2.34838918584629,5.44138903022236,124.989353036855));
#50616=CARTESIAN_POINT('Ctrl Pts',(-0.546894631689373,6.21887628360764,
124.896563278278));
#50617=CARTESIAN_POINT('Ctrl Pts',(1.67906776330359,6.01284011239471,124.803773519702));
#50618=CARTESIAN_POINT('Ctrl Pts',(3.30724960074758,4.91790052991357,124.710983761125));
#50619=CARTESIAN_POINT('Ctrl Pts',(4.93543143819138,3.82296094743256,124.618194002548));
#50620=CARTESIAN_POINT('Ctrl Pts',(5.96583271808636,1.83911795368359,124.525404243971));
#50621=CARTESIAN_POINT('Ctrl Pts',(5.92525296043562,-0.122570616094663,
124.432614485395));
#50622=CARTESIAN_POINT('Ctrl Pts',(5.88467320278487,-2.08425918587314,124.339824726818));
#50623=CARTESIAN_POINT('Ctrl Pts',(4.77311240758814,-4.02379333168089,124.247034968241));
#50624=CARTESIAN_POINT('Ctrl Pts',(3.10104261686253,-5.05046341815464,124.154245209664));
#50625=CARTESIAN_POINT('Ctrl Pts',(1.42897282613711,-6.07713350462827,124.061455451088));
#50626=CARTESIAN_POINT('Ctrl Pts',(-0.803605960117068,-6.19093953176812,
123.968665692511));
#50627=CARTESIAN_POINT('Ctrl Pts',(-2.57140667886717,-5.33961736868184,
123.875875933934));
#50628=CARTESIAN_POINT('Ctrl Pts',(-4.33920739761747,-4.48829520559547,
123.783086175357));
#50629=CARTESIAN_POINT('Ctrl Pts',(-5.64223004886356,-2.6718448522827,123.690296416781));
#50630=CARTESIAN_POINT('Ctrl Pts',(-5.88207589082117,-0.724451009431805,
123.597506658204));
#50631=CARTESIAN_POINT('Ctrl Pts',(-5.91148391431208,-0.485676789252728,
123.586129502871));
#50632=CARTESIAN_POINT('Ctrl Pts',(-5.92490840485771,-0.244933997561633,
123.574752347538));
#50633=CARTESIAN_POINT('Ctrl Pts',(-5.92304633245574,-0.00398199821673939,
123.563375192205));
#50634=CARTESIAN_POINT('Ctrl Pts',(-5.92441432658438,-0.0031840572747424,
123.311624807795));
#50635=CARTESIAN_POINT('Ctrl Pts',(-5.92559759744001,-0.185486275457294,
123.320237888184));
#50636=CARTESIAN_POINT('Ctrl Pts',(-5.91791554376533,-0.367687419896257,
123.328850968572));
#50637=CARTESIAN_POINT('Ctrl Pts',(-5.90104309195602,-0.54903348900264,
123.337464048961));
#50638=CARTESIAN_POINT('Ctrl Pts',(-5.71923848619479,-2.50307970426905,
123.430272000176));
#50639=CARTESIAN_POINT('Ctrl Pts',(-4.47037669295292,-4.35784683868379,
123.523079951392));
#50640=CARTESIAN_POINT('Ctrl Pts',(-2.7281895346718,-5.26124787418566,123.615887902608));
#50641=CARTESIAN_POINT('Ctrl Pts',(-0.986002376390676,-6.16464890968752,
123.708695853823));
#50642=CARTESIAN_POINT('Ctrl Pts',(1.24951014692971,-6.11668384627651,123.801503805039));
#50643=CARTESIAN_POINT('Ctrl Pts',(2.95134515200119,-5.13938801177825,123.894311756255));
#50644=CARTESIAN_POINT('Ctrl Pts',(4.65318015707267,-4.16209217727999,123.98711970747));
#50645=CARTESIAN_POINT('Ctrl Pts',(5.82133764389525,-2.25546557169447,124.079927658686));
#50646=CARTESIAN_POINT('Ctrl Pts',(5.91916164642105,-0.29541965774841,124.172735609902));
#50647=CARTESIAN_POINT('Ctrl Pts',(6.01698564894686,1.66462625619787,124.265543561117));
#50648=CARTESIAN_POINT('Ctrl Pts',(5.04447616717559,3.67809147850472,124.358351512333));
#50649=CARTESIAN_POINT('Ctrl Pts',(3.44840774343408,4.81998250071349,124.451159463549));
#50650=CARTESIAN_POINT('Ctrl Pts',(1.85233931969265,5.96187352292221,124.543967414765));
#50651=CARTESIAN_POINT('Ctrl Pts',(-0.367288046018615,6.23219034503295,
124.63677536598));
#50652=CARTESIAN_POINT('Ctrl Pts',(-2.19076919910286,5.50674837692975,124.729583317196));
#50653=CARTESIAN_POINT('Ctrl Pts',(-4.014250352187,4.78130640882659,124.822391268412));
#50654=CARTESIAN_POINT('Ctrl Pts',(-5.44158529264409,3.06010565050916,124.915199219628));
#50655=CARTESIAN_POINT('Ctrl Pts',(-5.81705090267984,1.13387226637038,125.008007170843));
#50656=CARTESIAN_POINT('Ctrl Pts',(-5.88935641279735,0.762926742405473,
125.025879716494));
#50657=CARTESIAN_POINT('Ctrl Pts',(-5.92265297372955,0.384377510403178,
125.043752262145));
#50658=CARTESIAN_POINT('Ctrl Pts',(-5.91915982610221,0.00521712502770735,
125.061624807795));
#50659=CARTESIAN_POINT('Origin',(0.,0.,-10.));
#50660=CARTESIAN_POINT('',(-5.90733548964813,0.0015994485885984,127.063375192205));
#50661=CARTESIAN_POINT('',(-5.90701629014678,0.000721185244744792,126.811624807795));
#50662=CARTESIAN_POINT('',(-5.91675,-7.2459289488551E-16,-10.));
#50663=CARTESIAN_POINT('Ctrl Pts',(-5.90733548964813,0.0015994485885984,
127.063375192205));
#50664=CARTESIAN_POINT('Ctrl Pts',(-5.90948223967714,0.893133898673095,
127.021562783792));
#50665=CARTESIAN_POINT('Ctrl Pts',(-5.72044046389006,1.78380468906801,126.97975037538));
#50666=CARTESIAN_POINT('Ctrl Pts',(-5.33557206520579,2.57979528293403,126.937937966967));
#50667=CARTESIAN_POINT('Ctrl Pts',(-4.4814752276016,4.346251170993,126.84514820839));
#50668=CARTESIAN_POINT('Ctrl Pts',(-2.66296894213967,5.64642482067912,126.752358449814));
#50669=CARTESIAN_POINT('Ctrl Pts',(-0.715198189598532,5.88321024295047,
126.659568691237));
#50670=CARTESIAN_POINT('Ctrl Pts',(1.23257256294227,6.11999566522179,126.56677893266));
#50671=CARTESIAN_POINT('Ctrl Pts',(3.30960778256256,5.29339286007849,126.473989174083));
#50672=CARTESIAN_POINT('Ctrl Pts',(4.56206056674281,3.78301829464937,126.381199415506));
#50673=CARTESIAN_POINT('Ctrl Pts',(5.81451335092313,2.27264372922017,126.28840965693));
#50674=CARTESIAN_POINT('Ctrl Pts',(6.24238369966374,0.0784974035052743,
126.195619898353));
#50675=CARTESIAN_POINT('Ctrl Pts',(5.64917237601244,-1.79178765869978,126.102830139776));
#50676=CARTESIAN_POINT('Ctrl Pts',(5.05596105236112,-3.66207272090495,126.0100403812));
#50677=CARTESIAN_POINT('Ctrl Pts',(3.44166805631763,-5.2084965195999,125.917250622623));
#50678=CARTESIAN_POINT('Ctrl Pts',(1.54764196647018,-5.72087872310008,125.824460864046));
#50679=CARTESIAN_POINT('Ctrl Pts',(-0.346384123377259,-6.23326092660026,
125.731671105469));
#50680=CARTESIAN_POINT('Ctrl Pts',(-2.52014330702865,-5.71160153490567,
125.638881346893));
#50681=CARTESIAN_POINT('Ctrl Pts',(-3.97536201151514,-4.39546807837805,
125.546091588316));
#50682=CARTESIAN_POINT('Ctrl Pts',(-5.19192318398324,-3.29518201411753,
125.468519456279));
#50683=CARTESIAN_POINT('Ctrl Pts',(-5.90630066388776,-1.63964272322248,
125.390947324242));
#50684=CARTESIAN_POINT('Ctrl Pts',(-5.92082732894822,0.0048284439233276,
125.313375192205));
#50685=CARTESIAN_POINT('Ctrl Pts',(-5.91915982610221,0.00521712502770735,
125.061624807795));
#50686=CARTESIAN_POINT('Ctrl Pts',(-5.90451387474925,-1.58451372852251,
125.13656021336));
#50687=CARTESIAN_POINT('Ctrl Pts',(-5.24313102181849,-3.18498822355375,
125.211495618925));
#50688=CARTESIAN_POINT('Ctrl Pts',(-4.09858227733526,-4.28081419582354,
125.28643102449));
#50689=CARTESIAN_POINT('Ctrl Pts',(-2.68105176234036,-5.63800126391799,
125.379238975706));
#50690=CARTESIAN_POINT('Ctrl Pts',(-0.522394452736071,-6.22110939014652,
125.472046926922));
#50691=CARTESIAN_POINT('Ctrl Pts',(1.38569455481539,-5.76225635239487,125.564854878137));
#50692=CARTESIAN_POINT('Ctrl Pts',(3.29378356236686,-5.30340331464321,125.657662829353));
#50693=CARTESIAN_POINT('Ctrl Pts',(4.95130426786537,-3.8025891129114,125.750470780569));
#50694=CARTESIAN_POINT('Ctrl Pts',(5.59678499689816,-1.94929373516699,125.843278731785));
#50695=CARTESIAN_POINT('Ctrl Pts',(6.24226572593094,-0.0959983574225864,
125.936086683));
#50696=CARTESIAN_POINT('Ctrl Pts',(5.87570647849779,2.10977819633463,126.028894634216));
#50697=CARTESIAN_POINT('Ctrl Pts',(4.66550672687537,3.65469438514516,126.121702585432));
#50698=CARTESIAN_POINT('Ctrl Pts',(3.45530697525289,5.19961057395578,126.214510536647));
#50699=CARTESIAN_POINT('Ctrl Pts',(1.40146671944114,6.08366639781989,126.307318487863));
#50700=CARTESIAN_POINT('Ctrl Pts',(-0.552473533347532,5.90072227394494,
126.400126439079));
#50701=CARTESIAN_POINT('Ctrl Pts',(-2.5064137861362,5.71777815007,126.492934390295));
#50702=CARTESIAN_POINT('Ctrl Pts',(-4.36045403590167,4.46783407845601,126.58574234151));
#50703=CARTESIAN_POINT('Ctrl Pts',(-5.26283844776865,2.72512097313255,126.678550292726));
#50704=CARTESIAN_POINT('Ctrl Pts',(-5.69413902220643,1.89217976368593,126.722908464416));
#50705=CARTESIAN_POINT('Ctrl Pts',(-5.90804095800662,0.946669164313941,
126.767266636106));
#50706=CARTESIAN_POINT('Ctrl Pts',(-5.90701629014678,0.000721185244744792,
126.811624807795));
#50707=CARTESIAN_POINT('Origin',(0.,0.,-10.));
#50708=CARTESIAN_POINT('',(-5.91675,7.2459289488551E-16,147.));
#50709=CARTESIAN_POINT('Origin',(0.,0.,147.));
#50710=CARTESIAN_POINT('',(-5.91675,-7.2459289488551E-16,130.));
#50711=CARTESIAN_POINT('',(-5.91675,-7.2459289488551E-16,-10.));
#50712=CARTESIAN_POINT('',(2.58391981634458,5.32271443393329,130.));
#50713=CARTESIAN_POINT('Origin',(0.,0.,130.));
#50714=CARTESIAN_POINT('',(-5.91448192755925,-0.0049507822674949,128.813375192205));
#50715=CARTESIAN_POINT('Ctrl Pts',(2.58391981634458,5.32271443393329,130.));
#50716=CARTESIAN_POINT('Ctrl Pts',(3.47055515188225,4.89229596196688,129.953605120712));
#50717=CARTESIAN_POINT('Ctrl Pts',(4.24029712840795,4.23605651223856,129.907210241423));
#50718=CARTESIAN_POINT('Ctrl Pts',(4.81442615980519,3.43370417302639,129.860815362135));
#50719=CARTESIAN_POINT('Ctrl Pts',(5.38855519120244,2.63135183381422,129.814420482847));
#50720=CARTESIAN_POINT('Ctrl Pts',(5.76707127747114,1.68288660511834,129.768025603558));
#50721=CARTESIAN_POINT('Ctrl Pts',(5.88207504663892,0.705646679344999,129.72163072427));
#50722=CARTESIAN_POINT('Ctrl Pts',(6.11208258497448,-1.2488331722018,129.628840965693));
#50723=CARTESIAN_POINT('Ctrl Pts',(5.28804085490593,-3.31841181205823,129.536051207116));
#50724=CARTESIAN_POINT('Ctrl Pts',(3.7771742476755,-4.56683408622936,129.443261448539));
#50725=CARTESIAN_POINT('Ctrl Pts',(2.26630764044515,-5.81525636040042,129.350471689963));
#50726=CARTESIAN_POINT('Ctrl Pts',(0.0686161560530948,-6.24252226888644,
129.257681931386));
#50727=CARTESIAN_POINT('Ctrl Pts',(-1.80142318997057,-5.64706513861724,
129.164892172809));
#50728=CARTESIAN_POINT('Ctrl Pts',(-3.67146253599433,-5.05160800834801,
129.072102414232));
#50729=CARTESIAN_POINT('Ctrl Pts',(-5.21384974364968,-3.43342783932321,
128.979312655656));
#50730=CARTESIAN_POINT('Ctrl Pts',(-5.72289947820789,-1.53825253979548,
128.886522897079));
#50731=CARTESIAN_POINT('Ctrl Pts',(-5.85666359298725,-1.04025317139774,
128.862140328787));
#50732=CARTESIAN_POINT('Ctrl Pts',(-5.91907655599569,-0.523127503885872,
128.837757760496));
#50733=CARTESIAN_POINT('Ctrl Pts',(-5.91448192755925,-0.0049507822674949,
128.813375192205));
#50734=CARTESIAN_POINT('',(-5.91642361182645,-0.00541095714722729,128.561624807795));
#50735=CARTESIAN_POINT('',(-5.91675,-7.2459289488551E-16,-10.));
#50736=CARTESIAN_POINT('',(-2.59168464642692,5.32810255942641,130.));
#50737=CARTESIAN_POINT('Ctrl Pts',(-5.91642361182645,-0.00541095714722729,
128.561624807795));
#50738=CARTESIAN_POINT('Ctrl Pts',(-5.92072243615008,-0.47190700523705,
128.583588961282));
#50739=CARTESIAN_POINT('Ctrl Pts',(-5.87022027230614,-0.937486925898181,
128.605553114769));
#50740=CARTESIAN_POINT('Ctrl Pts',(-5.76137787898222,-1.38900619205342,
128.627517268256));
#50741=CARTESIAN_POINT('Ctrl Pts',(-5.30147217235758,-3.29686838447854,
128.720325219472));
#50742=CARTESIAN_POINT('Ctrl Pts',(-3.79994585631488,-4.95368824049658,
128.813133170687));
#50743=CARTESIAN_POINT('Ctrl Pts',(-1.94616157152931,-5.5980107456732,128.905941121903));
#50744=CARTESIAN_POINT('Ctrl Pts',(-0.092377286743959,-6.24233325084974,
128.998749073119));
#50745=CARTESIAN_POINT('Ctrl Pts',(2.11366496678405,-5.87415840518507,129.091557024334));
#50746=CARTESIAN_POINT('Ctrl Pts',(3.65766172888916,-4.66320511213384,129.18436497555));
#50747=CARTESIAN_POINT('Ctrl Pts',(5.20165849099436,-3.45225181908255,129.277172926766));
#50748=CARTESIAN_POINT('Ctrl Pts',(6.08360976167645,-1.3985200786447,129.369980877982));
#50749=CARTESIAN_POINT('Ctrl Pts',(5.89993317977312,0.555595301027637,129.462788829197));
#50750=CARTESIAN_POINT('Ctrl Pts',(5.7162565978698,2.50971068069987,129.555596780413));
#50751=CARTESIAN_POINT('Ctrl Pts',(4.46695216338095,4.36420969960679,129.648404731629));
#50752=CARTESIAN_POINT('Ctrl Pts',(2.7229167058007,5.26500797028939,129.741212682844));
#50753=CARTESIAN_POINT('Ctrl Pts',(1.10188369738893,6.10227519691029,129.827475121896));
#50754=CARTESIAN_POINT('Ctrl Pts',(-0.946556911312304,6.11562209275089,
129.913737560948));
#50755=CARTESIAN_POINT('Ctrl Pts',(-2.59168464642692,5.32810255942641,130.));
#50756=CARTESIAN_POINT('Origin',(0.,0.,130.));
#50757=CARTESIAN_POINT('Origin',(0.,0.,-13.2351405640096));
#50758=CARTESIAN_POINT('',(-4.9163646833512,-0.00411529722797478,129.38985943599));
#50759=CARTESIAN_POINT('',(-4.92459990823896,0.000661498711628031,129.735140564009));
#50760=CARTESIAN_POINT('',(-4.91825,6.88216836313478E-12,-13.2351405640096));
#50761=CARTESIAN_POINT('',(2.86417334265864,-4.00661193697147,130.));
#50762=CARTESIAN_POINT('Ctrl Pts',(-4.9163646833512,-0.00411529722797478,
129.38985943599));
#50763=CARTESIAN_POINT('Ctrl Pts',(-4.92018393062525,-0.43484545501757,
129.414242004282));
#50764=CARTESIAN_POINT('Ctrl Pts',(-4.86830366606858,-0.864701932685717,
129.438624572573));
#50765=CARTESIAN_POINT('Ctrl Pts',(-4.75711334071876,-1.27865983079266,
129.463007140865));
#50766=CARTESIAN_POINT('Ctrl Pts',(-4.33396991620548,-2.85400878366436,
129.555796899442));
#50767=CARTESIAN_POINT('Ctrl Pts',(-3.05187317660211,-4.19910780192726,
129.648586658018));
#50768=CARTESIAN_POINT('Ctrl Pts',(-1.49741827930524,-4.69407666675153,
129.741376416595));
#50769=CARTESIAN_POINT('Ctrl Pts',(-0.0532262264089908,-5.15393568373128,
129.82758427773));
#50770=CARTESIAN_POINT('Ctrl Pts',(1.62605576293774,-4.87999239627907,129.913792138865));
#50771=CARTESIAN_POINT('Ctrl Pts',(2.86417334265864,-4.00661193697147,130.));
#50772=CARTESIAN_POINT('',(-2.85706463458608,-4.00329423553871,130.));
#50773=CARTESIAN_POINT('Origin',(0.,0.,130.));
#50774=CARTESIAN_POINT('Ctrl Pts',(-4.92459990823896,0.000661498711628031,
129.735140564009));
#50775=CARTESIAN_POINT('Ctrl Pts',(-4.92384457190956,-0.738149461065841,
129.777023067065));
#50776=CARTESIAN_POINT('Ctrl Pts',(-4.74695671268496,-1.47922316861453,
129.818905570121));
#50777=CARTESIAN_POINT('Ctrl Pts',(-4.42287481469073,-2.14486768324074,
129.860788073176));
#50778=CARTESIAN_POINT('Ctrl Pts',(-4.06380629222381,-2.88237259738225,
129.907192048784));
#50779=CARTESIAN_POINT('Ctrl Pts',(-3.52404725972277,-3.52728314116421,
129.953596024392));
#50780=CARTESIAN_POINT('Ctrl Pts',(-2.85706463458654,-4.00329423553838,
130.));
#50781=CARTESIAN_POINT('Origin',(0.,0.,-13.2351405640096));
#50782=CARTESIAN_POINT('',(-4.91042426534194,0.00132952854738158,127.63985943599));
#50783=CARTESIAN_POINT('',(-4.91797869250264,-0.00449781382338033,127.985140564009));
#50784=CARTESIAN_POINT('',(-4.91825,6.88216836313478E-12,-13.2351405640096));
#50785=CARTESIAN_POINT('Ctrl Pts',(-4.91042426534194,0.00132952854738161,
127.63985943599));
#50786=CARTESIAN_POINT('Ctrl Pts',(-4.90824865591709,-0.902190083096324,
127.690836786155));
#50787=CARTESIAN_POINT('Ctrl Pts',(-4.23589608641458,-3.4533195340969,127.834603894896));
#50788=CARTESIAN_POINT('Ctrl Pts',(-0.129499705332998,-5.81541776548578,
128.071160762213));
#50789=CARTESIAN_POINT('Ctrl Pts',(4.82184908053961,-3.25351245829232,128.349530037944));
#50790=CARTESIAN_POINT('Ctrl Pts',(5.34408280538262,2.29632880892462,128.627899313674));
#50791=CARTESIAN_POINT('Ctrl Pts',(0.958562204898396,5.73769098457033,128.906268589404));
#50792=CARTESIAN_POINT('Ctrl Pts',(-3.84727915788463,4.06816077427375,129.160255296843));
#50793=CARTESIAN_POINT('Ctrl Pts',(-4.90564948830288,1.20433163556846,129.321452245705));
#50794=CARTESIAN_POINT('Ctrl Pts',(-4.9163646833512,-0.00411529722797593,
129.38985943599));
#50795=CARTESIAN_POINT('Ctrl Pts',(-4.91797869250264,-0.00449781382338123,
127.985140564009));
#50796=CARTESIAN_POINT('Ctrl Pts',(-4.92155205503,-0.39226883482863,128.007104717496));
#50797=CARTESIAN_POINT('Ctrl Pts',(-4.70219114273014,-2.41455913631502,
128.121876822199));
#50798=CARTESIAN_POINT('Ctrl Pts',(-1.91054242683083,-5.49493073827346,
128.329456878117));
#50799=CARTESIAN_POINT('Ctrl Pts',(3.59072126358126,-4.5768037590934,128.607880731764));
#50800=CARTESIAN_POINT('Ctrl Pts',(5.79006558455199,0.54463932997096,128.886304585412));
#50801=CARTESIAN_POINT('Ctrl Pts',(2.67464333335573,5.16925071277719,129.164728439058));
#50802=CARTESIAN_POINT('Ctrl Pts',(-2.90822559480448,5.03732645866885,129.443152292706));
#50803=CARTESIAN_POINT('Ctrl Pts',(-4.88224936370592,1.79675240995502,129.633289667689));
#50804=CARTESIAN_POINT('Ctrl Pts',(-4.92468145141885,0.0804206638054886,
129.730619091457));
#50805=CARTESIAN_POINT('Ctrl Pts',(-4.92459990823896,0.000661498711627927,
129.735140564009));
#50806=CARTESIAN_POINT('Origin',(0.,0.,-13.2351405640096));
#50807=CARTESIAN_POINT('',(-4.92163924630915,0.0040136044860252,125.88985943599));
#50808=CARTESIAN_POINT('',(-4.91015893336957,0.000599479339165321,126.235140564009));
#50809=CARTESIAN_POINT('',(-4.91825,6.88216836313478E-12,-13.2351405640096));
#50810=CARTESIAN_POINT('Ctrl Pts',(-4.92163924630915,0.00401360448602523,
125.88985943599));
#50811=CARTESIAN_POINT('Ctrl Pts',(-4.90956407490104,-1.36293959073401,
125.967431568027));
#50812=CARTESIAN_POINT('Ctrl Pts',(-3.60543114971607,-4.38521193124015,
126.137793458641));
#50813=CARTESIAN_POINT('Ctrl Pts',(1.51899055903744,-5.61497221539792,126.400945107832));
#50814=CARTESIAN_POINT('Ctrl Pts',(5.54459407167148,-1.75861584681939,126.679314383562));
#50815=CARTESIAN_POINT('Ctrl Pts',(4.4776028977884,3.71298266576747,126.957683659292));
#50816=CARTESIAN_POINT('Ctrl Pts',(-0.701952670164813,5.77430311013206,
127.236052935023));
#50817=CARTESIAN_POINT('Ctrl Pts',(-4.40634675631825,3.12578018922078,127.463444860589));
#50818=CARTESIAN_POINT('Ctrl Pts',(-4.91220873372888,0.742410241629219,
127.598047027578));
#50819=CARTESIAN_POINT('Ctrl Pts',(-4.91042426534194,0.00132952854738161,
127.63985943599));
#50820=CARTESIAN_POINT('Ctrl Pts',(-4.91015893336957,0.000599479339165182,
126.235140564009));
#50821=CARTESIAN_POINT('Ctrl Pts',(-4.90922862128532,-0.858241586946162,
126.283590343535));
#50822=CARTESIAN_POINT('Ctrl Pts',(-4.28511186721648,-3.36349980276401,
126.424848074277));
#50823=CARTESIAN_POINT('Ctrl Pts',(-0.286591160200441,-5.81013496081811,
126.658913756234));
#50824=CARTESIAN_POINT('Ctrl Pts',(4.73304984475302,-3.38201813095182,126.937337609882));
#50825=CARTESIAN_POINT('Ctrl Pts',(5.40386860173048,2.15348096294236,127.215761463529));
#50826=CARTESIAN_POINT('Ctrl Pts',(1.10968603140598,5.71042388849744,127.494185317176));
#50827=CARTESIAN_POINT('Ctrl Pts',(-3.78509266885793,4.15375692724055,127.750645017336));
#50828=CARTESIAN_POINT('Ctrl Pts',(-4.90645306861513,1.24622973155316,127.91429676628));
#50829=CARTESIAN_POINT('Ctrl Pts',(-4.91797869250264,-0.00449781382338123,
127.985140564009));
#50830=CARTESIAN_POINT('Origin',(0.,0.,-13.2351405640096));
#50831=CARTESIAN_POINT('',(-4.92348377480886,-0.0033100034161842,124.13985943599));
#50832=CARTESIAN_POINT('',(-4.92025314821947,0.00433669247712778,124.485140564009));
#50833=CARTESIAN_POINT('',(-4.91825,6.88216836313478E-12,-13.2351405640096));
#50834=CARTESIAN_POINT('Ctrl Pts',(-4.92348377480886,-0.00331000341618409,
124.13985943599));
#50835=CARTESIAN_POINT('Ctrl Pts',(-4.92503160724926,-0.203599380317578,
124.151236591323));
#50836=CARTESIAN_POINT('Ctrl Pts',(-4.82286209861274,-2.03581585448879,
124.255403505233));
#50837=CARTESIAN_POINT('Ctrl Pts',(-2.52380371468285,-5.24076813201426,
124.45236017772));
#50838=CARTESIAN_POINT('Ctrl Pts',(3.04363480249081,-4.95696714685634,124.73072945345));
#50839=CARTESIAN_POINT('Ctrl Pts',(5.8155622361216,-0.120301504763635,125.00909872918));
#50840=CARTESIAN_POINT('Ctrl Pts',(3.24602435053818,4.82685823868056,125.287468004911));
#50841=CARTESIAN_POINT('Ctrl Pts',(-2.30491470342209,5.34065588049586,125.565837280641));
#50842=CARTESIAN_POINT('Ctrl Pts',(-4.78192169540783,2.17293537069928,125.766634424334));
#50843=CARTESIAN_POINT('Ctrl Pts',(-4.92400807960103,0.27217412393866,125.874641809451));
#50844=CARTESIAN_POINT('Ctrl Pts',(-4.92163924630915,0.00401360448602523,
125.88985943599));
#50845=CARTESIAN_POINT('Ctrl Pts',(-4.92025314821947,0.00433669247712733,
124.485140564009));
#50846=CARTESIAN_POINT('Ctrl Pts',(-4.90807882105857,-1.31711406519994,
124.560075969574));
#50847=CARTESIAN_POINT('Ctrl Pts',(-3.67741741891198,-4.29518066827556,
124.727819326355));
#50848=CARTESIAN_POINT('Ctrl Pts',(1.36013010449734,-5.65595010773044,124.988370634352));
#50849=CARTESIAN_POINT('Ctrl Pts',(5.49353165593364,-1.91333155142861,125.266794487999));
#50850=CARTESIAN_POINT('Ctrl Pts',(4.57943353516515,3.58726955670461,125.545218341646));
#50851=CARTESIAN_POINT('Ctrl Pts',(-0.542280161447921,5.79186205548623,
125.823642195293));
#50852=CARTESIAN_POINT('Ctrl Pts',(-4.36119727820526,3.21725084589819,126.053616269414));
#50853=CARTESIAN_POINT('Ctrl Pts',(-4.91101068013832,0.786910992930685,
126.190782392319));
#50854=CARTESIAN_POINT('Ctrl Pts',(-4.91015893336957,0.000599479339165182,
126.235140564009));
#50855=CARTESIAN_POINT('Origin',(0.,0.,-13.2351405640096));
#50856=CARTESIAN_POINT('',(-4.91119302625731,-0.00235396460084376,122.38985943599));
#50857=CARTESIAN_POINT('',(-4.92462090872917,-0.00264672153492462,122.735140564009));
#50858=CARTESIAN_POINT('',(-4.91825,6.88216836313478E-12,-13.2351405640096));
#50859=CARTESIAN_POINT('Ctrl Pts',(-4.91119302625731,-0.00235396460084351,
122.38985943599));
#50860=CARTESIAN_POINT('Ctrl Pts',(-4.91409224889185,-0.675107583035024,
122.427831373196));
#50861=CARTESIAN_POINT('Ctrl Pts',(-4.47117164087798,-2.98817465699793,
122.558593068979));
#50862=CARTESIAN_POINT('Ctrl Pts',(-0.940153731250069,-5.74032638196031,
122.782144523338));
#50863=CARTESIAN_POINT('Ctrl Pts',(4.3202276147748,-3.89498002173257,123.060513799069));
#50864=CARTESIAN_POINT('Ctrl Pts',(5.61257555605349,1.52781924872262,123.338883074799));
#50865=CARTESIAN_POINT('Ctrl Pts',(1.74989711756287,5.54735036413612,123.617252350529));
#50866=CARTESIAN_POINT('Ctrl Pts',(-3.49646344277389,4.51572304497822,123.884244470926));
#50867=CARTESIAN_POINT('Ctrl Pts',(-4.91240780153887,1.42991992956681,124.058446832747));
#50868=CARTESIAN_POINT('Ctrl Pts',(-4.92348377480886,-0.00331000341618409,
124.13985943599));
#50869=CARTESIAN_POINT('Ctrl Pts',(-4.92462090872918,-0.00264672153492481,
122.735140564009));
#50870=CARTESIAN_POINT('Ctrl Pts',(-4.92560449294135,-0.15418394798358,
122.743753644397));
#50871=CARTESIAN_POINT('Ctrl Pts',(-4.85041204194471,-1.937580837054,122.845174676002));
#50872=CARTESIAN_POINT('Ctrl Pts',(-2.67785788744019,-5.1641845055458,123.039403658822));
#50873=CARTESIAN_POINT('Ctrl Pts',(2.89689656449083,-5.04457280666451,123.317827512469));
#50874=CARTESIAN_POINT('Ctrl Pts',(5.80996060787651,-0.289969534807391,
123.596251366116));
#50875=CARTESIAN_POINT('Ctrl Pts',(3.3847889720702,4.73105991359457,123.874675219763));
#50876=CARTESIAN_POINT('Ctrl Pts',(-2.15035225820507,5.40515584988507,124.15309907341));
#50877=CARTESIAN_POINT('Ctrl Pts',(-4.75175655075456,2.26816332338643,124.356587521492));
#50878=CARTESIAN_POINT('Ctrl Pts',(-4.9231567985875,0.319510658820078,124.467268018358));
#50879=CARTESIAN_POINT('Ctrl Pts',(-4.92025314821947,0.00433669247712733,
124.485140564009));
#50880=CARTESIAN_POINT('Origin',(0.,0.,-13.2351405640096));
#50881=CARTESIAN_POINT('',(-4.91484151762446,0.00420376846348179,120.63985943599));
#50882=CARTESIAN_POINT('',(-4.91203269181966,-0.00303901792530925,120.985140564009));
#50883=CARTESIAN_POINT('',(-4.91825,6.88216836313478E-12,-13.2351405640096));
#50884=CARTESIAN_POINT('Ctrl Pts',(-4.91484151762446,0.00420376846348151,
120.63985943599));
#50885=CARTESIAN_POINT('Ctrl Pts',(-4.90560805093787,-1.13760008155203,
120.704426155069));
#50886=CARTESIAN_POINT('Ctrl Pts',(-3.94011208720615,-3.93438762851029,
120.861782632725));
#50887=CARTESIAN_POINT('Ctrl Pts',(0.720116960871199,-5.77205921455916,
121.111928868956));
#50888=CARTESIAN_POINT('Ctrl Pts',(5.24473027743382,-2.51555964562078,121.390298144687));
#50889=CARTESIAN_POINT('Ctrl Pts',(4.95217496174117,3.05142575896264,121.668667420417));
#50890=CARTESIAN_POINT('Ctrl Pts',(0.111156593441196,5.81574416777347,121.947036696148));
#50891=CARTESIAN_POINT('Ctrl Pts',(-4.15767394946337,3.58999786132769,122.187434034672));
#50892=CARTESIAN_POINT('Ctrl Pts',(-4.90700759142861,0.968860316144871,
122.335041614619));
#50893=CARTESIAN_POINT('Ctrl Pts',(-4.91119302625731,-0.00235396460084351,
122.38985943599));
#50894=CARTESIAN_POINT('Ctrl Pts',(-4.91203269181966,-0.00303901792530974,
120.985140564009));
#50895=CARTESIAN_POINT('Ctrl Pts',(-4.91552661966674,-0.624620968137917,
121.020239270437));
#50896=CARTESIAN_POINT('Ctrl Pts',(-4.51718910800845,-2.88547628658539,
121.14814592808));
#50897=CARTESIAN_POINT('Ctrl Pts',(-1.11628260678685,-5.7090837831698,121.368860536939));
#50898=CARTESIAN_POINT('Ctrl Pts',(4.19949232986848,-4.02541782590159,121.647284390586));
#50899=CARTESIAN_POINT('Ctrl Pts',(5.65674202384814,1.35683240677064,121.925708244233));
#50900=CARTESIAN_POINT('Ctrl Pts',(1.9165344585906,5.49241478468641,122.20413209788));
#50901=CARTESIAN_POINT('Ctrl Pts',(-3.41442109159254,4.60970351323632,122.473942871139));
#50902=CARTESIAN_POINT('Ctrl Pts',(-4.91500614351677,1.47866503114549,122.650945693182));
#50903=CARTESIAN_POINT('Ctrl Pts',(-4.92462090872918,-0.00264672153492481,
122.735140564009));
#50904=CARTESIAN_POINT('Origin',(0.,0.,-13.2351405640096));
#50905=CARTESIAN_POINT('',(-4.92629954194425,0.000537611582497406,118.88985943599));
#50906=CARTESIAN_POINT('',(-4.91349502065481,0.00378936958999432,119.235140564009));
#50907=CARTESIAN_POINT('',(-4.91825,6.88216836313478E-12,-13.2351405640096));
#50908=CARTESIAN_POINT('Ctrl Pts',(-4.92629954194425,0.000537611582497478,
118.88985943599));
#50909=CARTESIAN_POINT('Ctrl Pts',(-4.92382324188989,-1.6018918386726,118.981020936942));
#50910=CARTESIAN_POINT('Ctrl Pts',(-3.19834996239224,-4.83994622551109,
119.16497219647));
#50911=CARTESIAN_POINT('Ctrl Pts',(2.32169952544947,-5.33338047839311,119.441713214575));
#50912=CARTESIAN_POINT('Ctrl Pts',(5.74179765096292,-0.931126065133631,
119.720082490305));
#50913=CARTESIAN_POINT('Ctrl Pts',(3.88818176753445,4.3263470221884,119.998451766036));
#50914=CARTESIAN_POINT('Ctrl Pts',(-1.53664297821521,5.61016616253672,120.276821041766));
#50915=CARTESIAN_POINT('Ctrl Pts',(-4.6191898500751,2.63857074308124,120.490623598417));
#50916=CARTESIAN_POINT('Ctrl Pts',(-4.91887759842147,0.503302617187181,
120.611636396492));
#50917=CARTESIAN_POINT('Ctrl Pts',(-4.91484151762446,0.00420376846348151,
120.63985943599));
#50918=CARTESIAN_POINT('Ctrl Pts',(-4.91349502065481,0.00378936958999446,
119.235140564009));
#50919=CARTESIAN_POINT('Ctrl Pts',(-4.90570611541432,-1.08602599250415,
119.296724896476));
#50920=CARTESIAN_POINT('Ctrl Pts',(-4.00953220865736,-3.8298292770796,119.451117180158));
#50921=CARTESIAN_POINT('Ctrl Pts',(0.535527329685027,-5.79248953224288,
119.698317415056));
#50922=CARTESIAN_POINT('Ctrl Pts',(5.16262232020387,-2.68086838186981,119.976741268703));
#50923=CARTESIAN_POINT('Ctrl Pts',(5.04626096459074,2.89395486822036,120.25516512235));
#50924=CARTESIAN_POINT('Ctrl Pts',(0.29335695445051,5.80979054693031,120.533588975998));
#50925=CARTESIAN_POINT('Ctrl Pts',(-4.09594578481282,3.69290005239632,120.776914123217));
#50926=CARTESIAN_POINT('Ctrl Pts',(-4.90628798046357,1.01896516888556,120.927431319221));
#50927=CARTESIAN_POINT('Ctrl Pts',(-4.91203269181966,-0.00303901792530974,
120.985140564009));
#50928=CARTESIAN_POINT('Origin',(0.,0.,-13.2351405640096));
#50929=CARTESIAN_POINT('',(-4.91645972797145,-0.00447498277304698,117.13985943599));
#50930=CARTESIAN_POINT('',(-4.92580304736406,0.00153345327726321,117.485140564009));
#50931=CARTESIAN_POINT('',(-4.91825,6.88216836313478E-12,-13.2351405640096));
#50932=CARTESIAN_POINT('Ctrl Pts',(-4.91645972797146,-0.00447498277304677,
117.13985943599));
#50933=CARTESIAN_POINT('Ctrl Pts',(-4.92035572105884,-0.445617262204197,
117.164825960238));
#50934=CARTESIAN_POINT('Ctrl Pts',(-4.66354596905633,-2.52183626266821,
117.282582243062));
#50935=CARTESIAN_POINT('Ctrl Pts',(-1.73244237806593,-5.5528262552018,117.493128284463));
#50936=CARTESIAN_POINT('Ctrl Pts',(3.7340681068242,-4.46004163516174,117.771497560194));
#50937=CARTESIAN_POINT('Ctrl Pts',(5.77091971441071,0.72919247363337,118.049866835924));
#50938=CARTESIAN_POINT('Ctrl Pts',(2.50730934259094,5.24867944099596,118.328236111654));
#50939=CARTESIAN_POINT('Ctrl Pts',(-3.05920914417388,4.94737055676852,118.606605387384));
#50940=CARTESIAN_POINT('Ctrl Pts',(-4.91313559719146,1.68878926784965,118.793813162163));
#50941=CARTESIAN_POINT('Ctrl Pts',(-4.92634377173867,0.0291589917059973,
118.888231178365));
#50942=CARTESIAN_POINT('Ctrl Pts',(-4.92629954194425,0.000537611582497478,
118.88985943599));
#50943=CARTESIAN_POINT('Ctrl Pts',(-4.92580304736406,0.00153345327726352,
117.485140564009));
#50944=CARTESIAN_POINT('Ctrl Pts',(-4.91948717957292,-1.54697089948827,
117.573210522515));
#50945=CARTESIAN_POINT('Ctrl Pts',(-3.2961243867519,-4.73869079598163,117.754088432236));
#50946=CARTESIAN_POINT('Ctrl Pts',(2.14404793895791,-5.40765965436446,118.027774293173));
#50947=CARTESIAN_POINT('Ctrl Pts',(5.70843197086043,-1.11961106463314,118.306198146821));
#50948=CARTESIAN_POINT('Ctrl Pts',(4.02786563079502,4.19714462012598,118.584622000468));
#50949=CARTESIAN_POINT('Ctrl Pts',(-1.35353404604633,5.65753215529382,118.863045854115));
#50950=CARTESIAN_POINT('Ctrl Pts',(-4.57606832878287,2.74649626627515,119.079885375295));
#50951=CARTESIAN_POINT('Ctrl Pts',(-4.91744404141966,0.556332167569323,
119.20391694526));
#50952=CARTESIAN_POINT('Ctrl Pts',(-4.91349502065481,0.00378936958999446,
119.235140564009));
#50953=CARTESIAN_POINT('Origin',(0.,0.,-13.2351405640096));
#50954=CARTESIAN_POINT('',(-4.91051683961802,0.0014883242551948,115.38985943599));
#50955=CARTESIAN_POINT('',(-4.91816433701936,-0.0045430582786804,115.735140564009));
#50956=CARTESIAN_POINT('',(-4.91825,6.88216836313478E-12,-13.2351405640096));
#50957=CARTESIAN_POINT('Ctrl Pts',(-4.91051683961802,0.00148832425519413,
115.38985943599));
#50958=CARTESIAN_POINT('Ctrl Pts',(-4.90804726165632,-0.912344077878977,
115.441420742111));
#50959=CARTESIAN_POINT('Ctrl Pts',(-4.22428092503253,-3.47414309954378,
115.585771806808));
#50960=CARTESIAN_POINT('Ctrl Pts',(-0.0928658734872262,-5.81606498788651,
115.822912630082));
#50961=CARTESIAN_POINT('Ctrl Pts',(4.84211742021259,-3.22321809728275,116.101281905812));
#50962=CARTESIAN_POINT('Ctrl Pts',(5.329723076416,2.33008324797548,116.379651181542));
#50963=CARTESIAN_POINT('Ctrl Pts',(0.922096096344309,5.74325472209657,116.658020457272));
#50964=CARTESIAN_POINT('Ctrl Pts',(-3.86118283221186,4.04836320761304,116.911423208755));
#50965=CARTESIAN_POINT('Ctrl Pts',(-4.90587600195934,1.19391754851335,117.072036201661));
#50966=CARTESIAN_POINT('Ctrl Pts',(-4.91645972797146,-0.00447498277304677,
117.13985943599));
#50967=CARTESIAN_POINT('Ctrl Pts',(-4.91816433701936,-0.00454305827868106,
115.735140564009));
#50968=CARTESIAN_POINT('Ctrl Pts',(-4.92171124540485,-0.388470337231666,
115.756888197338));
#50969=CARTESIAN_POINT('Ctrl Pts',(-4.70496285032225,-2.40684556258418,
115.871443781883));
#50970=CARTESIAN_POINT('Ctrl Pts',(-1.92293779473958,-5.49017620296048,
116.078807317644));
#50971=CARTESIAN_POINT('Ctrl Pts',(3.57925453095985,-4.58570185517924,116.35723117129));
#50972=CARTESIAN_POINT('Ctrl Pts',(5.79280078373477,0.532149961902354,116.635655024938));
#50973=CARTESIAN_POINT('Ctrl Pts',(2.68387796260612,5.16105837826204,116.914078878585));
#50974=CARTESIAN_POINT('Ctrl Pts',(-2.89101218372597,5.04794741013998,117.192502732232));
#50975=CARTESIAN_POINT('Ctrl Pts',(-4.88641623084225,1.79962650389789,117.382856627373));
#50976=CARTESIAN_POINT('Ctrl Pts',(-4.92614282878396,0.0848399798069363,
117.480402571299));
#50977=CARTESIAN_POINT('Ctrl Pts',(-4.92580304736406,0.00153345327726352,
117.485140564009));
#50978=CARTESIAN_POINT('Origin',(0.,0.,-13.2351405640096));
#50979=CARTESIAN_POINT('',(-4.92193498823661,0.0039246167501111,113.63985943599));
#50980=CARTESIAN_POINT('',(-4.91014665664844,0.000535809922468655,113.985140564009));
#50981=CARTESIAN_POINT('',(-4.91825,6.88216836313478E-12,-13.2351405640096));
#50982=CARTESIAN_POINT('Ctrl Pts',(-4.92193498823661,0.00392461675011099,
113.63985943599));
#50983=CARTESIAN_POINT('Ctrl Pts',(-4.9099414525611,-1.37310435102102,113.718015523984));
#50984=CARTESIAN_POINT('Ctrl Pts',(-3.58916649890494,-4.40514596226126,
113.888961370553));
#50985=CARTESIAN_POINT('Ctrl Pts',(1.55427901866009,-5.60530576738952,114.1526969757));
#50986=CARTESIAN_POINT('Ctrl Pts',(5.55554360765141,-1.72370857086153,114.43106625143));
#50987=CARTESIAN_POINT('Ctrl Pts',(4.45416440249025,3.74107678207312,114.70943552716));
#50988=CARTESIAN_POINT('Ctrl Pts',(-0.738266183349346,5.76976594467228,
114.987804802891));
#50989=CARTESIAN_POINT('Ctrl Pts',(-4.41643946083194,3.10487486952994,115.214612772501));
#50990=CARTESIAN_POINT('Ctrl Pts',(-4.91249151569284,0.73218928160962,115.348630983534));
#50991=CARTESIAN_POINT('Ctrl Pts',(-4.91051683961802,0.00148832425519413,
115.38985943599));
#50992=CARTESIAN_POINT('Ctrl Pts',(-4.91014665664844,0.0005358099224681,
113.985140564009));
#50993=CARTESIAN_POINT('Ctrl Pts',(-4.90931870644957,-0.854473236054642,
114.033373823377));
#50994=CARTESIAN_POINT('Ctrl Pts',(-4.28925358204272,-3.35577066657218,
114.174415033961));
#50995=CARTESIAN_POINT('Ctrl Pts',(-0.300131481883046,-5.80944451695458,
114.408264195761));
#50996=CARTESIAN_POINT('Ctrl Pts',(4.72513224634132,-3.39305905586345,114.686688049408));
#50997=CARTESIAN_POINT('Ctrl Pts',(5.40890880969165,2.14089467055971,114.965111903055));
#50998=CARTESIAN_POINT('Ctrl Pts',(1.12293914182643,5.70777821798859,115.243535756702));
#50999=CARTESIAN_POINT('Ctrl Pts',(-3.77942826098378,4.1613386229973,115.50021197702));
#51000=CARTESIAN_POINT('Ctrl Pts',(-4.90657482594142,1.2499380190338,115.664080246122));
#51001=CARTESIAN_POINT('Ctrl Pts',(-4.91816433701936,-0.00454305827868106,
115.735140564009));
#51002=CARTESIAN_POINT('Origin',(0.,0.,-13.2351405640096));
#51003=CARTESIAN_POINT('',(-4.92322087232039,-0.0034344185441411,111.88985943599));
#51004=CARTESIAN_POINT('',(-4.92013737328565,0.00435641712180093,112.235140564009));
#51005=CARTESIAN_POINT('',(-4.91825,6.88216836313478E-12,-13.2351405640096));
#51006=CARTESIAN_POINT('Ctrl Pts',(-4.92322087232039,-0.0034344185441413,
111.88985943599));
#51007=CARTESIAN_POINT('Ctrl Pts',(-4.92489330250895,-0.214033463505952,
111.90182054728));
#51008=CARTESIAN_POINT('Ctrl Pts',(-4.81683781957552,-2.05665137631426,
112.006571417145));
#51009=CARTESIAN_POINT('Ctrl Pts',(-2.49079015772174,-5.25653882359623,
112.204112045588));
#51010=CARTESIAN_POINT('Ctrl Pts',(3.07475320216653,-4.9377250591284,112.482481321318));
#51011=CARTESIAN_POINT('Ctrl Pts',(5.81620382629126,-0.0837201577406925,
112.760850597049));
#51012=CARTESIAN_POINT('Ctrl Pts',(3.21560001691721,4.84717985482067,113.039219872779));
#51013=CARTESIAN_POINT('Ctrl Pts',(-2.3384612089734,5.3260524957894,113.317589148509));
#51014=CARTESIAN_POINT('Ctrl Pts',(-4.78834883631155,2.15207245650155,113.517802336246));
#51015=CARTESIAN_POINT('Ctrl Pts',(-4.92418061560507,0.261754669609081,
113.625225765407));
#51016=CARTESIAN_POINT('Ctrl Pts',(-4.92193498823661,0.00392461675011099,
113.63985943599));
#51017=CARTESIAN_POINT('Ctrl Pts',(-4.92013737328565,0.00435641712180083,
112.235140564009));
#51018=CARTESIAN_POINT('Ctrl Pts',(-4.90797477458816,-1.31335596428614,
112.309859449416));
#51019=CARTESIAN_POINT('Ctrl Pts',(-3.68324102270088,-4.28773323820959,
112.477386286039));
#51020=CARTESIAN_POINT('Ctrl Pts',(1.34693594561081,-5.65910664861623,112.737721073878));
#51021=CARTESIAN_POINT('Ctrl Pts',(5.48905411228744,-1.92613848265676,113.016144927525));
#51022=CARTESIAN_POINT('Ctrl Pts',(4.58778793892862,3.57658025625215,113.294568781172));
#51023=CARTESIAN_POINT('Ctrl Pts',(-0.528772413221697,5.79311006601865,
113.572992634819));
#51024=CARTESIAN_POINT('Ctrl Pts',(-4.35728148891868,3.22499886036145,113.803183229098));
#51025=CARTESIAN_POINT('Ctrl Pts',(-4.91091180554078,0.79069109385873,113.940565872161));
#51026=CARTESIAN_POINT('Ctrl Pts',(-4.91014665664844,0.0005358099224681,
113.985140564009));
#51027=CARTESIAN_POINT('Origin',(0.,0.,-13.2351405640096));
#51028=CARTESIAN_POINT('',(-4.91104925059525,-0.00220516644860025,110.13985943599));
#51029=CARTESIAN_POINT('',(-4.92470054292969,-0.00258956693979628,110.485140564009));
#51030=CARTESIAN_POINT('',(-4.91825,6.88216836313478E-12,-13.2351405640096));
#51031=CARTESIAN_POINT('Ctrl Pts',(-4.91104925059525,-0.00220516644859954,
110.13985943599));
#51032=CARTESIAN_POINT('Ctrl Pts',(-4.91380230587921,-0.685354792246956,
110.178415329152));
#51033=CARTESIAN_POINT('Ctrl Pts',(-4.4615567037503,-3.00910759707894,110.309760980891));
#51034=CARTESIAN_POINT('Ctrl Pts',(-0.904029340980253,-5.74612625726445,
110.533896391206));
#51035=CARTESIAN_POINT('Ctrl Pts',(4.34464099652475,-3.86772938881385,110.812265666937));
#51036=CARTESIAN_POINT('Ctrl Pts',(5.60285477669039,1.56309128495284,111.090634942667));
#51037=CARTESIAN_POINT('Ctrl Pts',(1.71497050149349,5.55824722307171,111.369004218397));
#51038=CARTESIAN_POINT('Ctrl Pts',(-3.51333726348395,4.49596995217328,111.635412382838));
#51039=CARTESIAN_POINT('Ctrl Pts',(-4.91191922429149,1.41971394224373,111.809030788703));
#51040=CARTESIAN_POINT('Ctrl Pts',(-4.92322087232039,-0.0034344185441413,
111.88985943599));
#51041=CARTESIAN_POINT('Ctrl Pts',(-4.92470054292969,-0.00258956693979698,
110.485140564009));
#51042=CARTESIAN_POINT('Ctrl Pts',(-4.92564256049222,-0.150311071404671,
110.49353712424));
#51043=CARTESIAN_POINT('Ctrl Pts',(-4.85250412977593,-1.92986611247264,
110.594741635686));
#51044=CARTESIAN_POINT('Ctrl Pts',(-2.68989438598306,-5.1579252315488,110.788754098348));
#51045=CARTESIAN_POINT('Ctrl Pts',(2.88512386742743,-5.05131515266979,111.067177951995));
#51046=CARTESIAN_POINT('Ctrl Pts',(5.80926853963687,-0.303518593130995,
111.345601805642));
#51047=CARTESIAN_POINT('Ctrl Pts',(3.39581343955041,4.72315314019781,111.62402565929));
#51048=CARTESIAN_POINT('Ctrl Pts',(-2.13774067438488,5.41015612631201,111.902449512937));
#51049=CARTESIAN_POINT('Ctrl Pts',(-4.7492296217318,2.27590767693226,112.106154481176));
#51050=CARTESIAN_POINT('Ctrl Pts',(-4.923081877169,0.323367947526276,112.217051498201));
#51051=CARTESIAN_POINT('Ctrl Pts',(-4.92013737328565,0.00435641712180083,
112.235140564009));
#51052=CARTESIAN_POINT('Origin',(0.,0.,-13.2351405640096));
#51053=CARTESIAN_POINT('',(-4.91512112114719,0.00426704468460083,108.38985943599));
#51054=CARTESIAN_POINT('',(-4.91210503009247,-0.00308641233103812,108.735140564009));
#51055=CARTESIAN_POINT('',(-4.91825,6.88216836313478E-12,-13.2351405640096));
#51056=CARTESIAN_POINT('Ctrl Pts',(-4.91512112114719,0.00426704468460083,
108.38985943599));
#51057=CARTESIAN_POINT('Ctrl Pts',(-4.90562515227987,-1.14769786247349,
108.455010111025));
#51058=CARTESIAN_POINT('Ctrl Pts',(-3.92619331620162,-3.95487106119495,
108.612950544637));
#51059=CARTESIAN_POINT('Ctrl Pts',(0.756408103882341,-5.76741560789225,
108.863680736825));
#51060=CARTESIAN_POINT('Ctrl Pts',(5.26044902321342,-2.48252131671617,109.142050012555));
#51061=CARTESIAN_POINT('Ctrl Pts',(4.93288399028696,3.08251383648926,109.420419288285));
#51062=CARTESIAN_POINT('Ctrl Pts',(0.0745742349817975,5.81632828314004,
109.698788564016));
#51063=CARTESIAN_POINT('Ctrl Pts',(-4.16983692941391,3.56924743907384,109.938601946584));
#51064=CARTESIAN_POINT('Ctrl Pts',(-4.90717672119688,0.958733404164842,
110.085625570576));
#51065=CARTESIAN_POINT('Ctrl Pts',(-4.91104925059525,-0.00220516644859954,
110.13985943599));
#51066=CARTESIAN_POINT('Ctrl Pts',(-4.91210503009247,-0.00308641233103826,
108.735140564009));
#51067=CARTESIAN_POINT('Ctrl Pts',(-4.91563471133498,-0.620811093111574,
108.770022750279));
#51068=CARTESIAN_POINT('Ctrl Pts',(-4.52057645045832,-2.87771128788229,
108.897712887764));
#51069=CARTESIAN_POINT('Ctrl Pts',(-1.1295941498845,-5.70646489155393,109.118210976465));
#51070=CARTESIAN_POINT('Ctrl Pts',(4.19009293312384,-4.03520082694487,109.396634830112));
#51071=CARTESIAN_POINT('Ctrl Pts',(5.65989100977229,1.34363620801531,109.675058683759));
#51072=CARTESIAN_POINT('Ctrl Pts',(1.92933851580168,5.48793015566298,109.953482537407));
#51073=CARTESIAN_POINT('Ctrl Pts',(-3.40794084750014,4.61695561495044,110.223509830823));
#51074=CARTESIAN_POINT('Ctrl Pts',(-4.91523035387596,1.48246828148492,110.400729173024));
#51075=CARTESIAN_POINT('Ctrl Pts',(-4.92470054292969,-0.00258956693979698,
110.485140564009));
#51076=CARTESIAN_POINT('Origin',(0.,0.,-13.2351405640096));
#51077=CARTESIAN_POINT('',(-4.92634169465701,0.000345390489136179,106.639859435991));
#51078=CARTESIAN_POINT('',(-4.91340451049185,0.00375331177323163,106.985140564009));
#51079=CARTESIAN_POINT('',(-4.91825,6.88216836313478E-12,-13.2351405640096));
#51080=CARTESIAN_POINT('Ctrl Pts',(-4.92634169465701,0.000345390489136449,
106.639859435991));
#51081=CARTESIAN_POINT('Ctrl Pts',(-4.92471495268435,-1.61231162362228,
106.731604892898));
#51082=CARTESIAN_POINT('Ctrl Pts',(-3.17949842752432,-4.85899970765747,
106.916140108382));
#51083=CARTESIAN_POINT('Ctrl Pts',(2.35519976353486,-5.31867183492482,107.193465082443));
#51084=CARTESIAN_POINT('Ctrl Pts',(5.74754071419879,-0.894992599078435,
107.471834358174));
#51085=CARTESIAN_POINT('Ctrl Pts',(3.860892779499,4.35071752231632,107.750203633904));
#51086=CARTESIAN_POINT('Ctrl Pts',(-1.57189968623559,5.60038993197703,108.028572909634));
#51087=CARTESIAN_POINT('Ctrl Pts',(-4.62732659044495,2.61763360948482,108.24179151033));
#51088=CARTESIAN_POINT('Ctrl Pts',(-4.91914962701757,0.492968877619891,
108.362220352448));
#51089=CARTESIAN_POINT('Ctrl Pts',(-4.91512112114719,0.00426704468460083,
108.38985943599));
#51090=CARTESIAN_POINT('Ctrl Pts',(-4.91340451049185,0.00375331177323107,
106.985140564009));
#51091=CARTESIAN_POINT('Ctrl Pts',(-4.90572611028794,-1.08228077601355,
107.046508376318));
#51092=CARTESIAN_POINT('Ctrl Pts',(-4.0144761831106,-3.82219628726396,107.200684139842));
#51093=CARTESIAN_POINT('Ctrl Pts',(0.522016777754955,-5.79372272254491,
107.447667854582));
#51094=CARTESIAN_POINT('Ctrl Pts',(5.15635602784475,-2.69290122657703,107.72609170823));
#51095=CARTESIAN_POINT('Ctrl Pts',(5.05299644850137,2.88217823762239,108.004515561877));
#51096=CARTESIAN_POINT('Ctrl Pts',(0.306905601200556,5.8090905875139,108.282939415524));
#51097=CARTESIAN_POINT('Ctrl Pts',(-4.09123231337672,3.7005678919498,108.526481082901));
#51098=CARTESIAN_POINT('Ctrl Pts',(-4.9062436002954,1.02271438993413,108.677214799063));
#51099=CARTESIAN_POINT('Ctrl Pts',(-4.91210503009247,-0.00308641233103826,
108.735140564009));
#51100=CARTESIAN_POINT('Origin',(0.,0.,-13.2351405640096));
#51101=CARTESIAN_POINT('',(-4.9161599573824,-0.00444126794963291,104.88985943599));
#51102=CARTESIAN_POINT('',(-4.92575191546683,0.00160007646054477,105.235140564009));
#51103=CARTESIAN_POINT('',(-4.91825,6.88216836313478E-12,-13.2351405640096));
#51104=CARTESIAN_POINT('Ctrl Pts',(-4.9161599573824,-0.00444126794963244,
104.88985943599));
#51105=CARTESIAN_POINT('Ctrl Pts',(-4.92009810546701,-0.455971562148408,
104.915409916194));
#51106=CARTESIAN_POINT('Ctrl Pts',(-4.65577396722329,-2.5427641382639,105.033750154974));
#51107=CARTESIAN_POINT('Ctrl Pts',(-1.69748166270338,-5.56361321611808,
105.244880152331));
#51108=CARTESIAN_POINT('Ctrl Pts',(3.76204723591069,-4.43646668065416,105.523249428062));
#51109=CARTESIAN_POINT('Ctrl Pts',(5.76621904666208,0.765476269840323,105.801618703792));
#51110=CARTESIAN_POINT('Ctrl Pts',(2.47424633725344,5.26434621547303,106.079987979522));
#51111=CARTESIAN_POINT('Ctrl Pts',(-3.0902668487708,4.92803072404851,106.358357255252));
#51112=CARTESIAN_POINT('Ctrl Pts',(-4.91794174754249,1.66805361794024,106.544981074075));
#51113=CARTESIAN_POINT('Ctrl Pts',(-4.9263602112072,0.0187016172552051,
106.638815134321));
#51114=CARTESIAN_POINT('Ctrl Pts',(-4.92634169465701,0.000345390489136449,
106.639859435991));
#51115=CARTESIAN_POINT('Ctrl Pts',(-4.92575191546683,0.00160007646054441,
105.235140564009));
#51116=CARTESIAN_POINT('Ctrl Pts',(-4.91921010578824,-1.54314000607646,
105.322994002357));
#51117=CARTESIAN_POINT('Ctrl Pts',(-3.30286425710867,-4.73153004719997,
105.50365539192));
#51118=CARTESIAN_POINT('Ctrl Pts',(2.13143050299427,-5.4126452417369,105.7771247327));
#51119=CARTESIAN_POINT('Ctrl Pts',(5.70580531843759,-1.13292107848706,106.055548586347));
#51120=CARTESIAN_POINT('Ctrl Pts',(4.03764314998017,4.18773952095986,106.333972439994));
#51121=CARTESIAN_POINT('Ctrl Pts',(-1.34033601366353,5.66067344690254,106.612396293641));
#51122=CARTESIAN_POINT('Ctrl Pts',(-4.57287513429699,2.75426175018904,106.829452334979));
#51123=CARTESIAN_POINT('Ctrl Pts',(-4.91733833116936,0.560153504204194,
106.953700425102));
#51124=CARTESIAN_POINT('Ctrl Pts',(-4.91340451049185,0.00375331177323107,
106.985140564009));
#51125=CARTESIAN_POINT('Origin',(0.,0.,-13.2351405640096));
#51126=CARTESIAN_POINT('',(-4.9106152160553,0.00164937912531336,103.13985943599));
#51127=CARTESIAN_POINT('',(-4.91828094548546,-0.00453972600810759,103.485140564009));
#51128=CARTESIAN_POINT('',(-4.91825,6.88216836313478E-12,-13.2351405640096));
#51129=CARTESIAN_POINT('Ctrl Pts',(-4.9106152160553,0.00164937912531374,
103.13985943599));
#51130=CARTESIAN_POINT('Ctrl Pts',(-4.90784427716826,-0.92248639834868,
103.192004698067));
#51131=CARTESIAN_POINT('Ctrl Pts',(-4.21255514724753,-3.49494162507719,
103.33693971872));
#51132=CARTESIAN_POINT('Ctrl Pts',(-0.0562818588867149,-5.81653405097377,
103.57466449795));
#51133=CARTESIAN_POINT('Ctrl Pts',(4.86229519584828,-3.19269814454921,103.85303377368));
#51134=CARTESIAN_POINT('Ctrl Pts',(5.31496177293694,2.36356031570952,104.13140304941));
#51135=CARTESIAN_POINT('Ctrl Pts',(0.885953644154715,5.74894095935824,104.409772325141));
#51136=CARTESIAN_POINT('Ctrl Pts',(-3.87557197153686,4.02797192499425,104.662591120667));
#51137=CARTESIAN_POINT('Ctrl Pts',(-4.90579622906001,1.18381707019861,104.822620157617));
#51138=CARTESIAN_POINT('Ctrl Pts',(-4.9161599573824,-0.00444126794963244,
104.88985943599));
#51139=CARTESIAN_POINT('Ctrl Pts',(-4.91828094548546,-0.0045397260081078,
103.485140564009));
#51140=CARTESIAN_POINT('Ctrl Pts',(-4.92179757162394,-0.3846215820958,103.50667167718));
#51141=CARTESIAN_POINT('Ctrl Pts',(-4.70766588298512,-2.39909247163602,
103.621010741567));
#51142=CARTESIAN_POINT('Ctrl Pts',(-1.93573661342329,-5.48567664608875,
103.82815775717));
#51143=CARTESIAN_POINT('Ctrl Pts',(3.56855014082175,-4.59403682989503,104.106581610817));
#51144=CARTESIAN_POINT('Ctrl Pts',(5.79402609657907,0.518638693265626,104.385005464464));
#51145=CARTESIAN_POINT('Ctrl Pts',(2.69590715174485,5.15478507128686,104.663429318111));
#51146=CARTESIAN_POINT('Ctrl Pts',(-2.87923162804837,5.05467602661504,104.941853171758));
#51147=CARTESIAN_POINT('Ctrl Pts',(-4.88448420473077,1.80732804898653,105.132423587058));
#51148=CARTESIAN_POINT('Ctrl Pts',(-4.92612084217979,0.0887160136435684,
105.230186051141));
#51149=CARTESIAN_POINT('Ctrl Pts',(-4.92575191546683,0.00160007646054441,
105.235140564009));
#51150=CARTESIAN_POINT('Origin',(0.,0.,-13.2351405640096));
#51151=CARTESIAN_POINT('',(-4.92222608014563,0.00382897363343741,101.389859435991));
#51152=CARTESIAN_POINT('',(-4.91013498857969,0.0004726267068067,101.735140564009));
#51153=CARTESIAN_POINT('',(-4.91825,6.88216836313478E-12,-13.2351405640096));
#51154=CARTESIAN_POINT('Ctrl Pts',(-4.92222608014563,0.0038289736334372,
101.389859435991));
#51155=CARTESIAN_POINT('Ctrl Pts',(-4.91033810900471,-1.38327561748898,
101.46859947994));
#51156=CARTESIAN_POINT('Ctrl Pts',(-3.57279275371078,-4.42504846667363,
101.640129282465));
#51157=CARTESIAN_POINT('Ctrl Pts',(1.58950480666019,-5.5954187049212,101.904448843568));
#51158=CARTESIAN_POINT('Ctrl Pts',(5.56627558047574,-1.68873093652502,102.182818119298));
#51159=CARTESIAN_POINT('Ctrl Pts',(4.43054548072448,3.76901880560565,102.461187395029));
#51160=CARTESIAN_POINT('Ctrl Pts',(-0.774542543027661,5.76500822747185,
102.739556670759));
#51161=CARTESIAN_POINT('Ctrl Pts',(-4.42645455217522,3.08395535649196,102.965780684413));
#51162=CARTESIAN_POINT('Ctrl Pts',(-4.91277501756771,0.72196474197561,103.09921493949));
#51163=CARTESIAN_POINT('Ctrl Pts',(-4.9106152160553,0.00164937912531374,
103.13985943599));
#51164=CARTESIAN_POINT('Ctrl Pts',(-4.91013498857969,0.000472626706806561,
101.735140564009));
#51165=CARTESIAN_POINT('Ctrl Pts',(-4.90940804483265,-0.85070330671101,
101.783157303219));
#51166=CARTESIAN_POINT('Ctrl Pts',(-4.29337995317973,-3.34803870942995,
101.923981993645));
#51167=CARTESIAN_POINT('Ctrl Pts',(-0.313679303199746,-5.8087287590948,
102.157614635287));
#51168=CARTESIAN_POINT('Ctrl Pts',(4.71720619091674,-3.40406966062208,102.436038488934));
#51169=CARTESIAN_POINT('Ctrl Pts',(5.41388703969527,2.12827432992347,102.714462342581));
#51170=CARTESIAN_POINT('Ctrl Pts',(1.13624762196393,5.70514380568731,102.992886196228));
#51171=CARTESIAN_POINT('Ctrl Pts',(-3.77385145643153,4.16884673512571,103.249778936704));
#51172=CARTESIAN_POINT('Ctrl Pts',(-4.90663946695428,1.25368750472487,103.413863725964));
#51173=CARTESIAN_POINT('Ctrl Pts',(-4.91828094548546,-0.0045397260081078,
103.485140564009));
#51174=CARTESIAN_POINT('Origin',(0.,0.,-13.2351405640096));
#51175=CARTESIAN_POINT('',(-4.92295084975763,-0.00355279698548788,99.6398594359904));
#51176=CARTESIAN_POINT('',(-4.92002136431585,0.00437517423019299,99.9851405640091));
#51177=CARTESIAN_POINT('',(-4.91825,6.88216836313478E-12,-13.2351405640096));
#51178=CARTESIAN_POINT('Ctrl Pts',(-4.92295084975763,-0.0035527969854883,
99.6398594359904));
#51179=CARTESIAN_POINT('Ctrl Pts',(-4.92474865037419,-0.224465174800093,
99.6524045032355));
#51180=CARTESIAN_POINT('Ctrl Pts',(-4.81074196999753,-2.07749203204646,
99.7577393290575));
#51181=CARTESIAN_POINT('Ctrl Pts',(-2.4576780448157,-5.27210153940609,99.9558639134564));
#51182=CARTESIAN_POINT('Ctrl Pts',(3.10574993054631,-4.91828764741234,100.234233189186));
#51183=CARTESIAN_POINT('Ctrl Pts',(5.81661536145012,-0.0471354507815979,
100.512602464917));
#51184=CARTESIAN_POINT('Ctrl Pts',(3.18504837292365,4.8673096137306,100.790971740647));
#51185=CARTESIAN_POINT('Ctrl Pts',(-2.3719150235782,5.3112385687993,101.069341016377));
#51186=CARTESIAN_POINT('Ctrl Pts',(-4.79470318360075,2.13121410472449,101.268970248158));
#51187=CARTESIAN_POINT('Ctrl Pts',(-4.92434727024986,0.251332311027171,
101.375809721363));
#51188=CARTESIAN_POINT('Ctrl Pts',(-4.92222608014563,0.0038289736334372,
101.389859435991));
#51189=CARTESIAN_POINT('Ctrl Pts',(-4.92002136431585,0.00437517423019302,
99.9851405640091));
#51190=CARTESIAN_POINT('Ctrl Pts',(-4.90787315670411,-1.30959848678255,
100.059642929258));
#51191=CARTESIAN_POINT('Ctrl Pts',(-3.68904982626242,-4.28028194088868,
100.226953245723));
#51192=CARTESIAN_POINT('Ctrl Pts',(1.33373425917899,-5.66223254802231,100.487071513404));
#51193=CARTESIAN_POINT('Ctrl Pts',(5.48454709390498,-1.93893467572513,100.765495367051));
#51194=CARTESIAN_POINT('Ctrl Pts',(4.59611667109638,3.56587100827567,101.043919220699));
#51195=CARTESIAN_POINT('Ctrl Pts',(-0.515260432469941,5.79432750098943,
101.322343074346));
#51196=CARTESIAN_POINT('Ctrl Pts',(-4.353355146971,3.23274483753813,101.552750188783));
#51197=CARTESIAN_POINT('Ctrl Pts',(-4.91081309983891,0.794470768077152,
101.690349352004));
#51198=CARTESIAN_POINT('Ctrl Pts',(-4.91013498857969,0.000472626706806561,
101.735140564009));
#51199=CARTESIAN_POINT('Origin',(0.,0.,-13.2351405640096));
#51200=CARTESIAN_POINT('',(-4.91091515388363,-0.00205329971730024,97.8898594359905));
#51201=CARTESIAN_POINT('',(-4.92477872676417,-0.00253174555402969,98.235140564009));
#51202=CARTESIAN_POINT('',(-4.91825,6.88216836313478E-12,-13.2351405640096));
#51203=CARTESIAN_POINT('Ctrl Pts',(-4.91091515388363,-0.00205329971729964,
97.8898594359905));
#51204=CARTESIAN_POINT('Ctrl Pts',(-4.91351335274079,-0.695597017619058,
97.9289992851084));
#51205=CARTESIAN_POINT('Ctrl Pts',(-4.45185496108958,-3.03003808629795,
98.0609288928032));
#51206=CARTESIAN_POINT('Ctrl Pts',(-0.867869184648594,-5.75169880053843,
98.2856482590747));
#51207=CARTESIAN_POINT('Ctrl Pts',(4.36888249237581,-3.84032573899534,98.5640175348048));
#51208=CARTESIAN_POINT('Ctrl Pts',(5.59291233487078,1.5983014822703,98.8423868105353));
#51209=CARTESIAN_POINT('Ctrl Pts',(1.67997603467162,5.56892418126753,99.1207560862653));
#51210=CARTESIAN_POINT('Ctrl Pts',(-3.53010137522744,4.47618315698173,99.3865802947507));
#51211=CARTESIAN_POINT('Ctrl Pts',(-4.91145119393814,1.4095161983887,99.5596147446588));
#51212=CARTESIAN_POINT('Ctrl Pts',(-4.92295084975763,-0.0035527969854883,
99.6398594359904));
#51213=CARTESIAN_POINT('Ctrl Pts',(-4.92477872676416,-0.00253174555403059,
98.235140564009));
#51214=CARTESIAN_POINT('Ctrl Pts',(-4.92567969671966,-0.146437961420724,
98.2433206040817));
#51215=CARTESIAN_POINT('Ctrl Pts',(-4.85458662833453,-1.9221521487663,98.3443085953702));
#51216=CARTESIAN_POINT('Ctrl Pts',(-2.70191625171569,-5.15163790174596,
98.5381045378744));
#51217=CARTESIAN_POINT('Ctrl Pts',(2.87333547360048,-5.05803002740593,98.8165283915213));
#51218=CARTESIAN_POINT('Ctrl Pts',(5.80854488292173,-0.31706599482648,99.0949522451687));
#51219=CARTESIAN_POINT('Ctrl Pts',(3.40681942119772,4.71522066645252,99.3733760988158));
#51220=CARTESIAN_POINT('Ctrl Pts',(-2.12511743336623,5.41512699725444,99.6517999524627));
#51221=CARTESIAN_POINT('Ctrl Pts',(-4.74669243361833,2.28365257603715,99.8557214408607));
#51222=CARTESIAN_POINT('Ctrl Pts',(-4.92300623678305,0.327224760665144,
99.9668349780427));
#51223=CARTESIAN_POINT('Ctrl Pts',(-4.92002136431585,0.00437517423019302,
99.9851405640091));
#51224=CARTESIAN_POINT('Origin',(0.,0.,-13.2351405640096));
#51225=CARTESIAN_POINT('',(-4.91540576548025,0.004324049150998,96.1398594359904));
#51226=CARTESIAN_POINT('',(-4.91217854052457,-0.00313320867413813,96.485140564009));
#51227=CARTESIAN_POINT('',(-4.91825,6.88216836313478E-12,-13.2351405640096));
#51228=CARTESIAN_POINT('Ctrl Pts',(-4.91540576548025,0.00432404915099827,
96.1398594359904));
#51229=CARTESIAN_POINT('Ctrl Pts',(-4.90565543805024,-1.1577958144934,96.2055940669812));
#51230=CARTESIAN_POINT('Ctrl Pts',(-3.91217231939379,-3.97533522155579,
96.3641184565489));
#51231=CARTESIAN_POINT('Ctrl Pts',(0.792669321423524,-5.76254382722172,
96.6154326046929));
#51232=CARTESIAN_POINT('Ctrl Pts',(5.27595965190304,-2.44938477280896,96.8938018804233));
#51233=CARTESIAN_POINT('Ctrl Pts',(4.91339786110621,3.11347996175579,97.1721711561536));
#51234=CARTESIAN_POINT('Ctrl Pts',(0.0379889261259919,5.81668228935273,
97.4505404318838));
#51235=CARTESIAN_POINT('Ctrl Pts',(-4.18190377251469,3.5484858234407,97.6897698584961));
#51236=CARTESIAN_POINT('Ctrl Pts',(-4.90735374175294,0.948603345866484,
97.8362095265317));
#51237=CARTESIAN_POINT('Ctrl Pts',(-4.91091515388363,-0.00205329971729964,
97.8898594359905));
#51238=CARTESIAN_POINT('Ctrl Pts',(-4.91217854052457,-0.00313320867413834,
96.485140564009));
#51239=CARTESIAN_POINT('Ctrl Pts',(-4.91574274650194,-0.617000532358035,
96.5198062301208));
#51240=CARTESIAN_POINT('Ctrl Pts',(-4.52395216156159,-2.86994616856643,
96.6472798474483));
#51241=CARTESIAN_POINT('Ctrl Pts',(-1.14289954901735,-5.70381496218517,
96.8675614159915));
#51242=CARTESIAN_POINT('Ctrl Pts',(4.18067074617859,-4.04496188041834,97.1459852696388));
#51243=CARTESIAN_POINT('Ctrl Pts',(5.66300921148187,1.33043270129022,97.4244091232857));
#51244=CARTESIAN_POINT('Ctrl Pts',(1.94213207890468,5.4834156773019,97.702832976933));
#51245=CARTESIAN_POINT('Ctrl Pts',(-3.40144532435673,4.62420256715795,97.9730767905073));
#51246=CARTESIAN_POINT('Ctrl Pts',(-4.91545759818065,1.4862729963575,98.150512652866));
#51247=CARTESIAN_POINT('Ctrl Pts',(-4.92477872676416,-0.00253174555403059,
98.235140564009));
#51248=CARTESIAN_POINT('Origin',(0.,0.,-13.2351405640096));
#51249=CARTESIAN_POINT('',(-4.92636580856042,0.000152401533172132,94.3898594359904));
#51250=CARTESIAN_POINT('',(-4.91331497134253,0.00371651414183716,94.7351405640091));
#51251=CARTESIAN_POINT('',(-4.91825,6.88216836313478E-12,-13.2351405640096));
#51252=CARTESIAN_POINT('Ctrl Pts',(-4.92636580856042,0.000152401533172267,
94.3898594359904));
#51253=CARTESIAN_POINT('Ctrl Pts',(-4.9256315120383,-1.6227476720123,94.482188848854));
#51254=CARTESIAN_POINT('Ctrl Pts',(-3.16053327954862,-4.87800756232656,
94.6673080202944));
#51255=CARTESIAN_POINT('Ctrl Pts',(2.38860682377799,-5.30375277093297,94.9452169503114));
#51256=CARTESIAN_POINT('Ctrl Pts',(5.75305638973991,-0.858823724782912,
95.2235862260417));
#51257=CARTESIAN_POINT('Ctrl Pts',(3.83345104448049,4.37491589671717,95.5019555017719));
#51258=CARTESIAN_POINT('Ctrl Pts',(-1.60709420580738,5.59039213539071,95.7803247775023));
#51259=CARTESIAN_POINT('Ctrl Pts',(-4.63538302620171,2.59669818368088,95.9929594222416));
#51260=CARTESIAN_POINT('Ctrl Pts',(-4.91941881535439,0.482630547677397,
96.1128043084044));
#51261=CARTESIAN_POINT('Ctrl Pts',(-4.91540576548025,0.00432404915099827,
96.1398594359904));
#51262=CARTESIAN_POINT('Ctrl Pts',(-4.91331497134253,0.00371651414183681,
94.7351405640091));
#51263=CARTESIAN_POINT('Ctrl Pts',(-4.9057476635683,-1.07853539604368,94.7962918561599));
#51264=CARTESIAN_POINT('Ctrl Pts',(-4.0194063842934,-3.81456105823947,94.9502510995264));
#51265=CARTESIAN_POINT('Ctrl Pts',(0.508503386553553,-5.7949244005297,95.1970182941089));
#51266=CARTESIAN_POINT('Ctrl Pts',(5.15006168983296,-2.70491942447578,95.4754421477558));
#51267=CARTESIAN_POINT('Ctrl Pts',(5.05970444894282,2.87038593073113,95.7538660014031));
#51268=CARTESIAN_POINT('Ctrl Pts',(0.320452578669648,5.80835903218928,96.0322898550501));
#51269=CARTESIAN_POINT('Ctrl Pts',(-4.08650533321589,3.7082338422809,96.2760480425855));
#51270=CARTESIAN_POINT('Ctrl Pts',(-4.90620054836839,1.02646330432835,96.4269982789051));
#51271=CARTESIAN_POINT('Ctrl Pts',(-4.91217854052457,-0.00313320867413834,
96.485140564009));
#51272=CARTESIAN_POINT('Origin',(0.,0.,-13.2351405640096));
#51273=CARTESIAN_POINT('',(-4.91586394481066,-0.0044009184501047,92.6398594359905));
#51274=CARTESIAN_POINT('',(-4.92569885802918,0.00166625634000921,92.985140564009));
#51275=CARTESIAN_POINT('',(-4.91825,6.88216836313478E-12,-13.2351405640096));
#51276=CARTESIAN_POINT('Ctrl Pts',(-4.91586394481065,-0.00440091845010419,
92.6398594359905));
#51277=CARTESIAN_POINT('Ctrl Pts',(-4.91983703663366,-0.466321471806239,
92.66599387215));
#51278=CARTESIAN_POINT('Ctrl Pts',(-4.64792287731085,-2.56369434537738,
92.7849180668864));
#51279=CARTESIAN_POINT('Ctrl Pts',(-1.66245379054078,-5.57418006599121,
92.9966320201996));
#51280=CARTESIAN_POINT('Ctrl Pts',(3.78987752860088,-4.41271620795891,93.2750012959297));
#51281=CARTESIAN_POINT('Ctrl Pts',(5.76129025225566,0.801729781810469,93.5533705716601));
#51282=CARTESIAN_POINT('Ctrl Pts',(2.44108544428034,5.27980471868994,93.8317398473903));
#51283=CARTESIAN_POINT('Ctrl Pts',(-3.12120229435501,4.90849592558558,94.1101091231206));
#51284=CARTESIAN_POINT('Ctrl Pts',(-4.92268165233641,1.64732391744147,94.2961489859873));
#51285=CARTESIAN_POINT('Ctrl Pts',(-4.92636946969337,0.00824402768593246,
94.3893990902772));
#51286=CARTESIAN_POINT('Ctrl Pts',(-4.92636580856042,0.000152401533172267,
94.3898594359904));
#51287=CARTESIAN_POINT('Ctrl Pts',(-4.92569885802918,0.00166625634000918,
92.985140564009));
#51288=CARTESIAN_POINT('Ctrl Pts',(-4.918936253497,-1.5393109239517,93.0727774821989));
#51289=CARTESIAN_POINT('Ctrl Pts',(-3.30958867840564,-4.72436363233033,
93.2532223516047));
#51290=CARTESIAN_POINT('Ctrl Pts',(2.11880147408499,-5.4176013894902,93.526475172226));
#51291=CARTESIAN_POINT('Ctrl Pts',(5.70314763188498,-1.14622493033275,93.8048990258731));
#51292=CARTESIAN_POINT('Ctrl Pts',(4.04739870824418,4.17831164449162,94.0833228795204));
#51293=CARTESIAN_POINT('Ctrl Pts',(-1.32713069113358,5.66378394985563,94.3617467331672));
#51294=CARTESIAN_POINT('Ctrl Pts',(-4.56967059078738,2.76202729401532,94.5790192946638));
#51295=CARTESIAN_POINT('Ctrl Pts',(-4.91723239767682,0.563974172450816,
94.7034839049442));
#51296=CARTESIAN_POINT('Ctrl Pts',(-4.91331497134253,0.00371651414183681,
94.7351405640091));
#51297=CARTESIAN_POINT('Origin',(0.,0.,-13.2351405640096));
#51298=CARTESIAN_POINT('',(-4.9107237361743,0.00180815062061624,90.8898594359904));
#51299=CARTESIAN_POINT('',(-4.9183976868952,-0.00453542631586867,91.235140564009));
#51300=CARTESIAN_POINT('',(-4.91825,6.88216836313478E-12,-13.2351405640096));
#51301=CARTESIAN_POINT('Ctrl Pts',(-4.9107237361743,0.00180815062061683,
90.8898594359904));
#51302=CARTESIAN_POINT('Ctrl Pts',(-4.90764819817127,-0.932625139035979,
90.9425886540228));
#51303=CARTESIAN_POINT('Ctrl Pts',(-4.20073444988904,-3.51573031561613,
91.088107630632));
#51304=CARTESIAN_POINT('Ctrl Pts',(-0.0196956176291403,-5.81677299681053,
91.3264163658181));
#51305=CARTESIAN_POINT('Ctrl Pts',(4.88228060641031,-3.16205188035358,91.6047856415481));
#51306=CARTESIAN_POINT('Ctrl Pts',(5.29999019571399,2.3969438748358,91.8831549172785));
#51307=CARTESIAN_POINT('Ctrl Pts',(0.849776141329328,5.75439975352813,92.1615241930086));
#51308=CARTESIAN_POINT('Ctrl Pts',(-3.88985778820703,4.00755963785217,92.4137590325795));
#51309=CARTESIAN_POINT('Ctrl Pts',(-4.90573065879529,1.17371760789,92.5732041135733));
#51310=CARTESIAN_POINT('Ctrl Pts',(-4.91586394481065,-0.00440091845010419,
92.6398594359905));
#51311=CARTESIAN_POINT('Ctrl Pts',(-4.9183976868952,-0.0045354263158684,
91.235140564009));
#51312=CARTESIAN_POINT('Ctrl Pts',(-4.92188327701382,-0.38077228891719,
91.2564551570223));
#51313=CARTESIAN_POINT('Ctrl Pts',(-4.7103583587901,-2.39133984619341,91.3705777012513));
#51314=CARTESIAN_POINT('Ctrl Pts',(-1.94852490354921,-5.48114725237695,
91.5775081966962));
#51315=CARTESIAN_POINT('Ctrl Pts',(3.55782634118013,-4.60234681743952,91.8559320503431));
#51316=CARTESIAN_POINT('Ctrl Pts',(5.79521989545676,0.505124603729757,92.1343559039904));
#51317=CARTESIAN_POINT('Ctrl Pts',(2.70792167772444,5.14848372720567,92.4127797576374));
#51318=CARTESIAN_POINT('Ctrl Pts',(-2.86743541210141,5.06137715048165,92.6912036112847));
#51319=CARTESIAN_POINT('Ctrl Pts',(-4.88254282097151,1.81503039074797,92.8819905467418));
#51320=CARTESIAN_POINT('Ctrl Pts',(-4.92609788679581,0.0925919079470681,
92.9799695309832));
#51321=CARTESIAN_POINT('Ctrl Pts',(-4.92569885802918,0.00166625634000918,
92.985140564009));
#51322=CARTESIAN_POINT('Origin',(0.,0.,-13.2351405640096));
#51323=CARTESIAN_POINT('',(-4.92251196586327,0.00372681388479887,89.1398594359905));
#51324=CARTESIAN_POINT('',(-4.91012478479042,0.000409354062299583,89.485140564009));
#51325=CARTESIAN_POINT('',(-4.91825,6.88216836313478E-12,-13.2351405640096));
#51326=CARTESIAN_POINT('Ctrl Pts',(-4.92251196586327,0.0037268138847989,
89.1398594359905));
#51327=CARTESIAN_POINT('Ctrl Pts',(-4.91075438653713,-1.39345382076143,
89.2191834358957));
#51328=CARTESIAN_POINT('Ctrl Pts',(-3.55631018654717,-4.44491937563105,
89.3912971943777));
#51329=CARTESIAN_POINT('Ctrl Pts',(1.62466770970617,-5.58531027310169,89.6562007114362));
#51330=CARTESIAN_POINT('Ctrl Pts',(5.57678733692693,-1.65368649159043,89.9345699871666));
#51331=CARTESIAN_POINT('Ctrl Pts',(4.40675127502924,3.79681171692856,90.2129392628969));
#51332=CARTESIAN_POINT('Ctrl Pts',(-0.810788259783799,5.76002243151662,
90.4913085386271));
#51333=CARTESIAN_POINT('Ctrl Pts',(-4.43638158111647,3.06303241975059,90.716948596325));
#51334=CARTESIAN_POINT('Ctrl Pts',(-4.91306034800856,0.711735285578314,
90.8497988954461));
#51335=CARTESIAN_POINT('Ctrl Pts',(-4.9107237361743,0.00180815062061683,
90.8898594359904));
#51336=CARTESIAN_POINT('Ctrl Pts',(-4.91012478479042,0.000409354062299305,
89.485140564009));
#51337=CARTESIAN_POINT('Ctrl Pts',(-4.90949807124995,-0.846932791369525,
89.5329407830614));
#51338=CARTESIAN_POINT('Ctrl Pts',(-4.29749360927449,-3.3403057452366,89.6735489533296));
#51339=CARTESIAN_POINT('Ctrl Pts',(-0.327225418400649,-5.80798140730008,
89.9069650748132));
#51340=CARTESIAN_POINT('Ctrl Pts',(4.70925447839735,-3.41506175049384,90.1853889284604));
#51341=CARTESIAN_POINT('Ctrl Pts',(5.41883582332552,2.11564241350824,90.4638127821077));
#51342=CARTESIAN_POINT('Ctrl Pts',(1.14954992199983,5.70247836285427,90.7422366357546));
#51343=CARTESIAN_POINT('Ctrl Pts',(-3.76826016539578,4.17635147584231,90.9993458963886));
#51344=CARTESIAN_POINT('Ctrl Pts',(-4.90670632864398,1.25743738123968,91.1636472058066));
#51345=CARTESIAN_POINT('Ctrl Pts',(-4.9183976868952,-0.0045354263158684,
91.235140564009));
#51346=CARTESIAN_POINT('Origin',(0.,0.,-13.2351405640096));
#51347=CARTESIAN_POINT('',(-4.92267424784073,-0.00366498708994259,87.3898594359905));
#51348=CARTESIAN_POINT('',(-4.91990514195361,0.00439296476756349,87.735140564009));
#51349=CARTESIAN_POINT('',(-4.91825,6.88216836313478E-12,-13.2351405640096));
#51350=CARTESIAN_POINT('Ctrl Pts',(-4.92267424784073,-0.0036649870899429,
87.3898594359905));
#51351=CARTESIAN_POINT('Ctrl Pts',(-4.92459773178982,-0.234894405579778,
87.4029884591917));
#51352=CARTESIAN_POINT('Ctrl Pts',(-4.80457424349024,-2.09833774282285,
87.5089072409697));
#51353=CARTESIAN_POINT('Ctrl Pts',(-2.42446869975928,-5.28745567713485,
87.7076157813245));
#51354=CARTESIAN_POINT('Ctrl Pts',(3.1366237873624,-4.89865565541509,87.9859850570546));
#51355=CARTESIAN_POINT('Ctrl Pts',(5.81679677614137,-0.0105488790210397,
88.2643543327851));
#51356=CARTESIAN_POINT('Ctrl Pts',(3.15437072011317,4.88724680918305,88.5427236085151));
#51357=CARTESIAN_POINT('Ctrl Pts',(-2.40527499904105,5.29621451536529,88.8210928842456));
#51358=CARTESIAN_POINT('Ctrl Pts',(-4.80098485902228,2.11036059073919,89.0201381600706));
#51359=CARTESIAN_POINT('Ctrl Pts',(-4.92450789050092,0.240907204047213,
89.1263936773189));
#51360=CARTESIAN_POINT('Ctrl Pts',(-4.92251196586327,0.0037268138847989,
89.1398594359905));
#51361=CARTESIAN_POINT('Ctrl Pts',(-4.91990514195361,0.00439296476756341,
87.735140564009));
#51362=CARTESIAN_POINT('Ctrl Pts',(-4.90777396943026,-1.30584162754635,
87.8094264091005));
#51363=CARTESIAN_POINT('Ctrl Pts',(-3.69484393042714,-4.27282686419821,
87.9765202054077));
#51364=CARTESIAN_POINT('Ctrl Pts',(1.32052531850694,-5.66532765029288,88.2364219529305));
#51365=CARTESIAN_POINT('Ctrl Pts',(5.48001024482615,-1.95172032284121,88.5148458065777));
#51366=CARTESIAN_POINT('Ctrl Pts',(4.60442040478046,3.5551423653677,88.7932696602248));
#51367=CARTESIAN_POINT('Ctrl Pts',(-0.501745649193681,5.79551342035425,
89.071693513872));
#51368=CARTESIAN_POINT('Ctrl Pts',(-4.34941635491549,3.24049005489256,89.3023171484666));
#51369=CARTESIAN_POINT('Ctrl Pts',(-4.91071488575088,0.798249805180592,
89.4401328318457));
#51370=CARTESIAN_POINT('Ctrl Pts',(-4.91012478479042,0.000409354062299305,
89.485140564009));
#51371=CARTESIAN_POINT('Origin',(0.,0.,-13.2351405640096));
#51372=CARTESIAN_POINT('',(-4.91079088019924,-0.00189858029133678,85.6398594359905));
#51373=CARTESIAN_POINT('',(-4.92485543050125,-0.00247326924054714,85.9851405640091));
#51374=CARTESIAN_POINT('',(-4.91825,6.88216836313478E-12,-13.2351405640096));
#51375=CARTESIAN_POINT('Ctrl Pts',(-4.91079088019924,-0.00189858029133678,
85.6398594359905));
#51376=CARTESIAN_POINT('Ctrl Pts',(-4.91322562087344,-0.705834272848961,
85.6795832410645));
#51377=CARTESIAN_POINT('Ctrl Pts',(-4.7719853585205,-1.40883815722723,85.7193070461385));
#51378=CARTESIAN_POINT('Ctrl Pts',(-4.48226309624073,-2.04412712243916,
85.7590308512125));
#51379=CARTESIAN_POINT('Ctrl Pts',(-3.80550872386488,-3.52808138106679,
85.8518206097893));
#51380=CARTESIAN_POINT('Ctrl Pts',(-2.31859170850729,-4.64256258633989,
85.944610368366));
#51381=CARTESIAN_POINT('Ctrl Pts',(-0.704362227995952,-4.87575758302086,
86.0374001269428));
#51382=CARTESIAN_POINT('Ctrl Pts',(0.909867252515474,-5.10895257970185,
86.1301898855195));
#51383=CARTESIAN_POINT('Ctrl Pts',(2.65140919818075,-4.46086136779037,86.2229796440963));
#51384=CARTESIAN_POINT('Ctrl Pts',(3.72047975084877,-3.2291126614191,86.3157694026731));
#51385=CARTESIAN_POINT('Ctrl Pts',(4.78955030351679,-1.99736395504783,86.4085591612498));
#51386=CARTESIAN_POINT('Ctrl Pts',(5.18614946318774,-0.181957754216804,
86.5013489198265));
#51387=CARTESIAN_POINT('Ctrl Pts',(4.72814345648312,1.38340074148049,86.5941386784033));
#51388=CARTESIAN_POINT('Ctrl Pts',(4.27013744977847,2.94875923717787,86.6869284369801));
#51389=CARTESIAN_POINT('Ctrl Pts',(2.95752627669819,4.26407002774135,86.7797181955569));
#51390=CARTESIAN_POINT('Ctrl Pts',(1.39311208672304,4.72529119424815,86.8725079541337));
#51391=CARTESIAN_POINT('Ctrl Pts',(-0.17130210325193,5.18651236075489,86.9652977127104));
#51392=CARTESIAN_POINT('Ctrl Pts',(-1.98751931012186,4.793643903205,87.0580874712871));
#51393=CARTESIAN_POINT('Ctrl Pts',(-3.22146188874805,3.72710631133011,87.1508772298639));
#51394=CARTESIAN_POINT('Ctrl Pts',(-4.2808112688118,2.81147542514635,87.2305379652394));
#51395=CARTESIAN_POINT('Ctrl Pts',(-4.91100345226673,1.39932632727122,87.3101987006149));
#51396=CARTESIAN_POINT('Ctrl Pts',(-4.92267424784073,-0.00366498708994259,
87.3898594359905));
#51397=CARTESIAN_POINT('Ctrl Pts',(-4.92485543050125,-0.00247326924054743,
85.9851405640091));
#51398=CARTESIAN_POINT('Ctrl Pts',(-4.92571589835969,-0.142564623586291,
85.9931040839239));
#51399=CARTESIAN_POINT('Ctrl Pts',(-4.85665955234442,-1.91443894856322,
86.0938755550544));
#51400=CARTESIAN_POINT('Ctrl Pts',(-2.71392342160519,-5.14532255195471,
86.2874549774007));
#51401=CARTESIAN_POINT('Ctrl Pts',(2.86153145157372,-5.06471739129104,86.5658788310476));
#51402=CARTESIAN_POINT('Ctrl Pts',(5.80778963327165,-0.330611671985869,
86.844302684695));
#51403=CARTESIAN_POINT('Ctrl Pts',(3.4178068730022,4.70726254641164,87.1227265383419));
#51404=CARTESIAN_POINT('Ctrl Pts',(-2.11248263373895,5.42006841507948,87.4011503919893));
#51405=CARTESIAN_POINT('Ctrl Pts',(-4.74414493672689,2.29139803765962,87.6052884005448));
#51406=CARTESIAN_POINT('Ctrl Pts',(-4.92292987519333,0.331081099453985,
87.7166184578847));
#51407=CARTESIAN_POINT('Ctrl Pts',(-4.91990514195361,0.00439296476756341,
87.735140564009));
#51408=CARTESIAN_POINT('Origin',(0.,0.,-13.2351405640096));
#51409=CARTESIAN_POINT('',(-4.91569510392104,0.00437467045132868,83.8898594359905));
#51410=CARTESIAN_POINT('',(-4.91225321192224,-0.00317939731315275,84.235140564009));
#51411=CARTESIAN_POINT('',(-4.91825,6.88216836313478E-12,-13.2351405640096));
#51412=CARTESIAN_POINT('Ctrl Pts',(-4.91569510392104,0.00437467045132868,
83.8898594359905));
#51413=CARTESIAN_POINT('Ctrl Pts',(-4.90569919331825,-1.16789416685134,
83.9561780229373));
#51414=CARTESIAN_POINT('Ctrl Pts',(-4.48569639064107,-2.34659643687551,
84.0224966098841));
#51415=CARTESIAN_POINT('Ctrl Pts',(-3.72203604387737,-3.22731867727539,
84.0888151968309));
#51416=CARTESIAN_POINT('Ctrl Pts',(-2.65355943010873,-4.45958262954313,
84.1816049554077));
#51417=CARTESIAN_POINT('Ctrl Pts',(-0.912330125604573,-5.10851334741882,
84.2743947139844));
#51418=CARTESIAN_POINT('Ctrl Pts',(0.702011588476717,-4.87609658295006,
84.3671844725612));
#51419=CARTESIAN_POINT('Ctrl Pts',(2.3163533025581,-4.64367981848129,84.459974231138));
#51420=CARTESIAN_POINT('Ctrl Pts',(3.80380742621645,-3.5299155716678,84.5527639897147));
#51421=CARTESIAN_POINT('Ctrl Pts',(4.48127712058259,-2.04628774251226,84.6455537482915));
#51422=CARTESIAN_POINT('Ctrl Pts',(5.15874681494869,-0.562659913356806,
84.7383435068682));
#51423=CARTESIAN_POINT('Ctrl Pts',(5.02623208002272,1.29083149814077,84.8311332654449));
#51424=CARTESIAN_POINT('Ctrl Pts',(4.14458884076517,2.66299108102481,84.9239230240217));
#51425=CARTESIAN_POINT('Ctrl Pts',(3.26294560150757,4.03515066390892,85.0167127825985));
#51426=CARTESIAN_POINT('Ctrl Pts',(1.6321738579185,4.92597841817944,85.1095025411753));
#51427=CARTESIAN_POINT('Ctrl Pts',(0.00118747916824744,4.92637155993192,
85.202292299752));
#51428=CARTESIAN_POINT('Ctrl Pts',(-1.62979889958191,4.92676470168441,85.2950820583288));
#51429=CARTESIAN_POINT('Ctrl Pts',(-3.2609999134932,4.03672323091877,85.3878718169055));
#51430=CARTESIAN_POINT('Ctrl Pts',(-4.14330455575185,2.6649888395449,85.4806615754822));
#51431=CARTESIAN_POINT('Ctrl Pts',(-4.64788973669743,1.88050147211048,85.533727528985));
#51432=CARTESIAN_POINT('Ctrl Pts',(-4.90753837618641,0.938470013819249,
85.5867934824877));
#51433=CARTESIAN_POINT('Ctrl Pts',(-4.91079088019924,-0.00189858029133678,
85.6398594359905));
#51434=CARTESIAN_POINT('Ctrl Pts',(-4.91225321192224,-0.00317939731315296,
84.235140564009));
#51435=CARTESIAN_POINT('Ctrl Pts',(-4.9158507142751,-0.613189286481138,
84.2695897099629));
#51436=CARTESIAN_POINT('Ctrl Pts',(-4.5273162591334,-2.86218094060655,84.3968468071324));
#51437=CARTESIAN_POINT('Ctrl Pts',(-1.15619873186854,-5.70113400951219,
84.6169118555179));
#51438=CARTESIAN_POINT('Ctrl Pts',(4.1712258203786,-4.05470093316368,84.8953357091649));
#51439=CARTESIAN_POINT('Ctrl Pts',(5.66609661183164,1.31722195828223,85.1737595628121));
#51440=CARTESIAN_POINT('Ctrl Pts',(1.95491507866457,5.47887137439827,85.4521834164592));
#51441=CARTESIAN_POINT('Ctrl Pts',(-3.39493451155719,4.63144433755238,85.7226437501916));
#51442=CARTESIAN_POINT('Ctrl Pts',(-4.91568788814768,1.49007919710422,85.9002961327082));
#51443=CARTESIAN_POINT('Ctrl Pts',(-4.92485543050125,-0.00247326924054743,
85.9851405640091));
#51444=CARTESIAN_POINT('Origin',(0.,0.,-13.2351405640096));
#51445=CARTESIAN_POINT('',(-4.92637127541955,-4.0931223634067E-5,82.1398594359905));
#51446=CARTESIAN_POINT('',(-4.91322641730633,0.00367898483844581,82.4851405640091));
#51447=CARTESIAN_POINT('',(-4.91825,6.88216836313478E-12,-13.2351405640096));
#51448=CARTESIAN_POINT('Ctrl Pts',(-4.92637127541955,-4.09312236341073E-5,
82.1398594359905));
#51449=CARTESIAN_POINT('Ctrl Pts',(-4.92637154201875,-0.00221365673367821,
82.1399830462334));
#51450=CARTESIAN_POINT('Ctrl Pts',(-4.92538488475959,-1.63537294175407,
82.232896415053));
#51451=CARTESIAN_POINT('Ctrl Pts',(-3.13898501948552,-4.89714294882462,
82.4185995424493));
#51452=CARTESIAN_POINT('Ctrl Pts',(2.42191938450794,-5.28862387665468,82.6969688181796));
#51453=CARTESIAN_POINT('Ctrl Pts',(5.75834445937218,-0.822620873182145,
82.9753380939098));
#51454=CARTESIAN_POINT('Ctrl Pts',(3.805857648145,4.39894118803992,83.2537073696402));
#51455=CARTESIAN_POINT('Ctrl Pts',(-1.64222514454274,5.5801731683174,83.5320766453704));
#51456=CARTESIAN_POINT('Ctrl Pts',(-4.64335949870137,2.57576464547258,83.7441273341538));
#51457=CARTESIAN_POINT('Ctrl Pts',(-4.91968498786378,0.472287679719399,
83.8633882643606));
#51458=CARTESIAN_POINT('Ctrl Pts',(-4.91569510392104,0.00437467045132874,
83.8898594359905));
#51459=CARTESIAN_POINT('Ctrl Pts',(-4.91322641730633,0.00367898483844553,
82.4851405640091));
#51460=CARTESIAN_POINT('Ctrl Pts',(-4.90577076072416,-1.07478984285633,
82.546075336002));
#51461=CARTESIAN_POINT('Ctrl Pts',(-4.02432282862942,-3.80692361268266,
82.6998180592107));
#51462=CARTESIAN_POINT('Ctrl Pts',(0.494987229579467,-5.79609455966206,
82.946368733635));
#51463=CARTESIAN_POINT('Ctrl Pts',(5.14373934040566,-2.71692291019715,83.2247925872822));
#51464=CARTESIAN_POINT('Ctrl Pts',(5.06638492942612,2.85857801168262,83.5032164409293));
#51465=CARTESIAN_POINT('Ctrl Pts',(0.333997813182944,5.80759588494068,83.7816402945764));
#51466=CARTESIAN_POINT('Ctrl Pts',(-4.08176482749318,3.71589788202843,84.0256150022698));
#51467=CARTESIAN_POINT('Ctrl Pts',(-4.90615883908873,1.03021192035268,84.1767817587472));
#51468=CARTESIAN_POINT('Ctrl Pts',(-4.91225321192224,-0.00317939731315296,
84.235140564009));
#51469=CARTESIAN_POINT('Origin',(0.,0.,-13.2351405640096));
#51470=CARTESIAN_POINT('',(-4.91557206079122,-0.00435402565801867,80.3898594359905));
#51471=CARTESIAN_POINT('',(-4.92564390538527,0.00173197686021732,80.7351405640091));
#51472=CARTESIAN_POINT('',(-4.91825,6.88216836313478E-12,-13.2351405640096));
#51473=CARTESIAN_POINT('Ctrl Pts',(-4.91557206079122,-0.00435402565801879,
80.3898594359905));
#51474=CARTESIAN_POINT('Ctrl Pts',(-4.91957268173767,-0.476666931688224,
80.4165778281061));
#51475=CARTESIAN_POINT('Ctrl Pts',(-4.63999236043617,-2.5846267150224,80.5360859787985));
#51476=CARTESIAN_POINT('Ctrl Pts',(-1.62736014737243,-5.58452638676924,
80.7483838880677));
#51477=CARTESIAN_POINT('Ctrl Pts',(3.81755788385611,-4.3887911567066,81.0267531637979));
#51478=CARTESIAN_POINT('Ctrl Pts',(5.75613352618714,0.837951575260477,81.3051224395282));
#51479=CARTESIAN_POINT('Ctrl Pts',(2.40782797560329,5.29505433906766,81.5834917152585));
#51480=CARTESIAN_POINT('Ctrl Pts',(-3.14954540178693,4.8889473466839,81.8617373807459));
#51481=CARTESIAN_POINT('Ctrl Pts',(-4.92617141560022,1.62877315225414,82.0471932876566));
#51482=CARTESIAN_POINT('Ctrl Pts',(-4.92637127541955,-4.09312236341073E-5,
82.1398594359905));
#51483=CARTESIAN_POINT('Ctrl Pts',(-4.92564390538527,0.0017319768602176,
80.7351405640091));
#51484=CARTESIAN_POINT('Ctrl Pts',(-4.91866561127433,-1.53548363053209,
80.8225609620411));
#51485=CARTESIAN_POINT('Ctrl Pts',(-3.316297660866,-4.71719158443029,81.0027893112887));
#51486=CARTESIAN_POINT('Ctrl Pts',(2.10616092092011,-5.42252807066782,81.2758256117524));
#51487=CARTESIAN_POINT('Ctrl Pts',(5.7004589256578,-1.15952254780973,81.5542494653993));
#51488=CARTESIAN_POINT('Ctrl Pts',(4.05713225252595,4.16886104199992,81.8326733190467));
#51489=CARTESIAN_POINT('Ctrl Pts',(-1.31391815028062,5.6668636472351,82.1110971726936));
#51490=CARTESIAN_POINT('Ctrl Pts',(-4.56645468057018,2.76979288701375,82.3285862543479));
#51491=CARTESIAN_POINT('Ctrl Pts',(-4.91712625102515,0.567794170749911,
82.4532673847863));
#51492=CARTESIAN_POINT('Ctrl Pts',(-4.91322641730633,0.00367898483844553,
82.4851405640091));
#51493=CARTESIAN_POINT('Origin',(0.,0.,-13.2351405640096));
#51494=CARTESIAN_POINT('',(-4.91084228422721,0.00196441572767522,78.6398594359905));
#51495=CARTESIAN_POINT('',(-4.91851453902819,-0.00453015795356559,78.9851405640091));
#51496=CARTESIAN_POINT('',(-4.91825,6.88216836313478E-12,-13.2351405640096));
#51497=CARTESIAN_POINT('Ctrl Pts',(-4.91084228422721,0.00196441572767485,
78.6398594359905));
#51498=CARTESIAN_POINT('Ctrl Pts',(-4.90745929868568,-0.942760414910041,
78.6931726099789));
#51499=CARTESIAN_POINT('Ctrl Pts',(-4.18881849136433,-3.53650879740012,
78.8392755425441));
#51500=CARTESIAN_POINT('Ctrl Pts',(0.0168914028385561,-5.81678181594319,
79.0781682336861));
#51501=CARTESIAN_POINT('Ctrl Pts',(4.90207286122337,-3.13128051714223,79.3565375094163));
#51502=CARTESIAN_POINT('Ctrl Pts',(5.28480893706208,2.43023260461352,79.6349067851467));
#51503=CARTESIAN_POINT('Ctrl Pts',(0.813565019144324,5.75963088864231,79.9132760608768));
#51504=CARTESIAN_POINT('Ctrl Pts',(-3.9040405862657,3.98712683648866,80.1649269444916));
#51505=CARTESIAN_POINT('Ctrl Pts',(-4.90567900691728,1.16361891835689,80.3237880695294));
#51506=CARTESIAN_POINT('Ctrl Pts',(-4.91557206079122,-0.00435402565801879,
80.3898594359905));
#51507=CARTESIAN_POINT('Ctrl Pts',(-4.91851453902819,-0.00453015795356587,
78.9851405640091));
#51508=CARTESIAN_POINT('Ctrl Pts',(-4.92196835436792,-0.376922461688771,
79.0062386368645));
#51509=CARTESIAN_POINT('Ctrl Pts',(-4.71304029456911,-2.38358769329157,
79.1201446609356));
#51510=CARTESIAN_POINT('Ctrl Pts',(-1.96130259556129,-5.47658804646063,
79.3268586362224));
#51511=CARTESIAN_POINT('Ctrl Pts',(3.54708319036234,-4.61063177261423,79.6052824898694));
#51512=CARTESIAN_POINT('Ctrl Pts',(5.79638217387485,0.491607766798655,79.8837063435167));
#51513=CARTESIAN_POINT('Ctrl Pts',(2.71992147519714,5.14215438029163,80.1621301971638));
#51514=CARTESIAN_POINT('Ctrl Pts',(-2.85562360004527,5.06805074529212,80.4405540508108));
#51515=CARTESIAN_POINT('Ctrl Pts',(-4.88059206529341,1.82273352739509,80.631557506426));
#51516=CARTESIAN_POINT('Ctrl Pts',(-4.92607396440468,0.0964676567022224,
80.7297530108254));
#51517=CARTESIAN_POINT('Ctrl Pts',(-4.92564390538527,0.0017319768602176,
80.7351405640091));
#51518=CARTESIAN_POINT('Origin',(0.,0.,-13.2351405640096));
#51519=CARTESIAN_POINT('',(-4.92279211704217,0.0036182553321711,76.8898594359905));
#51520=CARTESIAN_POINT('',(-4.91011604675776,0.000346003969231568,77.2351405640091));
#51521=CARTESIAN_POINT('',(-4.91825,6.88216836313478E-12,-13.2351405640096));
#51522=CARTESIAN_POINT('Ctrl Pts',(-4.92279211704217,0.00361825533217116,
76.8898594359905));
#51523=CARTESIAN_POINT('Ctrl Pts',(-4.91119054578483,-1.40363931961367,
76.9697673918518));
#51524=CARTESIAN_POINT('Ctrl Pts',(-3.539718546453,-4.46475810474062,77.1424651062897));
#51525=CARTESIAN_POINT('Ctrl Pts',(1.65976633666211,-5.5749808718471,77.4079525793045));
#51526=CARTESIAN_POINT('Ctrl Pts',(5.58707846113262,-1.61857662250689,77.6863218550347));
#51527=CARTESIAN_POINT('Ctrl Pts',(4.38278272676508,3.82445441648177,77.964691130765));
#51528=CARTESIAN_POINT('Ctrl Pts',(-0.847001899642621,5.75480875405768,
78.2430604064953));
#51529=CARTESIAN_POINT('Ctrl Pts',(-4.44622089908048,3.0421063371335,78.4681165082371));
#51530=CARTESIAN_POINT('Ctrl Pts',(-4.91334726948508,0.701500888597644,
78.6003828514022));
#51531=CARTESIAN_POINT('Ctrl Pts',(-4.91084228422721,0.00196441572767485,
78.6398594359905));
#51532=CARTESIAN_POINT('Ctrl Pts',(-4.91011604675776,0.000346003969231637,
77.2351405640091));
#51533=CARTESIAN_POINT('Ctrl Pts',(-4.90958877228912,-0.843161686015328,
77.2827242629036));
#51534=CARTESIAN_POINT('Ctrl Pts',(-4.30159456804404,-3.33257179119856,
77.4231159130138));
#51535=CARTESIAN_POINT('Ctrl Pts',(-0.340769753807865,-5.80720246563535,
77.6563155143396));
#51536=CARTESIAN_POINT('Ctrl Pts',(4.70127715203259,-3.42603526569229,77.9347393679867));
#51537=CARTESIAN_POINT('Ctrl Pts',(5.42375513366596,2.1029989900195,78.2131632216339));
#51538=CARTESIAN_POINT('Ctrl Pts',(1.16284596958247,5.69978190398691,78.4915870752809));
#51539=CARTESIAN_POINT('Ctrl Pts',(-3.76265437325353,4.18385281836137,78.7489128560728));
#51540=CARTESIAN_POINT('Ctrl Pts',(-4.90677542524329,1.26118766311134,78.9134306856488));
#51541=CARTESIAN_POINT('Ctrl Pts',(-4.91851453902819,-0.00453015795356587,
78.9851405640091));
#51542=CARTESIAN_POINT('Origin',(0.,0.,-13.2351405640096));
#51543=CARTESIAN_POINT('',(-4.92239160404736,-0.00377085183543027,75.1398594359906));
#51544=CARTESIAN_POINT('',(-4.91978873044366,0.00440978733039096,75.4851405640091));
#51545=CARTESIAN_POINT('',(-4.91825,6.88216836313478E-12,-13.2351405640096));
#51546=CARTESIAN_POINT('Ctrl Pts',(-4.92239160404736,-0.00377085183543145,
75.1398594359906));
#51547=CARTESIAN_POINT('Ctrl Pts',(-4.92444063379938,-0.245321050757574,
75.1535724151478));
#51548=CARTESIAN_POINT('Ctrl Pts',(-4.79833433295751,-2.11918842723071,
75.2600751528818));
#51549=CARTESIAN_POINT('Ctrl Pts',(-2.39116343640037,-5.30260062933267,
75.4593676491925));
#51550=CARTESIAN_POINT('Ctrl Pts',(3.16737355116417,-4.87882985982939,75.7377369249229));
#51551=CARTESIAN_POINT('Ctrl Pts',(5.81674806318794,0.0260381100804274,
76.016106200653));
#51552=CARTESIAN_POINT('Ctrl Pts',(3.12356827217368,4.90699065241089,76.2944754763835));
#51553=CARTESIAN_POINT('Ctrl Pts',(-2.43853981555445,5.28098092987785,76.5728447521136));
#51554=CARTESIAN_POINT('Ctrl Pts',(-4.80719417250829,2.08951200176882,76.7713060719827));
#51555=CARTESIAN_POINT('Ctrl Pts',(-4.92466238328182,0.23047945150494,76.876977633275));
#51556=CARTESIAN_POINT('Ctrl Pts',(-4.92279211704217,0.00361825533217116,
76.8898594359905));
#51557=CARTESIAN_POINT('Ctrl Pts',(-4.91978873044366,0.00440978733039082,
75.4851405640091));
#51558=CARTESIAN_POINT('Ctrl Pts',(-4.90767719882995,-1.30208537057339,
75.5592098889426));
#51559=CARTESIAN_POINT('Ctrl Pts',(-3.70062334914684,-4.26536803612013,
75.7260871650919));
#51560=CARTESIAN_POINT('Ctrl Pts',(1.30730919543873,-5.66839193859359,75.9857723924568));
#51561=CARTESIAN_POINT('Ctrl Pts',(5.475443589727,-1.96449535446343,76.264196246104));
#51562=CARTESIAN_POINT('Ctrl Pts',(4.61269909481645,3.54439438588181,76.542620099751));
#51563=CARTESIAN_POINT('Ctrl Pts',(-0.488228136900599,5.79666781766301,
76.8210439533983));
#51564=CARTESIAN_POINT('Ctrl Pts',(-4.3454650949107,3.24823449643751,77.0518841081509));
#51565=CARTESIAN_POINT('Ctrl Pts',(-4.91061717622366,0.802028208023915,
77.1899163116879));
#51566=CARTESIAN_POINT('Ctrl Pts',(-4.91011604675776,0.000346003969231637,
77.2351405640091));
#51567=CARTESIAN_POINT('Origin',(0.,0.,-13.2351405640096));
#51568=CARTESIAN_POINT('',(-4.91067656268135,-0.00174122703138476,73.3898594359905));
#51569=CARTESIAN_POINT('',(-4.92493062471777,-0.00241415038567228,73.7351405640091));
#51570=CARTESIAN_POINT('',(-4.91825,6.88216836313478E-12,-13.2351405640096));
#51571=CARTESIAN_POINT('Ctrl Pts',(-4.91067656268135,-0.0017412270313847,
73.3898594359905));
#51572=CARTESIAN_POINT('Ctrl Pts',(-4.91293934412357,-0.716066575557565,
73.4301671970206));
#51573=CARTESIAN_POINT('Ctrl Pts',(-4.43218965357877,-3.07189064286557,
73.5632647166273));
#51574=CARTESIAN_POINT('Ctrl Pts',(-0.795447298431173,-5.7621610190272,
73.7891519948111));
#51575=CARTESIAN_POINT('Ctrl Pts',(4.41684599871641,-3.78506372963529,74.0675212705412));
#51576=CARTESIAN_POINT('Ctrl Pts',(5.57236404275686,1.66853078747969,74.3458905462716));
#51577=CARTESIAN_POINT('Ctrl Pts',(1.60978909543459,5.58961672049141,74.6242598220017));
#51578=CARTESIAN_POINT('Ctrl Pts',(-3.56330145772682,4.43651082739373,74.8889161185748));
#51579=CARTESIAN_POINT('Ctrl Pts',(-4.91057574172695,1.38914396119285,75.0607826565711));
#51580=CARTESIAN_POINT('Ctrl Pts',(-4.92239160404736,-0.00377085183543145,
75.1398594359906));
#51581=CARTESIAN_POINT('Ctrl Pts',(-4.92493062471777,-0.00241415038567332,
73.7351405640091));
#51582=CARTESIAN_POINT('Ctrl Pts',(-4.92575116259624,-0.138691063730488,
73.742887563766));
#51583=CARTESIAN_POINT('Ctrl Pts',(-4.85872291664768,-1.90672651453574,
73.8434425147386));
#51584=CARTESIAN_POINT('Ctrl Pts',(-2.72591583034415,-5.13897921652443,
74.0368054169269));
#51585=CARTESIAN_POINT('Ctrl Pts',(2.84971186554951,-5.07137720795222,74.315229270574));
#51586=CARTESIAN_POINT('Ctrl Pts',(5.80700279479466,-0.344155550933751,
74.5936531242212));
#51587=CARTESIAN_POINT('Ctrl Pts',(3.42877573520264,4.69927882335965,74.8720769778683));
#51588=CARTESIAN_POINT('Ctrl Pts',(-2.09983634422443,5.42498035291051,75.1505008315154));
#51589=CARTESIAN_POINT('Ctrl Pts',(-4.7415871145915,2.29914405580575,75.354855360229));
#51590=CARTESIAN_POINT('Ctrl Pts',(-4.92285279866377,0.334936959346778,
75.4664019377269));
#51591=CARTESIAN_POINT('Ctrl Pts',(-4.91978873044366,0.00440978733039082,
75.4851405640091));
#51592=CARTESIAN_POINT('Origin',(0.,0.,-13.2351405640096));
#51593=CARTESIAN_POINT('',(-4.9159887804262,0.00441880477913321,71.6398594359906));
#51594=CARTESIAN_POINT('',(-4.91232903289984,-0.00322496870272804,71.9851405640091));
#51595=CARTESIAN_POINT('',(-4.91825,6.88216836313478E-12,-13.2351405640096));
#51596=CARTESIAN_POINT('Ctrl Pts',(-4.9159887804262,0.00441880477913298,
71.6398594359906));
#51597=CARTESIAN_POINT('Ctrl Pts',(-4.90575670288894,-1.17799315420249,
71.7067619788934));
#51598=CARTESIAN_POINT('Ctrl Pts',(-3.88382241329164,-4.01620380740258,
71.8664542803729));
#51599=CARTESIAN_POINT('Ctrl Pts',(0.865096242963933,-5.75211652387075,
72.1189363404294));
#51600=CARTESIAN_POINT('Ctrl Pts',(5.30635411174501,-2.38282228765471,72.3973056161595));
#51601=CARTESIAN_POINT('Ctrl Pts',(4.87384322087152,3.17504145990924,72.67567489189));
#51602=CARTESIAN_POINT('Ctrl Pts',(-0.0351847529388852,5.81669992753095,
72.95404416762));
#51603=CARTESIAN_POINT('Ctrl Pts',(-4.20575040548237,3.50693055059452,73.1921056823205));
#51604=CARTESIAN_POINT('Ctrl Pts',(-4.9077303486753,0.92833328544159,73.3373774384439));
#51605=CARTESIAN_POINT('Ctrl Pts',(-4.91067656268135,-0.0017412270313847,
73.3898594359905));
#51606=CARTESIAN_POINT('Ctrl Pts',(-4.91232903289984,-0.00322496870272818,
71.9851405640091));
#51607=CARTESIAN_POINT('Ctrl Pts',(-4.91595860382257,-0.609377356158057,
72.0193731898051));
#51608=CARTESIAN_POINT('Ctrl Pts',(-4.53066876099212,-2.85441561589539,
72.1464137668167));
#51609=CARTESIAN_POINT('Ctrl Pts',(-1.16949162610311,-5.69842204811702,
72.3662622950442));
#51610=CARTESIAN_POINT('Ctrl Pts',(4.16175820709524,-4.06441793220953,72.6446861486912));
#51611=CARTESIAN_POINT('Ctrl Pts',(5.66915319402907,1.30400405084528,72.9231100023384));
#51612=CARTESIAN_POINT('Ctrl Pts',(1.96768744555408,5.47429727166879,73.2015338559855));
#51613=CARTESIAN_POINT('Ctrl Pts',(-3.38840839793359,4.63868089417945,73.4722107098757));
#51614=CARTESIAN_POINT('Ctrl Pts',(-4.91592123594264,1.49388690482925,73.6500796125503));
#51615=CARTESIAN_POINT('Ctrl Pts',(-4.92493062471777,-0.00241415038567332,
73.7351405640091));
#51616=CARTESIAN_POINT('Origin',(0.,0.,-13.2351405640096));
#51617=CARTESIAN_POINT('',(-4.92635784080807,-0.000234171170717763,69.8898594359906));
#51618=CARTESIAN_POINT('',(-4.91313886229116,0.00364073211770066,70.2351405640091));
#51619=CARTESIAN_POINT('',(-4.91825,6.88216836313478E-12,-13.2351405640096));
#51620=CARTESIAN_POINT('Ctrl Pts',(-4.92635784080807,-0.000234171170717511,
69.8898594359906));
#51621=CARTESIAN_POINT('Ctrl Pts',(-4.92636642702435,-0.0126713156829149,
69.8905670021894));
#51622=CARTESIAN_POINT('Ctrl Pts',(-4.9206830606955,-1.65609920609382,69.9840643269651));
#51623=CARTESIAN_POINT('Ctrl Pts',(-3.10812063065928,-4.91678982254146,
70.1703514103174));
#51624=CARTESIAN_POINT('Ctrl Pts',(2.45513612779318,-5.2732857506286,70.4487206860478));
#51625=CARTESIAN_POINT('Ctrl Pts',(5.76340471388584,-0.786385476554853,
70.7270899617779));
#51626=CARTESIAN_POINT('Ctrl Pts',(3.77811368215897,4.42279244578133,71.0054592375083));
#51627=CARTESIAN_POINT('Ctrl Pts',(-1.67729111257008,5.56973343504611,71.2838285132385));
#51628=CARTESIAN_POINT('Ctrl Pts',(-4.65125634837052,2.5548331704508,71.495295246066));
#51629=CARTESIAN_POINT('Ctrl Pts',(-4.91994797220735,0.461940328916346,
71.6139722203167));
#51630=CARTESIAN_POINT('Ctrl Pts',(-4.9159887804262,0.00441880477913298,
71.6398594359906));
#51631=CARTESIAN_POINT('Ctrl Pts',(-4.91313886229116,0.00364073211770066,
70.2351405640091));
#51632=CARTESIAN_POINT('Ctrl Pts',(-4.90579538722953,-1.07104410681227,
70.2958588158442));
#51633=CARTESIAN_POINT('Ctrl Pts',(-4.02922553257357,-3.79928397318142,
70.4493850188949));
#51634=CARTESIAN_POINT('Ctrl Pts',(0.481468380347833,-5.79723319357744,
70.6957191731614));
#51635=CARTESIAN_POINT('Ctrl Pts',(5.13738901395058,-2.72891161845354,70.9741430268085));
#51636=CARTESIAN_POINT('Ctrl Pts',(5.07303785361562,2.84675454470068,71.2525668804556));
#51637=CARTESIAN_POINT('Ctrl Pts',(0.347541231067252,5.80680114991893,71.5309907341027));
#51638=CARTESIAN_POINT('Ctrl Pts',(-4.07701077938671,3.72355998975012,71.7751819619539));
#51639=CARTESIAN_POINT('Ctrl Pts',(-4.90611848687863,1.03396024638341,71.9265652385894));
#51640=CARTESIAN_POINT('Ctrl Pts',(-4.91232903289984,-0.00322496870272818,
71.9851405640091));
#51641=CARTESIAN_POINT('Origin',(0.,0.,-13.2351405640096));
#51642=CARTESIAN_POINT('',(-4.91528466670162,-0.00430068889825521,68.1398594359906));
#51643=CARTESIAN_POINT('',(-4.92558708781353,0.00179722223583485,68.4851405640091));
#51644=CARTESIAN_POINT('',(-4.91825,6.88216836313478E-12,-13.2351405640096));
#51645=CARTESIAN_POINT('Ctrl Pts',(-4.91528466670162,-0.00430068889825559,
68.1398594359906));
#51646=CARTESIAN_POINT('Ctrl Pts',(-4.91930521123973,-0.487007885028925,
68.1671617840622));
#51647=CARTESIAN_POINT('Ctrl Pts',(-4.63198207672563,-2.60556107402994,
68.2872538907107));
#51648=CARTESIAN_POINT('Ctrl Pts',(-1.59220212159397,-5.59465176912459,
68.5001357559359));
#51649=CARTESIAN_POINT('Ctrl Pts',(3.84508720656895,-4.36469247343464,68.7785050316661));
#51650=CARTESIAN_POINT('Ctrl Pts',(5.75074907247032,0.874140217161407,69.0568743073964));
#51651=CARTESIAN_POINT('Ctrl Pts',(2.37447524697441,5.31009447329176,69.3352435831267));
#51652=CARTESIAN_POINT('Ctrl Pts',(-3.16857614270845,4.86996611098083,69.6129052926581));
#51653=CARTESIAN_POINT('Ctrl Pts',(-4.92524043635853,1.61832750604788,69.7977772436127));
#51654=CARTESIAN_POINT('Ctrl Pts',(-4.92635784080807,-0.000234171170717511,
69.8898594359906));
#51655=CARTESIAN_POINT('Ctrl Pts',(-4.92558708781353,0.00179722223583461,
68.4851405640091));
#51656=CARTESIAN_POINT('Ctrl Pts',(-4.91839816763849,-1.53165810334221,
68.5723444418832));
#51657=CARTESIAN_POINT('Ctrl Pts',(-3.32299121478259,-4.71001393647895,
68.7523562709731));
#51658=CARTESIAN_POINT('Ctrl Pts',(2.09350891225194,-5.42742525847318,69.0251760512785));
#51659=CARTESIAN_POINT('Ctrl Pts',(5.69773921438019,-1.17281385859187,69.3035999049257));
#51660=CARTESIAN_POINT('Ctrl Pts',(4.06684372988438,4.15938776488691,69.5820237585728));
#51661=CARTESIAN_POINT('Ctrl Pts',(-1.30069846296805,5.66991252229023,69.8604476122199));
#51662=CARTESIAN_POINT('Ctrl Pts',(-4.56322738594952,2.77755851836255,70.0781532140321));
#51663=CARTESIAN_POINT('Ctrl Pts',(-4.91701990135298,0.571613497603942,
70.2030508646285));
#51664=CARTESIAN_POINT('Ctrl Pts',(-4.91313886229116,0.00364073211770066,
70.2351405640091));
#51665=CARTESIAN_POINT('Origin',(0.,0.,-13.2351405640096));
#51666=CARTESIAN_POINT('',(-4.91097073342421,0.00211795400143013,66.3898594359906));
#51667=CARTESIAN_POINT('',(-4.91863147951157,-0.0045239198518876,66.7351405640092));
#51668=CARTESIAN_POINT('',(-4.91825,6.88216836313478E-12,-13.2351405640096));
#51669=CARTESIAN_POINT('Ctrl Pts',(-4.91097073342421,0.00211795400142982,
66.3898594359906));
#51670=CARTESIAN_POINT('Ctrl Pts',(-4.90727785389205,-0.952892345756783,
66.443756565935));
#51671=CARTESIAN_POINT('Ctrl Pts',(-4.17680693104425,-3.55727669197261,
66.5904434544562));
#51672=CARTESIAN_POINT('Ctrl Pts',(0.0534777550381669,-5.8165605080231,
66.8299201015543));
#51673=CARTESIAN_POINT('Ctrl Pts',(4.92167117725461,-3.10038527231038,67.1082893772844));
#51674=CARTESIAN_POINT('Ctrl Pts',(5.26941859759108,2.46342518805391,67.3866586530149));
#51675=CARTESIAN_POINT('Ctrl Pts',(0.777321710206332,5.76463415774316,67.665027928745));
#51676=CARTESIAN_POINT('Ctrl Pts',(-3.91812067181916,3.9666740065567,67.9160948564037));
#51677=CARTESIAN_POINT('Ctrl Pts',(-4.90564098880511,1.15352076381265,68.0743720254855));
#51678=CARTESIAN_POINT('Ctrl Pts',(-4.91528466670162,-0.00430068889825559,
68.1398594359906));
#51679=CARTESIAN_POINT('Ctrl Pts',(-4.91863147951157,-0.00452391985188844,
66.7351405640092));
#51680=CARTESIAN_POINT('Ctrl Pts',(-4.92205279654655,-0.373072104444159,
66.7560221167066));
#51681=CARTESIAN_POINT('Ctrl Pts',(-4.71571170713008,-2.37583601988883,
66.8697116206198));
#51682=CARTESIAN_POINT('Ctrl Pts',(-1.97406961996107,-5.47199905313755,
67.0762090757487));
#51683=CARTESIAN_POINT('Ctrl Pts',(3.53632074680071,-4.61889165035702,67.3546329293958));
#51684=CARTESIAN_POINT('Ctrl Pts',(5.79751292551162,0.478088255991047,67.633056783043));
#51685=CARTESIAN_POINT('Ctrl Pts',(2.73190647889548,5.13579706497058,67.91148063669));
#51686=CARTESIAN_POINT('Ctrl Pts',(-2.843796256125,5.07469677474826,68.1899044903372));
#51687=CARTESIAN_POINT('Ctrl Pts',(-4.87863192338278,1.83043745707829,68.3811244661102));
#51688=CARTESIAN_POINT('Ctrl Pts',(-4.9260490768545,0.100343253904555,68.4795364906675));
#51689=CARTESIAN_POINT('Ctrl Pts',(-4.92558708781353,0.00179722223583461,
68.4851405640091));
#51690=CARTESIAN_POINT('Origin',(0.,0.,-13.2351405640096));
#51691=CARTESIAN_POINT('',(-4.92306599949043,0.00350342792735477,64.6398594359906));
#51692=CARTESIAN_POINT('',(-4.91010877574632,0.000282588420590091,64.9851405640092));
#51693=CARTESIAN_POINT('',(-4.91825,6.88216836313478E-12,-13.2351405640096));
#51694=CARTESIAN_POINT('Ctrl Pts',(-4.92306599949043,0.00350342792735464,
64.6398594359906));
#51695=CARTESIAN_POINT('Ctrl Pts',(-4.91164684544424,-1.41383247848128,
64.7203513478078));
#51696=CARTESIAN_POINT('Ctrl Pts',(-3.52301758553069,-4.48456406519882,
64.8936330182019));
#51697=CARTESIAN_POINT('Ctrl Pts',(1.69479929893489,-5.56443090981521,65.1597044471726));
#51698=CARTESIAN_POINT('Ctrl Pts',(5.59714854594884,-1.58340271831267,65.4380737229028));
#51699=CARTESIAN_POINT('Ctrl Pts',(4.3586407841906,3.85194581064795,65.7164429986333));
#51700=CARTESIAN_POINT('Ctrl Pts',(-0.883182029898331,5.74936740136187,
65.9948122743633));
#51701=CARTESIAN_POINT('Ctrl Pts',(-4.45597285748787,3.02117738192304,66.2192844201493));
#51702=CARTESIAN_POINT('Ctrl Pts',(-4.91363554678953,0.691261531159927,
66.3509668073583));
#51703=CARTESIAN_POINT('Ctrl Pts',(-4.91097073342421,0.00211795400142982,
66.3898594359906));
#51704=CARTESIAN_POINT('Ctrl Pts',(-4.91010877574632,0.00028258842059023,
64.9851405640092));
#51705=CARTESIAN_POINT('Ctrl Pts',(-4.90968013456912,-0.839389986717853,
65.0325077427457));
#51706=CARTESIAN_POINT('Ctrl Pts',(-4.30568284721683,-3.32483686443376,
65.172682872698));
#51707=CARTESIAN_POINT('Ctrl Pts',(-0.354312235753313,-5.80639193833713,
65.4056659538659));
#51708=CARTESIAN_POINT('Ctrl Pts',(4.69327425521161,-3.4369901465322,65.684089807513));
#51709=CARTESIAN_POINT('Ctrl Pts',(5.42864494396021,2.09034412822534,65.9625136611601));
#51710=CARTESIAN_POINT('Ctrl Pts',(1.1761356923939,5.69705444375144,66.2409375148073));
#51711=CARTESIAN_POINT('Ctrl Pts',(-3.75703406542712,4.19135073581093,66.498479815757));
#51712=CARTESIAN_POINT('Ctrl Pts',(-4.90684677096616,1.26493836497993,66.6632141654909));
#51713=CARTESIAN_POINT('Ctrl Pts',(-4.91863147951157,-0.00452391985188844,
66.7351405640092));
#51714=CARTESIAN_POINT('Origin',(0.,0.,-13.2351405640096));
#51715=CARTESIAN_POINT('',(-4.92210345011766,-0.00387026642323893,62.8898594359906));
#51716=CARTESIAN_POINT('',(-4.91967215389204,0.00442564071372511,63.2351405640092));
#51717=CARTESIAN_POINT('',(-4.91825,6.88216836313478E-12,-13.2351405640096));
#51718=CARTESIAN_POINT('Ctrl Pts',(-4.92210345011766,-0.00387026642323842,
62.8898594359906));
#51719=CARTESIAN_POINT('Ctrl Pts',(-4.92427744727768,-0.255745006656511,
62.9041563711039));
#51720=CARTESIAN_POINT('Ctrl Pts',(-4.79202192949461,-2.14004400017903,
63.011243064794));
#51721=CARTESIAN_POINT('Ctrl Pts',(-2.35776357238246,-5.31753579682578,
63.2111195170607));
#51722=CARTESIAN_POINT('Ctrl Pts',(3.19799800541104,-4.85881104501553,63.489488792791));
#51723=CARTESIAN_POINT('Ctrl Pts',(5.81646922451705,0.0626240690466223,
63.7678580685212));
#51724=CARTESIAN_POINT('Ctrl Pts',(3.09264224773008,4.92654036229607,64.0462273442516));
#51725=CARTESIAN_POINT('Ctrl Pts',(-2.47170815707546,5.26553841501739,64.3245966199818));
#51726=CARTESIAN_POINT('Ctrl Pts',(-4.8133314322023,2.06866842134372,64.5224739838948));
#51727=CARTESIAN_POINT('Ctrl Pts',(-4.92481065933777,0.220049157681148,
64.6275615892311));
#51728=CARTESIAN_POINT('Ctrl Pts',(-4.92306599949043,0.00350342792735464,
64.6398594359906));
#51729=CARTESIAN_POINT('Ctrl Pts',(-4.91967215389204,0.00442564071372501,
63.2351405640092));
#51730=CARTESIAN_POINT('Ctrl Pts',(-4.90758283094165,-1.29832969996648,
63.3089933687848));
#51731=CARTESIAN_POINT('Ctrl Pts',(-3.70638809642316,-4.25790548455125,
63.4756541247759));
#51732=CARTESIAN_POINT('Ctrl Pts',(1.29408596185757,-5.67142539625746,63.7351228319832));
#51733=CARTESIAN_POINT('Ctrl Pts',(5.47084715344585,-1.97725970110767,64.0135466856302));
#51734=CARTESIAN_POINT('Ctrl Pts',(4.62095269617623,3.53362712827672,64.2919705392774));
#51735=CARTESIAN_POINT('Ctrl Pts',(-0.474707969112876,5.79779068663673,
64.5703943929245));
#51736=CARTESIAN_POINT('Ctrl Pts',(-4.34150134912124,3.25597814609928,64.8014510678351));
#51737=CARTESIAN_POINT('Ctrl Pts',(-4.91051998423979,0.805805979545269,
64.93969979153));
#51738=CARTESIAN_POINT('Ctrl Pts',(-4.91010877574632,0.00028258842059023,
64.9851405640092));
#51739=CARTESIAN_POINT('Origin',(0.,0.,-13.2351405640096));
#51740=CARTESIAN_POINT('',(-4.91057232344976,-0.0015814614971166,61.1398594359906));
#51741=CARTESIAN_POINT('',(-4.92500427991532,-0.00235440163140754,61.4851405640091));
#51742=CARTESIAN_POINT('',(-4.91825,6.88216836313478E-12,-13.2351405640096));
#51743=CARTESIAN_POINT('Ctrl Pts',(-4.91057232344976,-0.00158146149711672,
61.1398594359906));
#51744=CARTESIAN_POINT('Ctrl Pts',(-4.91265475868819,-0.726293947282865,
61.1807511529767));
#51745=CARTESIAN_POINT('Ctrl Pts',(-4.4222253859021,-3.09281216434233,61.3144326285396));
#51746=CARTESIAN_POINT('Ctrl Pts',(-0.75918843374404,-5.76705028032932,
61.5409038626791));
#51747=CARTESIAN_POINT('Ctrl Pts',(4.4405661116445,-3.75720755640298,61.8192731384095));
#51748=CARTESIAN_POINT('Ctrl Pts',(5.56175900540656,1.703547116917,62.0976424141395));
#51749=CARTESIAN_POINT('Ctrl Pts',(1.57459939979797,5.59963148286865,62.3760116898701));
#51750=CARTESIAN_POINT('Ctrl Pts',(-3.57973792379162,4.41662647127613,62.6400840304868));
#51751=CARTESIAN_POINT('Ctrl Pts',(-4.9101678027961,1.37896873811473,62.8113666125271));
#51752=CARTESIAN_POINT('Ctrl Pts',(-4.92210345011766,-0.00387026642323842,
62.8898594359906));
#51753=CARTESIAN_POINT('Ctrl Pts',(-4.92500427991532,-0.00235440163140841,
61.4851405640091));
#51754=CARTESIAN_POINT('Ctrl Pts',(-4.92578548668796,-0.134817287697758,
61.4926710436081));
#51755=CARTESIAN_POINT('Ctrl Pts',(-4.86077673604698,-1.89901484929061,
61.5930094744228));
#51756=CARTESIAN_POINT('Ctrl Pts',(-2.73789341270518,-5.13260792995689,
61.7861558564532));
#51757=CARTESIAN_POINT('Ctrl Pts',(2.83787677981535,-5.07800944116647,62.0645797101003));
#51758=CARTESIAN_POINT('Ctrl Pts',(5.80618437177022,-0.357697558004235,
62.3430035637474));
#51759=CARTESIAN_POINT('Ctrl Pts',(3.4397259481389,4.69126954072045,62.6214274173947));
#51760=CARTESIAN_POINT('Ctrl Pts',(-2.08717863360625,5.42986278403133,62.8998512710416));
#51761=CARTESIAN_POINT('Ctrl Pts',(-4.73901895071827,2.30689062440745,63.1044223199133));
#51762=CARTESIAN_POINT('Ctrl Pts',(-4.92277501352727,0.338792335834338,
63.2161854175691));
#51763=CARTESIAN_POINT('Ctrl Pts',(-4.91967215389204,0.00442564071372501,
63.2351405640092));
#51764=CARTESIAN_POINT('Origin',(0.,0.,-13.2351405640096));
#51765=CARTESIAN_POINT('',(-4.91628642972681,0.00445635614462418,59.3898594359906));
#51766=CARTESIAN_POINT('',(-4.91240599187292,-0.00326991338738425,59.7351405640091));
#51767=CARTESIAN_POINT('',(-4.91825,6.88216836313478E-12,-13.2351405640096));
#51768=CARTESIAN_POINT('Ctrl Pts',(-4.91628642972681,0.00445635614462425,
59.3898594359906));
#51769=CARTESIAN_POINT('Ctrl Pts',(-4.9058282512334,-1.18809301663682,59.4573459348495));
#51770=CARTESIAN_POINT('Ctrl Pts',(-3.86949289148344,-4.03660726229823,
59.6176221922852));
#51771=CARTESIAN_POINT('Ctrl Pts',(0.901259081565336,-5.74656141372159,
59.8706882082974));
#51772=CARTESIAN_POINT('Ctrl Pts',(5.32123674041329,-2.34939897979313,60.1490574840279));
#51773=CARTESIAN_POINT('Ctrl Pts',(4.85377627470227,3.20563439726283,60.4274267597579));
#51774=CARTESIAN_POINT('Ctrl Pts',(-0.0717702282064447,5.81636355879867,
60.7057960354884));
#51775=CARTESIAN_POINT('Ctrl Pts',(-4.21753087644577,3.4861376510141,60.9432735942325));
#51776=CARTESIAN_POINT('Ctrl Pts',(-4.90792938452277,0.918193042991883,
61.0879613943999));
#51777=CARTESIAN_POINT('Ctrl Pts',(-4.91057232344976,-0.00158146149711672,
61.1398594359906));
#51778=CARTESIAN_POINT('Ctrl Pts',(-4.91240599187292,-0.00326991338738404,
59.7351405640092));
#51779=CARTESIAN_POINT('Ctrl Pts',(-4.91606640436456,-0.605564742131566,
59.7691566696472));
#51780=CARTESIAN_POINT('Ctrl Pts',(-4.53400968494839,-2.84665020624194,
59.8959807265009));
#51781=CARTESIAN_POINT('Ctrl Pts',(-1.18277815942064,-5.69567909274991,
60.1156127345705));
#51782=CARTESIAN_POINT('Ctrl Pts',(4.15226795782324,-4.07411282470503,60.3940365882174));
#51783=CARTESIAN_POINT('Ctrl Pts',(5.67217894144929,1.29077905087206,60.6724604418648));
#51784=CARTESIAN_POINT('Ctrl Pts',(1.98044911010386,5.469693393992,60.9508842955118));
#51785=CARTESIAN_POINT('Ctrl Pts',(-3.38186697238311,4.64591220500507,61.22177766956));
#51786=CARTESIAN_POINT('Ctrl Pts',(-4.91615765368059,1.4976961407447,61.3998630923924));
#51787=CARTESIAN_POINT('Ctrl Pts',(-4.92500427991532,-0.00235440163140841,
61.4851405640091));
#51788=CARTESIAN_POINT('Origin',(0.,0.,-13.2351405640096));
#51789=CARTESIAN_POINT('',(-4.9263260156827,-0.000426885928948556,57.6398594359905));
#51790=CARTESIAN_POINT('',(-4.91305232001281,0.00360176434312187,57.9851405640092));
#51791=CARTESIAN_POINT('',(-4.91825,6.88216836313478E-12,-13.2351405640096));
#51792=CARTESIAN_POINT('Ctrl Pts',(-4.9263260156827,-0.000426885928949852,
57.6398594359905));
#51793=CARTESIAN_POINT('Ctrl Pts',(-4.92635412757088,-0.0231288288560638,
57.6411509581455));
#51794=CARTESIAN_POINT('Ctrl Pts',(-4.9159151427125,-1.67683142689444,57.7352322388772));
#51795=CARTESIAN_POINT('Ctrl Pts',(-3.0771332764778,-4.93624217523513,57.9221032781857));
#51796=CARTESIAN_POINT('Ctrl Pts',(2.4882557394928,-5.25773899967072,58.2004725539159));
#51797=CARTESIAN_POINT('Ctrl Pts',(5.76823695308387,-0.750118968468039,
58.4788418296462));
#51798=CARTESIAN_POINT('Ctrl Pts',(3.7502202441463,4.44646872632352,58.7572111053764));
#51799=CARTESIAN_POINT('Ctrl Pts',(-1.7122907225886,5.55907334859995,59.0355803811067));
#51800=CARTESIAN_POINT('Ctrl Pts',(-4.65907391466842,2.53390393001092,59.2464631579781));
#51801=CARTESIAN_POINT('Ctrl Pts',(-4.9202075993099,0.451588553192956,59.3645561762727));
#51802=CARTESIAN_POINT('Ctrl Pts',(-4.91628642972681,0.00445635614462425,
59.3898594359906));
#51803=CARTESIAN_POINT('Ctrl Pts',(-4.91305232001281,0.00360176434312139,
57.9851405640092));
#51804=CARTESIAN_POINT('Ctrl Pts',(-4.90582152856365,-1.06729817837134,
58.0456422956863));
#51805=CARTESIAN_POINT('Ctrl Pts',(-4.0341145126111,-3.79164216223504,58.1989519785791));
#51806=CARTESIAN_POINT('Ctrl Pts',(0.467946912388112,-5.79834029608278,
58.4450696126877));
#51807=CARTESIAN_POINT('Ctrl Pts',(5.13101074500744,-2.7408854840378,58.7234934663347));
#51808=CARTESIAN_POINT('Ctrl Pts',(5.07966318532585,2.83491559409379,59.001917319982));
#51809=CARTESIAN_POINT('Ctrl Pts',(0.361082758659297,5.80597483144648,59.2803411736289));
#51810=CARTESIAN_POINT('Ctrl Pts',(-4.07224317210069,3.73122014391495,59.5247489216382));
#51811=CARTESIAN_POINT('Ctrl Pts',(-4.90607950617085,1.03770829089449,59.6763487184315));
#51812=CARTESIAN_POINT('Ctrl Pts',(-4.91240599187292,-0.00326991338738404,
59.7351405640092));
#51813=CARTESIAN_POINT('Origin',(0.,0.,-13.2351405640096));
#51814=CARTESIAN_POINT('',(-4.91500211464461,-0.00424101522293115,55.8898594359906));
#51815=CARTESIAN_POINT('',(-4.92552843553515,0.00186197695103037,56.2351405640092));
#51816=CARTESIAN_POINT('',(-4.91825,6.88216836313478E-12,-13.2351405640096));
#51817=CARTESIAN_POINT('Ctrl Pts',(-4.91500211464461,-0.00424101522293059,
55.8898594359906));
#51818=CARTESIAN_POINT('Ctrl Pts',(-4.91903479884973,-0.497344277840858,
55.9177457400183));
#51819=CARTESIAN_POINT('Ctrl Pts',(-4.62389168535497,-2.62649724502737,
56.0384218026228));
#51820=CARTESIAN_POINT('Ctrl Pts',(-1.55698110414879,-5.60455581247088,
56.2518876238041));
#51821=CARTESIAN_POINT('Ctrl Pts',(3.87246440760804,-4.34042111154972,56.5302568995343));
#51822=CARTESIAN_POINT('Ctrl Pts',(5.74513710412806,0.910294275796876,56.8086261752646));
#51823=CARTESIAN_POINT('Ctrl Pts',(2.34102857791428,5.3249245263352,57.0869954509948));
#51824=CARTESIAN_POINT('Ctrl Pts',(-3.18749317080709,4.85093885713963,57.3640732045702));
#51825=CARTESIAN_POINT('Ctrl Pts',(-4.92433442136023,1.60789840159787,57.5483611995687));
#51826=CARTESIAN_POINT('Ctrl Pts',(-4.9263260156827,-0.000426885928949852,
57.6398594359905));
#51827=CARTESIAN_POINT('Ctrl Pts',(-4.92552843553515,0.00186197695103052,
56.2351405640092));
#51828=CARTESIAN_POINT('Ctrl Pts',(-4.9181339110517,-1.52783432001219,56.3221279217254));
#51829=CARTESIAN_POINT('Ctrl Pts',(-3.32966935051829,-4.70283072137663,
56.5019232306572));
#51830=CARTESIAN_POINT('Ctrl Pts',(2.08084551689526,-5.43229292627044,56.7745264908049));
#51831=CARTESIAN_POINT('Ctrl Pts',(5.69498851284468,-1.18609879038724,57.052950344452));
#51832=CARTESIAN_POINT('Ctrl Pts',(4.07653308749828,4.14989186467828,57.3313741980992));
#51833=CARTESIAN_POINT('Ctrl Pts',(-1.2874717010986,5.67293055843817,57.6097980517462));
#51834=CARTESIAN_POINT('Ctrl Pts',(-4.55998868921863,2.78532417715685,57.8277201737163));
#51835=CARTESIAN_POINT('Ctrl Pts',(-4.91691335885449,0.57543215157618,57.9528343444706));
#51836=CARTESIAN_POINT('Ctrl Pts',(-4.91305232001281,0.00360176434312139,
57.9851405640092));
#51837=CARTESIAN_POINT('Origin',(0.,0.,-13.2351405640096));
#51838=CARTESIAN_POINT('',(-4.91110894597329,0.00226854779708756,54.1398594359906));
#51839=CARTESIAN_POINT('',(-4.91874848582105,-0.00451671112762952,54.4851405640092));
#51840=CARTESIAN_POINT('',(-4.91825,6.88216836313478E-12,-13.2351405640096));
#51841=CARTESIAN_POINT('Ctrl Pts',(-4.91110894597329,0.00226854779708741,
54.1398594359906));
#51842=CARTESIAN_POINT('Ctrl Pts',(-4.9071041400712,-0.963021056215211,
54.1943405218911));
#51843=CARTESIAN_POINT('Ctrl Pts',(-4.16469942930719,-3.57803361618035,
54.3416113663684));
#51844=CARTESIAN_POINT('Ctrl Pts',(0.0900619915185718,-5.81610908180557,
54.5816719694224));
#51845=CARTESIAN_POINT('Ctrl Pts',(4.94107477914329,-3.06936736815449,54.8600412451526));
#51846=CARTESIAN_POINT('Ctrl Pts',(5.25381978618318,2.49652031197179,55.138410520883));
#51847=CARTESIAN_POINT('Ctrl Pts',(0.741047648394848,5.76940936288854,55.4167797966132));
#51848=CARTESIAN_POINT('Ctrl Pts',(-3.93209835299061,3.94620162905268,55.6672627683158));
#51849=CARTESIAN_POINT('Ctrl Pts',(-4.90561631953321,1.14342291189664,55.8249559814415));
#51850=CARTESIAN_POINT('Ctrl Pts',(-4.91500211464461,-0.00424101522293059,
55.8898594359906));
#51851=CARTESIAN_POINT('Ctrl Pts',(-4.91874848582105,-0.00451671112763018,
54.4851405640092));
#51852=CARTESIAN_POINT('Ctrl Pts',(-4.92213659647667,-0.36922122126081,
54.5058055965487));
#51853=CARTESIAN_POINT('Ctrl Pts',(-4.7183726132553,-2.36808483286878,54.619278580304));
#51854=CARTESIAN_POINT('Ctrl Pts',(-1.98682590730801,-5.46738029736734,
54.8255595152749));
#51855=CARTESIAN_POINT('Ctrl Pts',(3.52553906903275,-4.627126405742,55.1039833689222));
#51856=CARTESIAN_POINT('Ctrl Pts',(5.7986121442169,0.464566144840059,55.3824072225692));
#51857=CARTESIAN_POINT('Ctrl Pts',(2.74387662363257,5.12941181581999,55.6608310762164));
#51858=CARTESIAN_POINT('Ctrl Pts',(-2.83195344466994,5.08131520270228,55.9392549298634));
#51859=CARTESIAN_POINT('Ctrl Pts',(-4.87666238088383,1.83814217788545,56.1306914257944));
#51860=CARTESIAN_POINT('Ctrl Pts',(-4.92602322606875,0.104218693560284,
56.2293199705097));
#51861=CARTESIAN_POINT('Ctrl Pts',(-4.92552843553515,0.00186197695103052,
56.2351405640092));
#51862=CARTESIAN_POINT('Origin',(0.,0.,-13.2351405640096));
#51863=CARTESIAN_POINT('',(-4.92333307335781,0.0033824739169612,52.3898594359906));
#51864=CARTESIAN_POINT('',(-4.91010297280824,0.000219119417446956,52.7351405640092));
#51865=CARTESIAN_POINT('',(-4.91825,6.88216836313478E-12,-13.2351405640096));
#51866=CARTESIAN_POINT('Ctrl Pts',(-4.92333307335781,0.00338247391696123,
52.3898594359906));
#51867=CARTESIAN_POINT('Ctrl Pts',(-4.9121235422079,-1.4240336674598,52.4709353037639));
#51868=CARTESIAN_POINT('Ctrl Pts',(-3.50620705899313,-4.50433666380612,
52.6448009301139));
#51869=CARTESIAN_POINT('Ctrl Pts',(1.72976521052916,-5.55366080439025,52.9114563150408));
#51870=CARTESIAN_POINT('Ctrl Pts',(5.6069971929771,-1.54816617057876,53.1898255907711));
#51871=CARTESIAN_POINT('Ctrl Pts',(4.33432640242356,3.87928481179605,53.4681948665013));
#51872=CARTESIAN_POINT('Ctrl Pts',(-0.919327219170563,5.74369858870307,
53.7465641422317));
#51873=CARTESIAN_POINT('Ctrl Pts',(-4.4656378077124,3.0002458228677,53.9704523320613));
#51874=CARTESIAN_POINT('Ctrl Pts',(-4.91392494708448,0.68101719729,54.1015507633143));
#51875=CARTESIAN_POINT('Ctrl Pts',(-4.91110894597329,0.00226854779708741,
54.1398594359906));
#51876=CARTESIAN_POINT('Ctrl Pts',(-4.91010297280824,0.000219119417446609,
52.7351405640092));
#51877=CARTESIAN_POINT('Ctrl Pts',(-4.90977214474024,-0.835617689631801,
52.7822912225878));
#51878=CARTESIAN_POINT('Ctrl Pts',(-4.30975846453187,-3.3171009819724,52.9222498323822));
#51879=CARTESIAN_POINT('Ctrl Pts',(-0.367852790578618,-5.80554982981413,
53.1550163933922));
#51880=CARTESIAN_POINT('Ctrl Pts',(4.68524583146246,-3.4479263334292,53.4334402470393));
#51881=CARTESIAN_POINT('Ctrl Pts',(5.43350522761236,2.0776778969562,53.7118641006865));
#51882=CARTESIAN_POINT('Ctrl Pts',(1.18941901815086,5.69429599698262,53.9902879543335));
#51883=CARTESIAN_POINT('Ctrl Pts',(-3.75139922738628,4.19884520123217,54.2480467754412));
#51884=CARTESIAN_POINT('Ctrl Pts',(-4.90692038000867,1.26868950158949,54.412997645333));
#51885=CARTESIAN_POINT('Ctrl Pts',(-4.91874848582105,-0.00451671112763018,
54.4851405640092));
#51886=CARTESIAN_POINT('Origin',(0.,0.,-13.2351405640096));
#51887=CARTESIAN_POINT('',(-4.92181031186921,-0.00396311810717911,50.6398594359906));
#51888=CARTESIAN_POINT('',(-4.91955543626503,0.00444052391018634,50.9851405640092));
#51889=CARTESIAN_POINT('',(-4.91825,6.88216836313478E-12,-13.2351405640096));
#51890=CARTESIAN_POINT('Ctrl Pts',(-4.92181031186921,-0.00396311810717906,
50.6398594359906));
#51891=CARTESIAN_POINT('Ctrl Pts',(-4.92410826691375,-0.266166171072131,
50.6547403270599));
#51892=CARTESIAN_POINT('Ctrl Pts',(-4.78563672242207,-2.16090437287408,
50.762410976706));
#51893=CARTESIAN_POINT('Ctrl Pts',(-2.32427042909063,-5.33226058874023,
50.962871384929));
#51894=CARTESIAN_POINT('Ctrl Pts',(3.22849593851986,-4.8386000029697,51.2412406606591));
#51895=CARTESIAN_POINT('Ctrl Pts',(5.81596027116012,0.0992075504414687,
51.5196099363895));
#51896=CARTESIAN_POINT('Ctrl Pts',(3.06159387029672,4.94589516540121,51.7979792121197));
#51897=CARTESIAN_POINT('Ctrl Pts',(-2.50477871137838,5.24988758173003,52.07634848785));
#51898=CARTESIAN_POINT('Ctrl Pts',(-4.81939694442464,2.04782992932728,52.273641895807));
#51899=CARTESIAN_POINT('Ctrl Pts',(-4.9249526332522,0.209616428241301,52.3781455451872));
#51900=CARTESIAN_POINT('Ctrl Pts',(-4.92333307335781,0.00338247391696123,
52.3898594359906));
#51901=CARTESIAN_POINT('Ctrl Pts',(-4.91955543626503,0.00444052391018648,
50.9851405640092));
#51902=CARTESIAN_POINT('Ctrl Pts',(-4.90749085177966,-1.29457459993488,
51.0587768486269));
#51903=CARTESIAN_POINT('Ctrl Pts',(-3.71213818630798,-4.25043923730225,
51.2252210844603));
#51904=CARTESIAN_POINT('Ctrl Pts',(1.28085568968505,-5.67442800678559,51.4844732715094));
#51905=CARTESIAN_POINT('Ctrl Pts',(5.4662209609829,-1.99001329334819,51.7628971251566));
#51906=CARTESIAN_POINT('Ctrl Pts',(4.62918116396803,3.52284065111588,52.0413209788037));
#51907=CARTESIAN_POINT('Ctrl Pts',(-0.461185219367196,5.79888202116823,
52.3197448324508));
#51908=CARTESIAN_POINT('Ctrl Pts',(-4.33752509971949,3.26372098771621,52.5510180275193));
#51909=CARTESIAN_POINT('Ctrl Pts',(-4.91042332281752,0.809583122763727,
52.6894832713721));
#51910=CARTESIAN_POINT('Ctrl Pts',(-4.91010297280824,0.000219119417446609,
52.7351405640092));
#51911=CARTESIAN_POINT('Origin',(0.,0.,-13.2351405640096));
#51912=CARTESIAN_POINT('',(-4.91047827356641,-0.00141950771611534,48.8898594359906));
#51913=CARTESIAN_POINT('',(-4.92507636652171,-0.00229403587955257,49.2351405640092));
#51914=CARTESIAN_POINT('',(-4.91825,6.88216836313478E-12,-13.2351405640096));
#51915=CARTESIAN_POINT('Ctrl Pts',(-4.91047827356641,-0.00141950771611582,
48.8898594359906));
#51916=CARTESIAN_POINT('Ctrl Pts',(-4.91237210306681,-0.736516413527698,
48.9313351089327));
#51917=CARTESIAN_POINT('Ctrl Pts',(-4.41217290705613,-3.11373014312353,
49.0656005404517));
#51918=CARTESIAN_POINT('Ctrl Pts',(-0.722899533583313,-5.77171138208786,
49.2926557305472));
#51919=CARTESIAN_POINT('Ctrl Pts',(4.46411054420093,-3.72920273824468,49.5710250062776));
#51920=CARTESIAN_POINT('Ctrl Pts',(5.55093393037054,1.73849604958962,49.8493942820078));
#51921=CARTESIAN_POINT('Ctrl Pts',(1.53934740890388,5.60942470922629,50.1277635577381));
#51922=CARTESIAN_POINT('Ctrl Pts',(-3.59606567504477,4.39671076577627,50.391251942399));
#51923=CARTESIAN_POINT('Ctrl Pts',(-4.90977937405317,1.36880030165654,50.5619505684832));
#51924=CARTESIAN_POINT('Ctrl Pts',(-4.92181031186921,-0.00396311810717906,
50.6398594359906));
#51925=CARTESIAN_POINT('Ctrl Pts',(-4.92507636652171,-0.00229403587955276,
49.2351405640092));
#51926=CARTESIAN_POINT('Ctrl Pts',(-4.92581886796819,-0.130943301348753,
49.2424545234503));
#51927=CARTESIAN_POINT('Ctrl Pts',(-4.86282102530499,-1.89130395537016,
49.342576434107));
#51928=CARTESIAN_POINT('Ctrl Pts',(-2.7498561035418,-5.1262087269058,49.5355062959795));
#51929=CARTESIAN_POINT('Ctrl Pts',(2.82602625874287,-5.08461405486067,49.8139301496266));
#51930=CARTESIAN_POINT('Ctrl Pts',(5.80533436864992,-0.371237619541609,
50.0923540032738));
#51931=CARTESIAN_POINT('Ctrl Pts',(3.4506574522521,4.68323474205681,50.3707778569208));
#51932=CARTESIAN_POINT('Ctrl Pts',(-2.07450957073036,5.43471568188616,50.649201710568));
#51933=CARTESIAN_POINT('Ctrl Pts',(-4.73644042858587,2.31463773732241,50.8539892795975));
#51934=CARTESIAN_POINT('Ctrl Pts',(-4.92269652618555,0.342647224444224,
50.9659688974112));
#51935=CARTESIAN_POINT('Ctrl Pts',(-4.91955543626503,0.00444052391018648,
50.9851405640092));
#51936=CARTESIAN_POINT('Origin',(0.,0.,-13.2351405640096));
#51937=CARTESIAN_POINT('',(-4.91658767744717,0.00448723658957973,47.1398594359906));
#51938=CARTESIAN_POINT('',(-4.9124840770588,-0.00331422200313403,47.4851405640092));
#51939=CARTESIAN_POINT('',(-4.91825,6.88216836313478E-12,-13.2351405640096));
#51940=CARTESIAN_POINT('Ctrl Pts',(-4.91658767744717,0.00448723658958032,
47.1398594359906));
#51941=CARTESIAN_POINT('Ctrl Pts',(-4.9059141224208,-1.19819399969518,47.2079298908056));
#51942=CARTESIAN_POINT('Ctrl Pts',(-3.85505991893494,-4.05698950369964,
47.3687901041973));
#51943=CARTESIAN_POINT('Ctrl Pts',(0.937386264007801,-5.74077895462167,
47.6224400761656));
#51944=CARTESIAN_POINT('Ctrl Pts',(5.33590884708369,-2.31588272358329,47.900809351896));
#51945=CARTESIAN_POINT('Ctrl Pts',(4.83351730048996,3.23610051136267,48.1791786276262));
#51946=CARTESIAN_POINT('Ctrl Pts',(-0.108352864056654,5.81579707956082,
48.4575479033566));
#51947=CARTESIAN_POINT('Ctrl Pts',(-4.22921657272871,3.4653350732591,48.6944415061446));
#51948=CARTESIAN_POINT('Ctrl Pts',(-4.90813521021704,0.908049173531873,
48.838545350356));
#51949=CARTESIAN_POINT('Ctrl Pts',(-4.91047827356641,-0.00141950771611582,
48.8898594359906));
#51950=CARTESIAN_POINT('Ctrl Pts',(-4.9124840770588,-0.00331422200313375,
47.4851405640092));
#51951=CARTESIAN_POINT('Ctrl Pts',(-4.91617410517375,-0.601751445209023,
47.5189401494893));
#51952=CARTESIAN_POINT('Ctrl Pts',(-4.53733904880512,-2.83888472337153,
47.6455476861851));
#51953=CARTESIAN_POINT('Ctrl Pts',(-1.19605825955486,-5.69290515833011,
47.8649631740968));
#51954=CARTESIAN_POINT('Ctrl Pts',(4.14275512418048,-4.08378555791893,48.1433870277438));
#51955=CARTESIAN_POINT('Ctrl Pts',(5.67517383763514,1.27754703029398,48.421810881391));
#51956=CARTESIAN_POINT('Ctrl Pts',(1.99320000290249,5.46505976640885,48.7002347350381));
#51957=CARTESIAN_POINT('Ctrl Pts',(-3.37531022387012,4.65313823791433,48.9713446292442));
#51958=CARTESIAN_POINT('Ctrl Pts',(-4.91639715342663,1.50150692616823,49.1496465722345));
#51959=CARTESIAN_POINT('Ctrl Pts',(-4.92507636652171,-0.00229403587955276,
49.2351405640092));
#51960=CARTESIAN_POINT('Origin',(0.,0.,-13.2351405640096));
#51961=CARTESIAN_POINT('',(-4.92627640968079,-0.00061865787654027,45.3898594359906));
#51962=CARTESIAN_POINT('',(-4.91296680399423,0.00356208998599034,45.7351405640092));
#51963=CARTESIAN_POINT('',(-4.91825,6.88216836313478E-12,-13.2351405640096));
#51964=CARTESIAN_POINT('Ctrl Pts',(-4.92627640968079,-0.000618657876541137,
45.3898594359906));
#51965=CARTESIAN_POINT('Ctrl Pts',(-4.92633465053822,-0.033586076024589,
45.3917349141016));
#51966=CARTESIAN_POINT('Ctrl Pts',(-4.91108086732445,-1.69756959127752,
45.4864001507893));
#51967=CARTESIAN_POINT('Ctrl Pts',(-3.046024182882,-4.95549923731964,45.6738551460538));
#51968=CARTESIAN_POINT('Ctrl Pts',(2.52127690930862,-5.24198423885123,45.9522244217841));
#51969=CARTESIAN_POINT('Ctrl Pts',(5.77284098579036,-0.713822783719208,
46.2305936975144));
#51970=CARTESIAN_POINT('Ctrl Pts',(3.72217843764396,4.46996909297098,46.5089629732446));
#51971=CARTESIAN_POINT('Ctrl Pts',(-1.74722258992204,5.54819333071977,46.7873322489749));
#51972=CARTESIAN_POINT('Ctrl Pts',(-4.66681253604691,2.51297709137372,46.9976310698902));
#51973=CARTESIAN_POINT('Ctrl Pts',(-4.92046370339166,0.441232413174631,
47.1151401322288));
#51974=CARTESIAN_POINT('Ctrl Pts',(-4.91658767744717,0.00448723658958032,
47.1398594359906));
#51975=CARTESIAN_POINT('Ctrl Pts',(-4.91296680399423,0.00356208998598999,
45.7351405640092));
#51976=CARTESIAN_POINT('Ctrl Pts',(-4.90584917021152,-1.0635520480926,45.7954257755284));
#51977=CARTESIAN_POINT('Ctrl Pts',(-4.03898978525713,-3.78399820225403,
45.9485189382633));
#51978=CARTESIAN_POINT('Ctrl Pts',(0.454422899244266,-5.79941586115651,
46.1944200522139));
#51979=CARTESIAN_POINT('Ctrl Pts',(5.12460456826788,-2.75284444182363,46.4728439058611));
#51980=CARTESIAN_POINT('Ctrl Pts',(5.08626088852126,2.82306122425459,46.7512677595082));
#51981=CARTESIAN_POINT('Ctrl Pts',(0.374622322305924,5.8051169340179,47.0296916131553));
#51982=CARTESIAN_POINT('Ctrl Pts',(-4.06746198886625,3.7388783229028,47.2743158813224));
#51983=CARTESIAN_POINT('Ctrl Pts',(-4.9060419114083,1.04145606245698,47.4261321982736));
#51984=CARTESIAN_POINT('Ctrl Pts',(-4.9124840770588,-0.00331422200313375,
47.4851405640092));
#51985=CARTESIAN_POINT('Origin',(0.,0.,-13.2351405640096));
#51986=CARTESIAN_POINT('',(-4.91472474733406,-0.00417511919816473,43.6398594359906));
#51987=CARTESIAN_POINT('',(-4.92546797871252,0.00192622575846596,43.9851405640092));
#51988=CARTESIAN_POINT('',(-4.91825,6.88216836313478E-12,-13.2351405640096));
#51989=CARTESIAN_POINT('Ctrl Pts',(-4.91472474733406,-0.00417511919816496,
43.6398594359906));
#51990=CARTESIAN_POINT('Ctrl Pts',(-4.91876162149318,-0.507676058970831,
43.6683296959744));
#51991=CARTESIAN_POINT('Ctrl Pts',(-4.61572084458829,-2.6474350464209,43.789589714535));
#51992=CARTESIAN_POINT('Ctrl Pts',(-1.52169848847216,-5.61423812497824,
44.0036394916721));
#51993=CARTESIAN_POINT('Ctrl Pts',(3.89968840385962,-4.31597803129028,44.2820087674025));
#51994=CARTESIAN_POINT('Ctrl Pts',(5.73929784318452,0.946412320817448,44.5603780431327));
#51995=CARTESIAN_POINT('Ctrl Pts',(2.30748929166079,5.33954391148237,44.838747318863));
#51996=CARTESIAN_POINT('Ctrl Pts',(-3.20629665985511,4.83186626178632,45.1152411164823));
#51997=CARTESIAN_POINT('Ctrl Pts',(-4.92345316924109,1.59748535742421,45.2989451555248));
#51998=CARTESIAN_POINT('Ctrl Pts',(-4.92627640968079,-0.000618657876541137,
45.3898594359906));
#51999=CARTESIAN_POINT('Ctrl Pts',(-4.92546797871252,0.00192622575846612,
43.9851405640092));
#52000=CARTESIAN_POINT('Ctrl Pts',(-4.91787282992045,-1.52401225827842,
44.0719114015675));
#52001=CARTESIAN_POINT('Ctrl Pts',(-3.33633207850513,-4.6956419719452,44.2514901903414));
#52002=CARTESIAN_POINT('Ctrl Pts',(2.06817080372702,-5.43713104758401,44.5238769303312));
#52003=CARTESIAN_POINT('Ctrl Pts',(5.69220683601255,-1.19937727093821,44.8023007839783));
#52004=CARTESIAN_POINT('Ctrl Pts',(4.08620027266672,4.14037339302263,45.0807246376255));
#52005=CARTESIAN_POINT('Ctrl Pts',(-1.27423793661312,5.67591773926357,45.3591484912725));
#52006=CARTESIAN_POINT('Ctrl Pts',(-4.55673857265977,2.7930898524097,45.5772871334005));
#52007=CARTESIAN_POINT('Ctrl Pts',(-4.91680663377896,0.579250131291795,
45.7026178243127));
#52008=CARTESIAN_POINT('Ctrl Pts',(-4.91296680399423,0.00356208998598999,
45.7351405640092));
#52009=CARTESIAN_POINT('Origin',(0.,0.,-13.2351405640096));
#52010=CARTESIAN_POINT('',(-4.91125677312356,0.00241598250425361,41.8898594359907));
#52011=CARTESIAN_POINT('',(-4.91886553528195,-0.00450853108237725,42.2351405640092));
#52012=CARTESIAN_POINT('',(-4.91825,6.88216836313478E-12,-13.2351405640096));
#52013=CARTESIAN_POINT('Ctrl Pts',(-4.91125677312356,0.0024159825042535,
41.8898594359907));
#52014=CARTESIAN_POINT('Ctrl Pts',(-4.90693843454433,-0.973146675809823,
41.9449244778472));
#52015=CARTESIAN_POINT('Ctrl Pts',(-4.15249564758543,-3.59877918216972,
42.0927792782805));
#52016=CARTESIAN_POINT('Ctrl Pts',(0.126642664911688,-5.81542755515032,
42.3334238372905));
#52017=CARTESIAN_POINT('Ctrl Pts',(4.96028289923243,-3.03822803182378,42.6117931130208));
#52018=CARTESIAN_POINT('Ctrl Pts',(5.23801311996793,2.52951666703768,42.8901623887511));
#52019=CARTESIAN_POINT('Ctrl Pts',(0.704744268806608,5.77395631515876,43.1685316644814));
#52020=CARTESIAN_POINT('Ctrl Pts',(-3.94597393987301,3.92571018031166,43.4184306802278));
#52021=CARTESIAN_POINT('Ctrl Pts',(-4.90560471393971,1.13332513565534,43.5755399373976));
#52022=CARTESIAN_POINT('Ctrl Pts',(-4.91472474733406,-0.00417511919816496,
43.6398594359906));
#52023=CARTESIAN_POINT('Ctrl Pts',(-4.91886553528195,-0.00450853108237819,
42.2351405640092));
#52024=CARTESIAN_POINT('Ctrl Pts',(-4.92221974715232,-0.365369816257576,
42.2555890763908));
#52025=CARTESIAN_POINT('Ctrl Pts',(-4.72102302970205,-2.36033413903901,
42.3688455399882));
#52026=CARTESIAN_POINT('Ctrl Pts',(-1.99957138822013,-5.46273180427181,
42.5749099548013));
#52027=CARTESIAN_POINT('Ctrl Pts',(3.51473821570051,-4.6353359939799,42.8533338084484));
#52028=CARTESIAN_POINT('Ctrl Pts',(5.79967982401188,0.45104150689311,43.1317576620956));
#52029=CARTESIAN_POINT('Ctrl Pts',(2.75583184430228,5.12299866756965,43.4101815157427));
#52030=CARTESIAN_POINT('Ctrl Pts',(-2.82009523009366,5.08790599315611,43.6886053693897));
#52031=CARTESIAN_POINT('Ctrl Pts',(-4.87468342339853,1.84584768784173,43.8802583854787));
#52032=CARTESIAN_POINT('Ctrl Pts',(-4.92599641404625,0.108093969687443,
43.9791034503518));
#52033=CARTESIAN_POINT('Ctrl Pts',(-4.92546797871252,0.00192622575846612,
43.9851405640092));
#52034=CARTESIAN_POINT('Origin',(0.,0.,-13.2351405640096));
#52035=CARTESIAN_POINT('',(-4.92359279332473,0.00325554800820353,40.1398594359906));
#52036=CARTESIAN_POINT('',(-4.91009863878307,0.000155608968132326,40.4851405640092));
#52037=CARTESIAN_POINT('',(-4.91825,6.88216836313478E-12,-13.2351405640096));
#52038=CARTESIAN_POINT('Ctrl Pts',(-4.92359279332473,0.0032555480082035,
40.1398594359906));
#52039=CARTESIAN_POINT('Ctrl Pts',(-4.91262089068949,-1.43424326230662,
40.22151925972));
#52040=CARTESIAN_POINT('Ctrl Pts',(-3.489286725208,-4.52407530298379,40.3959688420261));
#52041=CARTESIAN_POINT('Ctrl Pts',(1.76466268810206,-5.5426709816656,40.663208182909));
#52042=CARTESIAN_POINT('Ctrl Pts',(5.61662401257895,-1.5128683733554,40.9415774586392));
#52043=CARTESIAN_POINT('Ctrl Pts',(4.30984054340475,3.90647033832362,41.2199467343696));
#52044=CARTESIAN_POINT('Ctrl Pts',(-0.955436037461097,5.73780254035447,
41.4983160100997));
#52045=CARTESIAN_POINT('Ctrl Pts',(-4.4752161010382,2.97931192419287,41.7216202439735));
#52046=CARTESIAN_POINT('Ctrl Pts',(-4.91421523994953,0.670767874864228,
41.8521347192705));
#52047=CARTESIAN_POINT('Ctrl Pts',(-4.91125677312356,0.0024159825042535,
41.8898594359907));
#52048=CARTESIAN_POINT('Ctrl Pts',(-4.91009863878307,0.000155608968132256,
40.4851405640092));
#52049=CARTESIAN_POINT('Ctrl Pts',(-4.9098647894845,-0.831844790997033,
40.53207470243));
#52050=CARTESIAN_POINT('Ctrl Pts',(-4.31382143773829,-3.30936416075672,
40.6718167920664));
#52051=CARTESIAN_POINT('Ctrl Pts',(-0.381391344636143,-5.80467614464644,
40.9043668329184));
#52052=CARTESIAN_POINT('Ctrl Pts',(4.67719192445218,-3.45884376690104,41.1827906865657));
#52053=CARTESIAN_POINT('Ctrl Pts',(5.43833595818706,2.06500036510422,41.4612145402126));
#52054=CARTESIAN_POINT('Ctrl Pts',(1.20269587460476,5.69150657868371,41.7396383938599));
#52055=CARTESIAN_POINT('Ctrl Pts',(-3.74574984464755,4.20633618758006,41.9976137351253));
#52056=CARTESIAN_POINT('Ctrl Pts',(-4.90699626654784,1.27244108778943,42.1627811251751));
#52057=CARTESIAN_POINT('Ctrl Pts',(-4.91886553528195,-0.00450853108237819,
42.2351405640092));
#52058=CARTESIAN_POINT('Origin',(0.,0.,-13.2351405640096));
#52059=CARTESIAN_POINT('',(-4.92151270901473,-0.00404930601734944,38.3898594359906));
#52060=CARTESIAN_POINT('',(-4.91943860138798,0.00445443611122698,38.7351405640092));
#52061=CARTESIAN_POINT('',(-4.91825,6.88216836313478E-12,-13.2351405640096));
#52062=CARTESIAN_POINT('Ctrl Pts',(-4.92151270901473,-0.00404930601735014,
38.3898594359906));
#52063=CARTESIAN_POINT('Ctrl Pts',(-4.92393319119315,-0.276584443330804,
38.405324283016));
#52064=CARTESIAN_POINT('Ctrl Pts',(-4.77917839932122,-2.18176945279143,
38.5135788886182));
#52065=CARTESIAN_POINT('Ctrl Pts',(-2.29068533160149,-5.3467744225246,38.7146232527971));
#52066=CARTESIAN_POINT('Ctrl Pts',(3.25886614391259,-4.81819753329374,38.9929925285273));
#52067=CARTESIAN_POINT('Ctrl Pts',(5.81522122325282,0.135787106926827,39.2713618042576));
#52068=CARTESIAN_POINT('Ctrl Pts',(3.03042436822842,4.96505429599969,39.5497310799879));
#52069=CARTESIAN_POINT('Ctrl Pts',(-2.53775017010531,5.23402904920365,39.8281003557182));
#52070=CARTESIAN_POINT('Ctrl Pts',(-4.82539101363885,2.02699660194297,40.0248098077191));
#52071=CARTESIAN_POINT('Ctrl Pts',(-4.9250882234629,0.199181370173329,40.1287295011432));
#52072=CARTESIAN_POINT('Ctrl Pts',(-4.92359279332473,0.0032555480082035,
40.1398594359906));
#52073=CARTESIAN_POINT('Ctrl Pts',(-4.91943860138798,0.00445443611122684,
38.7351405640092));
#52074=CARTESIAN_POINT('Ctrl Pts',(-4.90740124733523,-1.29082005479286,
38.808560328469));
#52075=CARTESIAN_POINT('Ctrl Pts',(-3.7178736329033,-4.24296932209831,38.9747880441445));
#52076=CARTESIAN_POINT('Ctrl Pts',(1.26761845088123,-5.6773997538465,39.2338237110357));
#52077=CARTESIAN_POINT('Ctrl Pts',(5.46156503750013,-2.00275606181767,39.5122475646828));
#52078=CARTESIAN_POINT('Ctrl Pts',(4.63738445343698,3.51203501306753,39.79067141833));
#52079=CARTESIAN_POINT('Ctrl Pts',(-0.447659961214595,5.79994181532161,
40.0690952719771));
#52080=CARTESIAN_POINT('Ctrl Pts',(-4.33353632888539,3.27146300503898,40.3005849872035));
#52081=CARTESIAN_POINT('Ctrl Pts',(-4.91032720501026,0.813359640780624,
40.4392667512142));
#52082=CARTESIAN_POINT('Ctrl Pts',(-4.91009863878307,0.000155608968132256,
40.4851405640092));
#52083=CARTESIAN_POINT('Origin',(0.,0.,-13.2351405640096));
#52084=CARTESIAN_POINT('',(-4.91039451300053,-0.00125559194926212,36.6398594359907));
#52085=CARTESIAN_POINT('',(-4.92514685489251,-0.00223306629119513,36.9851405640092));
#52086=CARTESIAN_POINT('',(-4.91825,6.88216836313478E-12,-13.2351405640096));
#52087=CARTESIAN_POINT('Ctrl Pts',(-4.91039451300053,-0.00125559194926225,
36.6398594359907));
#52088=CARTESIAN_POINT('Ctrl Pts',(-4.91209161801324,-0.746734003806369,
36.6819190648888));
#52089=CARTESIAN_POINT('Ctrl Pts',(-4.40203186568558,-3.13464429489364,
36.8167684523638));
#52090=CARTESIAN_POINT('Ctrl Pts',(-0.6865820336325,-5.77614413989737,37.0444075984155));
#52091=CARTESIAN_POINT('Ctrl Pts',(4.48747836490629,-3.70105038310417,37.3227768741457));
#52092=CARTESIAN_POINT('Ctrl Pts',(5.53988924591708,1.77337620282608,37.601146149876));
#52093=CARTESIAN_POINT('Ctrl Pts',(1.50403451741344,5.61899601211875,37.8795154256062));
#52094=CARTESIAN_POINT('Ctrl Pts',(-3.61228496672945,4.376764288983,38.1424198543112));
#52095=CARTESIAN_POINT('Ctrl Pts',(-4.90941019225197,1.35863830109606,38.3125345244393));
#52096=CARTESIAN_POINT('Ctrl Pts',(-4.92151270901473,-0.00404930601735014,
38.3898594359906));
#52097=CARTESIAN_POINT('Ctrl Pts',(-4.92514685489251,-0.00223306629119565,
36.9851405640092));
#52098=CARTESIAN_POINT('Ctrl Pts',(-4.92585130384514,-0.127069110559573,
36.9922380032924));
#52099=CARTESIAN_POINT('Ctrl Pts',(-4.8648557991442,-1.883593835252,37.0921433937912));
#52100=CARTESIAN_POINT('Ctrl Pts',(-2.76180383778841,-5.11978164217659,
37.2848567355058));
#52101=CARTESIAN_POINT('Ctrl Pts',(2.81416036678732,-5.09119101311223,37.5632805891529));
#52102=CARTESIAN_POINT('Ctrl Pts',(5.80445279005691,-0.384775661901064,
37.8417044428));
#52103=CARTESIAN_POINT('Ctrl Pts',(3.46157018808544,4.67517447107051,38.1201282964472));
#52104=CARTESIAN_POINT('Ctrl Pts',(-2.06182922450441,5.4395390200798,38.3985521500943));
#52105=CARTESIAN_POINT('Ctrl Pts',(-4.73385153164491,2.3223853883346,38.6035562392816));
#52106=CARTESIAN_POINT('Ctrl Pts',(-4.92261734310881,0.346501620743559,
38.7157523772533));
#52107=CARTESIAN_POINT('Ctrl Pts',(-4.91943860138798,0.00445443611122684,
38.7351405640092));
#52108=CARTESIAN_POINT('Origin',(0.,0.,-13.2351405640096));
#52109=CARTESIAN_POINT('',(-4.9168921402267,0.00451136639437725,34.8898594359907));
#52110=CARTESIAN_POINT('',(-4.91256327647705,-0.0033578852818672,35.2351405640092));
#52111=CARTESIAN_POINT('',(-4.91825,6.88216836313478E-12,-13.2351405640096));
#52112=CARTESIAN_POINT('Ctrl Pts',(-4.9168921402267,0.00451136639437716,
34.8898594359907));
#52113=CARTESIAN_POINT('Ctrl Pts',(-4.90601460004845,-1.20829635438866,
34.9585138467616));
#52114=CARTESIAN_POINT('Ctrl Pts',(-3.84052319461895,-4.07735003469892,
35.1199580161093));
#52115=CARTESIAN_POINT('Ctrl Pts',(0.973476361005944,-5.73476937534023,
35.3741919440339));
#52116=CARTESIAN_POINT('Ctrl Pts',(5.3503698512895,-2.28227484501538,35.6525612197641));
#52117=CARTESIAN_POINT('Ctrl Pts',(4.81306709973239,3.26643859688978,35.9309304954944));
#52118=CARTESIAN_POINT('Ctrl Pts',(-0.144931213185082,5.81500051222889,
36.2092997712246));
#52119=CARTESIAN_POINT('Ctrl Pts',(-4.24080783721543,3.44452318441275,36.4456094180567));
#52120=CARTESIAN_POINT('Ctrl Pts',(-4.90834755349023,0.897901568891311,
36.5891293063121));
#52121=CARTESIAN_POINT('Ctrl Pts',(-4.91039451300053,-0.00125559194926225,
36.6398594359907));
#52122=CARTESIAN_POINT('Ctrl Pts',(-4.91256327647705,-0.00335788528186755,
35.2351405640092));
#52123=CARTESIAN_POINT('Ctrl Pts',(-4.91628169557517,-0.597937466264363,
35.2687236293315));
#52124=CARTESIAN_POINT('Ctrl Pts',(-4.54065687035625,-2.83111917892638,
35.3951146458694));
#52125=CARTESIAN_POINT('Ctrl Pts',(-1.20933185427489,-5.69010025994507,
35.614313613623));
#52126=CARTESIAN_POINT('Ctrl Pts',(4.13321975790782,-4.09343607924097,35.8927374672701));
#52127=CARTESIAN_POINT('Ctrl Pts',(5.67813786629717,1.26430806108067,36.1711613209173));
#52128=CARTESIAN_POINT('Ctrl Pts',(2.00594005459731,5.46039641412169,36.4495851745644));
#52129=CARTESIAN_POINT('Ctrl Pts',(-3.3687381414251,4.66035896071285,36.7209115889284));
#52130=CARTESIAN_POINT('Ctrl Pts',(-4.91663974719475,1.50531928252447,36.8994300520767));
#52131=CARTESIAN_POINT('Ctrl Pts',(-4.92514685489251,-0.00223306629119565,
36.9851405640092));
#52132=CARTESIAN_POINT('Origin',(0.,0.,-13.2351405640096));
#52133=CARTESIAN_POINT('',(-4.92620963101609,-0.000809084526366828,33.1398594359907));
#52134=CARTESIAN_POINT('',(-4.91288232756503,0.00352171762486198,33.4851405640093));
#52135=CARTESIAN_POINT('',(-4.91825,6.88216836313478E-12,-13.2351405640096));
#52136=CARTESIAN_POINT('Ctrl Pts',(-4.92620963101609,-0.00080908452636648,
33.1398594359907));
#52137=CARTESIAN_POINT('Ctrl Pts',(-4.92630800682412,-0.0440429370985507,
33.1423188700577));
#52138=CARTESIAN_POINT('Ctrl Pts',(-4.90617996860179,-1.7183136832693,33.2375680627015));
#52139=CARTESIAN_POINT('Ctrl Pts',(-3.01479458062872,-4.97456024693533,
33.425607013922));
#52140=CARTESIAN_POINT('Ctrl Pts',(2.55419833083681,-5.22602209146957,33.7039762896522));
#52141=CARTESIAN_POINT('Ctrl Pts',(5.77721662985775,-0.677498358280351,
33.9823455653825));
#52142=CARTESIAN_POINT('Ctrl Pts',(3.69398937205911,4.49329261598795,34.2607148411128));
#52143=CARTESIAN_POINT('Ctrl Pts',(-1.78208533257483,5.53709381184744,34.539084116843));
#52144=CARTESIAN_POINT('Ctrl Pts',(-4.67447254991247,2.4920528176031,34.7487989818024));
#52145=CARTESIAN_POINT('Ctrl Pts',(-4.92071612200041,0.43087197212862,34.8657240881849));
#52146=CARTESIAN_POINT('Ctrl Pts',(-4.9168921402267,0.00451136639437716,
34.8898594359907));
#52147=CARTESIAN_POINT('Ctrl Pts',(-4.91288232756503,0.0035217176248617,
33.4851405640092));
#52148=CARTESIAN_POINT('Ctrl Pts',(-4.90587829766462,-1.059805706633,33.5452092553706));
#52149=CARTESIAN_POINT('Ctrl Pts',(-4.04385136705686,-3.77635211556013,
33.6980858979476));
#52150=CARTESIAN_POINT('Ctrl Pts',(0.440896414474084,-5.80045988294852,
33.9437704917402));
#52151=CARTESIAN_POINT('Ctrl Pts',(5.11817051857534,-2.76478842676563,34.2221943453874));
#52152=CARTESIAN_POINT('Ctrl Pts',(5.09283092731677,2.81119149965931,34.5006181990345));
#52153=CARTESIAN_POINT('Ctrl Pts',(0.388159848365178,5.80422746229918,34.7790420526816));
#52154=CARTESIAN_POINT('Ctrl Pts',(-4.06266721294199,3.74653450500493,35.0238828410066));
#52155=CARTESIAN_POINT('Ctrl Pts',(-4.90600571704411,1.04520356973813,35.1759156781158));
#52156=CARTESIAN_POINT('Ctrl Pts',(-4.91256327647705,-0.00335788528186755,
35.2351405640092));
#52157=CARTESIAN_POINT('Origin',(0.,0.,-13.2351405640096));
#52158=CARTESIAN_POINT('',(-4.91445289798421,-0.00410312268860868,31.3898594359907));
#52159=CARTESIAN_POINT('',(-4.92540574744767,0.00198995367837004,31.7351405640093));
#52160=CARTESIAN_POINT('',(-4.91825,6.88216836313478E-12,-13.2351405640096));
#52161=CARTESIAN_POINT('Ctrl Pts',(-4.91445289798421,-0.00410312268860874,
31.3898594359907));
#52162=CARTESIAN_POINT('Ctrl Pts',(-4.9184858592771,-0.518003180154603,
31.4189136519305));
#52163=CARTESIAN_POINT('Ctrl Pts',(-4.60746921181795,-2.66837429237667,
31.540757626447));
#52164=CARTESIAN_POINT('Ctrl Pts',(-1.48635567043628,-5.62369832358916,
31.7553913595403));
#52165=CARTESIAN_POINT('Ctrl Pts',(3.92675811827154,-4.29136419968826,32.0337606352706));
#52166=CARTESIAN_POINT('Ctrl Pts',(5.73323152065607,0.982492923299337,32.3121299110009));
#52167=CARTESIAN_POINT('Ctrl Pts',(2.27385871511533,5.35395205035231,32.5904991867312));
#52168=CARTESIAN_POINT('Ctrl Pts',(-3.22498678761868,4.8127489975417,32.8664090283944));
#52169=CARTESIAN_POINT('Ctrl Pts',(-4.92259647513489,1.58708789756534,33.0495291114809));
#52170=CARTESIAN_POINT('Ctrl Pts',(-4.92620963101609,-0.00080908452636648,
33.1398594359907));
#52171=CARTESIAN_POINT('Ctrl Pts',(-4.92540574744767,0.0019899536783699,
31.7351405640093));
#52172=CARTESIAN_POINT('Ctrl Pts',(-4.91761491259624,-1.52019189598326,
31.8216948814096));
#52173=CARTESIAN_POINT('Ctrl Pts',(-3.34297940924432,-4.68844772092739,
32.0010571500257));
#52174=CARTESIAN_POINT('Ctrl Pts',(2.05548484168548,-5.44193959609919,32.2732273698575));
#52175=CARTESIAN_POINT('Ctrl Pts',(5.68939419901335,-1.21264922802275,32.5516512235046));
#52176=CARTESIAN_POINT('Ctrl Pts',(4.09584523280961,4.13083240169122,32.8300750771517));
#52177=CARTESIAN_POINT('Ctrl Pts',(-1.26099724149055,5.67887404851917,33.1084989307988));
#52178=CARTESIAN_POINT('Ctrl Pts',(-4.55347701854424,2.80085553305158,33.3268540930847));
#52179=CARTESIAN_POINT('Ctrl Pts',(-4.91669973643047,0.583067435438709,
33.4524013041548));
#52180=CARTESIAN_POINT('Ctrl Pts',(-4.91288232756503,0.0035217176248617,
33.4851405640092));
#52181=CARTESIAN_POINT('Origin',(0.,0.,-13.2351405640096));
#52182=CARTESIAN_POINT('',(-4.91141405521213,0.00256004678308836,29.6398594359907));
#52183=CARTESIAN_POINT('',(-4.91898260507021,-0.0044993792021053,29.9851405640093));
#52184=CARTESIAN_POINT('',(-4.91825,6.88216836313478E-12,-13.2351405640096));
#52185=CARTESIAN_POINT('Ctrl Pts',(-4.91141405521213,0.00256004678308774,
29.6398594359907));
#52186=CARTESIAN_POINT('Ctrl Pts',(-4.90678101561315,-0.983269338981918,
29.6955084338033));
#52187=CARTESIAN_POINT('Ctrl Pts',(-4.1401952484112,-3.6195129973856,29.8439471901927));
#52188=CARTESIAN_POINT('Ctrl Pts',(0.163218327990816,-5.81451595502028,
30.0851757051587));
#52189=CARTESIAN_POINT('Ctrl Pts',(4.97929477759872,-3.00696849527155,30.363544980889));
#52190=CARTESIAN_POINT('Ctrl Pts',(5.22199922429825,2.56241294782984,30.6419142566192));
#52191=CARTESIAN_POINT('Ctrl Pts',(0.668413007697845,5.77827483466457,30.9202835323496));
#52192=CARTESIAN_POINT('Ctrl Pts',(-3.95974774448338,3.90520013200073,31.16959859214));
#52193=CARTESIAN_POINT('Ctrl Pts',(-4.9056058866944,1.12322721352206,31.3261238933537));
#52194=CARTESIAN_POINT('Ctrl Pts',(-4.91445289798421,-0.00410312268860874,
31.3898594359907));
#52195=CARTESIAN_POINT('Ctrl Pts',(-4.91898260507021,-0.00449937920210593,
29.9851405640093));
#52196=CARTESIAN_POINT('Ctrl Pts',(-4.92230224163488,-0.361517893593529,
30.005372556233));
#52197=CARTESIAN_POINT('Ctrl Pts',(-4.72366297320252,-2.35258394513135,
30.1184124996724));
#52198=CARTESIAN_POINT('Ctrl Pts',(-2.01230599337432,-5.4580535991341,30.3242603943276));
#52199=CARTESIAN_POINT('Ctrl Pts',(3.50391824555016,-4.64352037041854,30.6026842479747));
#52200=CARTESIAN_POINT('Ctrl Pts',(5.80071595908955,0.437514415711182,30.8811081016218));
#52201=CARTESIAN_POINT('Ctrl Pts',(2.76777207587959,5.11655765510094,31.1595319552689));
#52202=CARTESIAN_POINT('Ctrl Pts',(-2.80822167689368,5.0944691102622,31.4379558089161));
#52203=CARTESIAN_POINT('Ctrl Pts',(-4.87269503648718,1.85355398490913,31.6298253451628));
#52204=CARTESIAN_POINT('Ctrl Pts',(-4.9259686428611,0.111969076315626,31.7288869301939));
#52205=CARTESIAN_POINT('Ctrl Pts',(-4.92540574744767,0.0019899536783699,
31.7351405640093));
#52206=CARTESIAN_POINT('Origin',(0.,0.,-13.2351405640096));
#52207=CARTESIAN_POINT('',(-4.92384460879403,0.00312281753491277,27.8898594359907));
#52208=CARTESIAN_POINT('',(-4.9100957742978,9.20690869954388E-5,28.2351405640093));
#52209=CARTESIAN_POINT('',(-4.91825,6.88216836313478E-12,-13.2351405640096));
#52210=CARTESIAN_POINT('Ctrl Pts',(-4.92384460879403,0.00312281753491236,
27.8898594359907));
#52211=CARTESIAN_POINT('Ctrl Pts',(-4.91313914334963,-1.44446164443976,
27.9721032156761));
#52212=CARTESIAN_POINT('Ctrl Pts',(-3.47225634574353,-4.54377938079009,
28.1471367539382));
#52213=CARTESIAN_POINT('Ctrl Pts',(1.79949035101865,-5.53146187642727,28.4149600507771));
#52214=CARTESIAN_POINT('Ctrl Pts',(5.62602862389248,-1.47751072311508,28.6933293265074));
#52215=CARTESIAN_POINT('Ctrl Pts',(4.28518417585832,3.93350131470056,28.9716986022376));
#52216=CARTESIAN_POINT('Ctrl Pts',(-0.991507056211286,5.73167948957902,
29.250067877968));
#52217=CARTESIAN_POINT('Ctrl Pts',(-4.48470808861617,2.95837594561327,29.4727881558856));
#52218=CARTESIAN_POINT('Ctrl Pts',(-4.9145061974271,0.660513555564752,29.6027186752265));
#52219=CARTESIAN_POINT('Ctrl Pts',(-4.91141405521213,0.00256004678308774,
29.6398594359907));
#52220=CARTESIAN_POINT('Ctrl Pts',(-4.9100957742978,9.20690869953694E-5,
28.2351405640093));
#52221=CARTESIAN_POINT('Ctrl Pts',(-4.9099580555162,-0.828071287137276,
28.2818581822721));
#52222=CARTESIAN_POINT('Ctrl Pts',(-4.31787178459561,-3.3016264176408,28.4213837517506));
#52223=CARTESIAN_POINT('Ctrl Pts',(-0.394927824289227,-5.80377088758623,
28.6537172724448));
#52224=CARTESIAN_POINT('Ctrl Pts',(4.6691125779863,-3.46974238756726,28.9321411260919));
#52225=CARTESIAN_POINT('Ctrl Pts',(5.4431371094098,2.0523116016232,29.210564979739));
#52226=CARTESIAN_POINT('Ctrl Pts',(1.215966189542,5.68868620402655,29.4889888333862));
#52227=CARTESIAN_POINT('Ctrl Pts',(-3.74008590277417,4.21382366772307,29.7471806948096));
#52228=CARTESIAN_POINT('Ctrl Pts',(-4.90707444474069,1.27619313853601,29.9125646050173));
#52229=CARTESIAN_POINT('Ctrl Pts',(-4.91898260507021,-0.00449937920210593,
29.9851405640093));
#52230=CARTESIAN_POINT('Origin',(0.,0.,-13.2351405640096));
#52231=CARTESIAN_POINT('',(-4.92121115498267,-0.00412874098909444,26.1398594359907));
#52232=CARTESIAN_POINT('',(-4.91932167294426,0.00446737670234801,26.4851405640093));
#52233=CARTESIAN_POINT('',(-4.91825,6.88216836313478E-12,-13.2351405640096));
#52234=CARTESIAN_POINT('Ctrl Pts',(-4.92121115498267,-0.00412874098909458,
26.1398594359907));
#52235=CARTESIAN_POINT('Ctrl Pts',(-4.92375232237933,-0.286999724354,26.1559082389721));
#52236=CARTESIAN_POINT('Ctrl Pts',(-4.77264664606773,-2.20263914365286,
26.2647468005303));
#52237=CARTESIAN_POINT('Ctrl Pts',(-2.25700960862895,-5.36107672397384,
26.4663751206653));
#52238=CARTESIAN_POINT('Ctrl Pts',(3.28910742006482,-4.79760444316246,26.7447443963955));
#52239=CARTESIAN_POINT('Ctrl Pts',(5.81425211003376,0.17236129132015,27.0231136721258));
#52240=CARTESIAN_POINT('Ctrl Pts',(2.99913497467191,4.98401699610638,27.3014829478561));
#52241=CARTESIAN_POINT('Ctrl Pts',(-2.57062122881967,5.21796344484313,27.5798522235863));
#52242=CARTESIAN_POINT('Ctrl Pts',(-4.83131394241821,2.00616851179972,27.7759777196312));
#52243=CARTESIAN_POINT('Ctrl Pts',(-4.92521735227726,0.188744091725602,
27.8793134570993));
#52244=CARTESIAN_POINT('Ctrl Pts',(-4.92384460879403,0.00312281753491236,
27.8898594359907));
#52245=CARTESIAN_POINT('Ctrl Pts',(-4.91932167294426,0.00446737670234811,
26.4851405640093));
#52246=CARTESIAN_POINT('Ctrl Pts',(-4.90731400357618,-1.28706604896177,
26.5583438083111));
#52247=CARTESIAN_POINT('Ctrl Pts',(-3.72359445036012,-4.23549576657875,
26.7243550038287));
#52248=CARTESIAN_POINT('Ctrl Pts',(1.2543743174442,-5.68034062127683,26.983174150562));
#52249=CARTESIAN_POINT('Ctrl Pts',(5.45687940832144,-2.01548793720741,27.2615980042091));
#52250=CARTESIAN_POINT('Ctrl Pts',(4.64556251996484,3.50121027290405,27.5400218578563));
#52251=CARTESIAN_POINT('Ctrl Pts',(-0.434132268219488,5.80097006333265,
27.8184457115034));
#52252=CARTESIAN_POINT('Ctrl Pts',(-4.32953501880666,3.27920418173089,28.0501519468877));
#52253=CARTESIAN_POINT('Ctrl Pts',(-4.91023164390618,0.817135536779907,
28.1890502310564));
#52254=CARTESIAN_POINT('Ctrl Pts',(-4.9100957742978,9.20690869953694E-5,
28.2351405640093));
#52255=CARTESIAN_POINT('Origin',(0.,0.,-13.2351405640096));
#52256=CARTESIAN_POINT('',(-4.91032113059727,-0.00108994245123004,24.3898594359907));
#52257=CARTESIAN_POINT('',(-4.92521571531249,-0.00217150628855023,24.7351405640093));
#52258=CARTESIAN_POINT('',(-4.91825,6.88216836313478E-12,-13.2351405640096));
#52259=CARTESIAN_POINT('Ctrl Pts',(-4.91032113059727,-0.00108994245122979,
24.3898594359907));
#52260=CARTESIAN_POINT('Ctrl Pts',(-4.91181354648729,-0.756946751686931,
24.4325030208449));
#52261=CARTESIAN_POINT('Ctrl Pts',(-4.39180191053746,-3.15555433076574,
24.5679363642759));
#52262=CARTESIAN_POINT('Ctrl Pts',(-0.650237370706631,-5.78034837838638,
24.7961594662836));
#52263=CARTESIAN_POINT('Ctrl Pts',(4.51066864926873,-3.67275160476199,25.0745287420139));
#52264=CARTESIAN_POINT('Ctrl Pts',(5.52862538900271,1.8081861966767,25.3528980177442));
#52265=CARTESIAN_POINT('Ctrl Pts',(1.46866212239656,5.62834501288036,25.6312672934744));
#52266=CARTESIAN_POINT('Ctrl Pts',(-3.62839605704299,4.35678761453777,25.8935877662233));
#52267=CARTESIAN_POINT('Ctrl Pts',(-4.90905999239607,1.34848239136343,26.0631184803953));
#52268=CARTESIAN_POINT('Ctrl Pts',(-4.92121115498267,-0.00412874098909458,
26.1398594359907));
#52269=CARTESIAN_POINT('Ctrl Pts',(-4.92521571531249,-0.00217150628855014,
24.7351405640093));
#52270=CARTESIAN_POINT('Ctrl Pts',(-4.92588279180187,-0.123194721221349,
24.7420214831345));
#52271=CARTESIAN_POINT('Ctrl Pts',(-4.86688107224675,-1.8758844913496,24.8417103534754));
#52272=CARTESIAN_POINT('Ctrl Pts',(-2.77373655046063,-5.11332671072659,
25.0342071750321));
#52273=CARTESIAN_POINT('Ctrl Pts',(2.80227916848797,-5.09774028014861,25.3126310286793));
#52274=CARTESIAN_POINT('Ctrl Pts',(5.80353964078615,-0.39831161144852,25.5910548823263));
#52275=CARTESIAN_POINT('Ctrl Pts',(3.47246409628408,4.66708877160151,25.8694787359735));
#52276=CARTESIAN_POINT('Ctrl Pts',(-2.04913766389717,5.44433277237802,26.1479025896206));
#52277=CARTESIAN_POINT('Ctrl Pts',(-4.73125224331919,2.33013357115337,26.3531231989659));
#52278=CARTESIAN_POINT('Ctrl Pts',(-4.9225374708358,0.350355520336658,26.4655358570954));
#52279=CARTESIAN_POINT('Ctrl Pts',(-4.91932167294426,0.00446737670234811,
26.4851405640093));
#52280=CARTESIAN_POINT('Origin',(0.,0.,-13.2351405640096));
#52281=CARTESIAN_POINT('',(-4.91719942584508,0.00452867428901858,22.6398594359907));
#52282=CARTESIAN_POINT('',(-4.91264357795,-0.00340089404915922,22.9851405640093));
#52283=CARTESIAN_POINT('',(-4.91825,6.88216836313478E-12,-13.2351405640096));
#52284=CARTESIAN_POINT('Ctrl Pts',(-4.91719942584508,0.0045286742890192,
22.6398594359907));
#52285=CARTESIAN_POINT('Ctrl Pts',(-4.90612996717293,-1.21840033721416,
22.7090978027177));
#52286=CARTESIAN_POINT('Ctrl Pts',(-3.82588241968382,-4.09768835375591,
22.8711259280215));
#52287=CARTESIAN_POINT('Ctrl Pts',(1.00952794474132,-5.72853291363189,23.1259438119021));
#52288=CARTESIAN_POINT('Ctrl Pts',(5.36461918091565,-2.24857667370483,23.4043130876322));
#52289=CARTESIAN_POINT('Ctrl Pts',(4.79242648149282,3.29664745359036,23.6826823633626));
#52290=CARTESIAN_POINT('Ctrl Pts',(-0.181503828456812,5.8139738883171,23.9610516390928));
#52291=CARTESIAN_POINT('Ctrl Pts',(-4.25230501364173,3.42370234687152,24.1967773299688));
#52292=CARTESIAN_POINT('Ctrl Pts',(-4.90856614337602,0.887750125635713,
24.3397132622682));
#52293=CARTESIAN_POINT('Ctrl Pts',(-4.91032113059727,-0.00108994245122979,
24.3898594359907));
#52294=CARTESIAN_POINT('Ctrl Pts',(-4.91264357795,-0.00340089404915991,
22.9851405640093));
#52295=CARTESIAN_POINT('Ctrl Pts',(-4.916389164947,-0.594122806234998,23.0185071091736));
#52296=CARTESIAN_POINT('Ctrl Pts',(-4.54396316738755,-2.82335358446512,
23.1446816055536));
#52297=CARTESIAN_POINT('Ctrl Pts',(-1.222598871385,-5.68726441285079,23.3636640531493));
#52298=CARTESIAN_POINT('Ctrl Pts',(4.12366191086833,-4.10306433618151,23.6420879067964));
#52299=CARTESIAN_POINT('Ctrl Pts',(5.68107101131397,1.25106221523925,23.9205117604436));
#52300=CARTESIAN_POINT('Ctrl Pts',(2.01866919589476,5.45570336249478,24.1989356140907));
#52301=CARTESIAN_POINT('Ctrl Pts',(-3.36215071414575,4.66757434112606,24.4704785486126));
#52302=CARTESIAN_POINT('Ctrl Pts',(-4.91688544694772,1.50913323134417,24.6492135319188));
#52303=CARTESIAN_POINT('Ctrl Pts',(-4.92521571531249,-0.00217150628855014,
24.7351405640093));
#52304=CARTESIAN_POINT('Origin',(0.,0.,-13.2351405640096));
#52305=CARTESIAN_POINT('',(-4.92612628624265,-0.000997778412739117,20.8898594359907));
#52306=CARTESIAN_POINT('',(-4.91279890386086,0.00348065594282992,21.2351405640093));
#52307=CARTESIAN_POINT('',(-4.91825,6.88216836313478E-12,-13.2351405640096));
#52308=CARTESIAN_POINT('Ctrl Pts',(-4.92612628624265,-0.000997778412738558,
20.8898594359907));
#52309=CARTESIAN_POINT('Ctrl Pts',(-4.9262742113422,-0.0544992921925554,
20.8929028260137));
#52310=CARTESIAN_POINT('Ctrl Pts',(-4.90121217819937,-1.73906368377049,
20.9887359746135));
#52311=CARTESIAN_POINT('Ctrl Pts',(-2.98344570524222,-4.99342444997913,
21.1773588817902));
#52312=CARTESIAN_POINT('Ctrl Pts',(2.58701870162035,-5.20985318902981,21.4557281575204));
#52313=CARTESIAN_POINT('Ctrl Pts',(5.7813637121742,-0.641147129240114,21.7340974332507));
#52314=CARTESIAN_POINT('Ctrl Pts',(3.66565416262452,4.51643837263511,22.0124667089809));
#52315=CARTESIAN_POINT('Ctrl Pts',(-1.81687757128598,5.5257752311088,22.2908359847112));
#52316=CARTESIAN_POINT('Ctrl Pts',(-4.68205429258674,2.47113126762697,22.4999668937145));
#52317=CARTESIAN_POINT('Ctrl Pts',(-4.92096469604245,0.420507295909191,
22.616308044141));
#52318=CARTESIAN_POINT('Ctrl Pts',(-4.91719942584508,0.0045286742890192,
22.6398594359907));
#52319=CARTESIAN_POINT('Ctrl Pts',(-4.91279890386086,0.00348065594282986,
21.2351405640093));
#52320=CARTESIAN_POINT('Ctrl Pts',(-4.90590889642109,-1.05605914474809,
21.2949927352127));
#52321=CARTESIAN_POINT('Ctrl Pts',(-4.04869927458494,-3.76870392438603,
21.4476528576317));
#52322=CARTESIAN_POINT('Ctrl Pts',(0.427367531648445,-5.80147235578038,
21.6931209312665));
#52323=CARTESIAN_POINT('Ctrl Pts',(5.1117086309249,-2.77671737390015,21.9715447849137));
#52324=CARTESIAN_POINT('Ctrl Pts',(5.09937326597762,2.79930648486794,22.2499686385608));
#52325=CARTESIAN_POINT('Ctrl Pts',(0.401695263205706,5.80330642112832,22.5283924922079));
#52326=CARTESIAN_POINT('Ctrl Pts',(-4.05785882761375,3.75418866842352,22.7734498006908));
#52327=CARTESIAN_POINT('Ctrl Pts',(-4.90597093754048,1.04895082150337,22.9256991579579));
#52328=CARTESIAN_POINT('Ctrl Pts',(-4.91264357795,-0.00340089404915991,
22.9851405640093));
#52329=CARTESIAN_POINT('Origin',(0.,0.,-13.2351405640096));
#52330=CARTESIAN_POINT('',(-4.91418689020212,-0.00402515463966349,19.1398594359907));
#52331=CARTESIAN_POINT('',(-4.92534177178078,0.00205314599783006,19.4851405640093));
#52332=CARTESIAN_POINT('',(-4.91825,6.88216836313478E-12,-13.2351405640096));
#52333=CARTESIAN_POINT('Ctrl Pts',(-4.91418689020212,-0.00402515463966295,
19.1398594359907));
#52334=CARTESIAN_POINT('Ctrl Pts',(-4.91820769545533,-0.528325596070794,
19.1694976078865));
#52335=CARTESIAN_POINT('Ctrl Pts',(-4.59913644360476,-2.68931479280248,
19.2919255383591));
#52336=CARTESIAN_POINT('Ctrl Pts',(-1.45095404829527,-5.63293603403351,
19.5071432274085));
#52337=CARTESIAN_POINT('Ctrl Pts',(3.95367247989527,-4.26658059053105,19.7855125031388));
#52338=CARTESIAN_POINT('Ctrl Pts',(5.72693837654226,1.01853465579974,20.063881778869));
#52339=CARTESIAN_POINT('Ctrl Pts',(2.24013817879126,5.36814837292146,20.3422510545993));
#52340=CARTESIAN_POINT('Ctrl Pts',(-3.24356373581575,4.79358773299822,20.6175769403066));
#52341=CARTESIAN_POINT('Ctrl Pts',(-4.92176413075087,1.57670555159041,20.800113067437));
#52342=CARTESIAN_POINT('Ctrl Pts',(-4.92612628624265,-0.000997778412738558,
20.8898594359907));
#52343=CARTESIAN_POINT('Ctrl Pts',(-4.92534177178078,0.00205314599783015,
19.4851405640093));
#52344=CARTESIAN_POINT('Ctrl Pts',(-4.91736014737601,-1.516373211075,19.5714783612517));
#52345=CARTESIAN_POINT('Ctrl Pts',(-3.34961135330605,-4.68124800098687,
19.7506241097099));
#52346=CARTESIAN_POINT('Ctrl Pts',(2.04278769977008,-5.44671854566206,20.0225778093838));
#52347=CARTESIAN_POINT('Ctrl Pts',(5.68655061714523,-1.22591458945406,20.3010016630309));
#52348=CARTESIAN_POINT('Ctrl Pts',(4.10546791546748,4.12126894257805,20.579425516678));
#52349=CARTESIAN_POINT('Ctrl Pts',(-1.2477496877477,5.68179947012534,20.8578493703251));
#52350=CARTESIAN_POINT('Ctrl Pts',(-4.55020400913313,2.80862120793031,21.0764210527689));
#52351=CARTESIAN_POINT('Ctrl Pts',(-4.91659267716771,0.586884062767262,
21.202184783997));
#52352=CARTESIAN_POINT('Ctrl Pts',(-4.91279890386086,0.00348065594282986,
21.2351405640093));
#52353=CARTESIAN_POINT('Origin',(0.,0.,-13.2351405640096));
#52354=CARTESIAN_POINT('',(-4.91158062171437,0.00270053279499022,17.3898594359907));
#52355=CARTESIAN_POINT('',(-4.91909967221345,-0.00448925516201348,17.7351405640093));
#52356=CARTESIAN_POINT('',(-4.91825,6.88216836313478E-12,-13.2351405640096));
#52357=CARTESIAN_POINT('Ctrl Pts',(-4.91158062171437,0.00270053279499041,
17.3898594359907));
#52358=CARTESIAN_POINT('Ctrl Pts',(-4.90663216249858,-0.993389185122712,
17.4460923897593));
#52359=CARTESIAN_POINT('Ctrl Pts',(-4.127797895462,-3.64023466456982,17.5951151021047));
#52360=CARTESIAN_POINT('Ctrl Pts',(0.199787533727289,-5.81337431748075,
17.8369275730269));
#52361=CARTESIAN_POINT('Ctrl Pts',(4.99810966208265,-2.97558999520659,18.1152968487571));
#52362=CARTESIAN_POINT('Ctrl Pts',(5.20577873272567,2.59520785288553,18.3936661244875));
#52363=CARTESIAN_POINT('Ctrl Pts',(0.632055302428017,5.78236475055406,18.6720354002177));
#52364=CARTESIAN_POINT('Ctrl Pts',(-3.97342008071557,3.88467195111445,18.9207665040521));
#52365=CARTESIAN_POINT('Ctrl Pts',(-4.90561955236608,1.11312892929739,19.0767078493098));
#52366=CARTESIAN_POINT('Ctrl Pts',(-4.91418689020212,-0.00402515463966295,
19.1398594359907));
#52367=CARTESIAN_POINT('Ctrl Pts',(-4.91909967221345,-0.00448925516201404,
17.7351405640093));
#52368=CARTESIAN_POINT('Ctrl Pts',(-4.92238407305303,-0.357665457469601,
17.7551560360751));
#52369=CARTESIAN_POINT('Ctrl Pts',(-4.72629246046279,-2.34483425780271,
17.8679794593566));
#52370=CARTESIAN_POINT('Ctrl Pts',(-2.02502965350643,-5.45334570739934,
18.0736108338538));
#52371=CARTESIAN_POINT('Ctrl Pts',(3.49307921743211,-4.65167949054264,18.352034687501));
#52372=CARTESIAN_POINT('Ctrl Pts',(5.80172054381419,0.4239849448688,18.6304585411481));
#52373=CARTESIAN_POINT('Ctrl Pts',(2.77969725342115,5.11008881344677,18.9088823947953));
#52374=CARTESIAN_POINT('Ctrl Pts',(-2.79633284965052,5.10100451832347,19.1873062484423));
#52375=CARTESIAN_POINT('Ctrl Pts',(-4.8706972056682,1.86126106698695,19.379392304847));
#52376=CARTESIAN_POINT('Ctrl Pts',(-4.92593991466264,0.115844007487335,
19.478670410036));
#52377=CARTESIAN_POINT('Ctrl Pts',(-4.92534177178078,0.00205314599783015,
19.4851405640093));
#52378=CARTESIAN_POINT('Origin',(0.,0.,-13.2351405640096));
#52379=CARTESIAN_POINT('',(-4.92408796408552,0.00298446262078338,15.6398594359907));
#52380=CARTESIAN_POINT('',(-4.9100940628477,2.85129012446328E-5,15.9851405640093));
#52381=CARTESIAN_POINT('',(-4.91825,6.88216836313478E-12,-13.2351405640096));
#52382=CARTESIAN_POINT('Ctrl Pts',(-4.92408796408553,0.00298446262078356,
15.6398594359907));
#52383=CARTESIAN_POINT('Ctrl Pts',(-4.91367855042134,-1.45468920093622,
15.7226871716321));
#52384=CARTESIAN_POINT('Ctrl Pts',(-3.45511568541442,-4.56344829093663,
15.8983046658504));
#52385=CARTESIAN_POINT('Ctrl Pts',(1.83424682140562,-5.52003393213674,16.1667119186453));
#52386=CARTESIAN_POINT('Ctrl Pts',(5.63521065484668,-1.44209461869877,16.4450811943755));
#52387=CARTESIAN_POINT('Ctrl Pts',(4.26035827525457,3.96037667151086,16.7234504701058));
#52388=CARTESIAN_POINT('Ctrl Pts',(-1.02753884835743,5.7253296786206,17.0018197458361));
#52389=CARTESIAN_POINT('Ctrl Pts',(-4.49411412142162,2.93743814234507,17.2239560677977));
#52390=CARTESIAN_POINT('Ctrl Pts',(-4.91479759406829,0.65025423483065,17.3533026311826));
#52391=CARTESIAN_POINT('Ctrl Pts',(-4.91158062171437,0.00270053279499041,
17.3898594359907));
#52392=CARTESIAN_POINT('Ctrl Pts',(-4.91009437976676,2.85117933054163E-5,
15.9851405640093));
#52393=CARTESIAN_POINT('Ctrl Pts',(-4.91005192958233,-0.824297174460165,
16.0316416621142));
#52394=CARTESIAN_POINT('Ctrl Pts',(-4.32190952287306,-3.29388776939099,
16.1709507114348));
#52395=CARTESIAN_POINT('Ctrl Pts',(-0.408462155912262,-5.8028340635571,
16.4030677119711));
#52396=CARTESIAN_POINT('Ctrl Pts',(4.66100783600869,-3.48062213614987,16.6814915656182));
#52397=CARTESIAN_POINT('Ctrl Pts',(5.4479086551669,2.03961167552763,16.9599154192653));
#52398=CARTESIAN_POINT('Ctrl Pts',(1.22922989078505,5.68583488835121,17.2383392729125));
#52399=CARTESIAN_POINT('Ctrl Pts',(-3.73440738737732,4.22130761444361,17.4967476544938));
#52400=CARTESIAN_POINT('Ctrl Pts',(-4.90715492872457,1.27994566889007,17.6623480848594));
#52401=CARTESIAN_POINT('Ctrl Pts',(-4.91909967221345,-0.00448925516201404,
17.7351405640093));
#52402=CARTESIAN_POINT('Origin',(0.,0.,-13.2351405640096));
#52403=CARTESIAN_POINT('',(-4.92090615674067,-0.00420134538231084,13.8898594359907));
#52404=CARTESIAN_POINT('',(-4.91920467447417,0.00447934526514732,14.2351405640093));
#52405=CARTESIAN_POINT('',(-4.91825,6.88216836313478E-12,-13.2351405640096));
#52406=CARTESIAN_POINT('Ctrl Pts',(-4.92090615674067,-0.00420134538231042,
13.8898594359907));
#52407=CARTESIAN_POINT('Ctrl Pts',(-4.92356576649449,-0.297411916716882,
13.9064921949282));
#52408=CARTESIAN_POINT('Ctrl Pts',(-4.76604114686728,-2.22351334540009,
14.0159147124424));
#52409=CARTESIAN_POINT('Ctrl Pts',(-2.22324459247222,-5.3751669272517,14.2181269885334));
#52410=CARTESIAN_POINT('Ctrl Pts',(3.31921857055293,-4.77682154729211,14.4964962642637));
#52411=CARTESIAN_POINT('Ctrl Pts',(5.81305296984359,0.208928656651545,14.774865539994));
#52412=CARTESIAN_POINT('Ctrl Pts',(2.96772692751709,5.00278251550746,15.0532348157242));
#52413=CARTESIAN_POINT('Ctrl Pts',(-2.60339058705663,5.2016914042456,15.3316040914545));
#52414=CARTESIAN_POINT('Ctrl Pts',(-4.83716603141205,1.98534572792005,15.5271456315433));
#52415=CARTESIAN_POINT('Ctrl Pts',(-4.92533994588682,0.178304702346117,
15.6298974130554));
#52416=CARTESIAN_POINT('Ctrl Pts',(-4.92408796408553,0.00298446262078356,
15.6398594359907));
#52417=CARTESIAN_POINT('Ctrl Pts',(-4.91920467447417,0.00447934526514739,
14.2351405640093));
#52418=CARTESIAN_POINT('Ctrl Pts',(-4.90722910644829,-1.28331256696772,
14.3081272881532));
#52419=CARTESIAN_POINT('Ctrl Pts',(-3.72930065287923,-4.22801859829677,
14.4739219635129));
#52420=CARTESIAN_POINT('Ctrl Pts',(1.2411233614091,-5.68325059308101,14.7325245900883));
#52421=CARTESIAN_POINT('Ctrl Pts',(5.45216409893207,-2.0282088502685,15.0109484437354));
#52422=CARTESIAN_POINT('Ctrl Pts',(4.65371531907096,3.49036648950155,15.2893722973825));
#52423=CARTESIAN_POINT('Ctrl Pts',(-0.420602213959508,5.80196675960862,
15.5677961510297));
#52424=CARTESIAN_POINT('Ctrl Pts',(-4.32552115167899,3.2869445013678,15.7997189065719));
#52425=CARTESIAN_POINT('Ctrl Pts',(-4.91013665262773,0.820910814028876,
15.9388337108985));
#52426=CARTESIAN_POINT('Ctrl Pts',(-4.91009437976676,2.85117933054163E-5,
15.9851405640093));
#52427=CARTESIAN_POINT('Origin',(0.,0.,-13.2351405640096));
#52428=CARTESIAN_POINT('',(-4.91025820404979,-0.000922789237043502,12.1398594359907));
#52429=CARTESIAN_POINT('',(-4.92528291799711,-0.00210936955439167,12.4851405640093));
#52430=CARTESIAN_POINT('',(-4.91825,6.88216836313478E-12,-13.2351405640096));
#52431=CARTESIAN_POINT('Ctrl Pts',(-4.91025820404979,-0.000922789237043017,
12.1398594359907));
#52432=CARTESIAN_POINT('Ctrl Pts',(-4.91153813360514,-0.767154694837722,
12.183086976801));
#52433=CARTESIAN_POINT('Ctrl Pts',(-4.38148269050377,-3.17645995727246,
12.319104276188));
#52434=CARTESIAN_POINT('Ctrl Pts',(-0.613866982695112,-5.78432393122432,
12.5479113341518));
#52435=CARTESIAN_POINT('Ctrl Pts',(4.53368047982022,-3.64430752279149,12.8262806098821));
#52436=CARTESIAN_POINT('Ctrl Pts',(5.51714280525491,1.84292465396758,13.1046498856123));
#52437=CARTESIAN_POINT('Ctrl Pts',(1.43323162327729,5.63747134164028,13.3830191613426));
#52438=CARTESIAN_POINT('Ctrl Pts',(-3.64439920708976,4.33678131162103,13.6447556781354));
#52439=CARTESIAN_POINT('Ctrl Pts',(-4.90872850781162,1.33833223303946,13.8137024363514));
#52440=CARTESIAN_POINT('Ctrl Pts',(-4.92090615674067,-0.00420134538231042,
13.8898594359907));
#52441=CARTESIAN_POINT('Ctrl Pts',(-4.92528291799711,-0.0021093695543929,
12.4851405640093));
#52442=CARTESIAN_POINT('Ctrl Pts',(-4.92591332939639,-0.119320139238976,
12.4918049629766));
#52443=CARTESIAN_POINT('Ctrl Pts',(-4.86889685925445,-1.86817592601175,
12.5912773131596));
#52444=CARTESIAN_POINT('Ctrl Pts',(-2.78565417665601,-5.10684396766439,
12.7835576145584));
#52445=CARTESIAN_POINT('Ctrl Pts',(2.79038272846711,-5.10426182034811,13.0619814682055));
#52446=CARTESIAN_POINT('Ctrl Pts',(5.80259492580427,-0.411845394561442,
13.3404053218526));
#52447=CARTESIAN_POINT('Ctrl Pts',(3.48333911759557,4.65897768762844,13.6188291754998));
#52448=CARTESIAN_POINT('Ctrl Pts',(-2.03643495793874,5.4490969127073,13.8972530291469));
#52449=CARTESIAN_POINT('Ctrl Pts',(-4.72864254700507,2.33788227941386,14.1026901586501));
#52450=CARTESIAN_POINT('Ctrl Pts',(-4.9224569159734,0.354208918867955,14.2153193369375));
#52451=CARTESIAN_POINT('Ctrl Pts',(-4.91920467447417,0.00447934526514739,
14.2351405640093));
#52452=CARTESIAN_POINT('Origin',(0.,0.,-13.2351405640096));
#52453=CARTESIAN_POINT('',(-4.91750913335068,0.00453909766118435,10.3898594359907));
#52454=CARTESIAN_POINT('',(-4.91272496910331,-0.00344323922728262,10.7351405640093));
#52455=CARTESIAN_POINT('',(-4.91825,6.88216836313478E-12,-13.2351405640096));
#52456=CARTESIAN_POINT('Ctrl Pts',(-4.91750913335068,0.00453909766118428,
10.3898594359907));
#52457=CARTESIAN_POINT('Ctrl Pts',(-4.90626050624057,-1.22850621016978,
10.4596817586738));
#52458=CARTESIAN_POINT('Ctrl Pts',(-3.81113729750009,-4.11800395470607,
10.6222938399336));
#52459=CARTESIAN_POINT('Ctrl Pts',(1.04553958891947,-5.72206981622731,10.8776956797702));
#52460=CARTESIAN_POINT('Ctrl Pts',(5.37865627222158,-2.214789542839,11.1560649555005));
#52461=CARTESIAN_POINT('Ctrl Pts',(4.77159626236785,3.32672588632348,11.4344342312307));
#52462=CARTESIAN_POINT('Ctrl Pts',(-0.218069262963983,5.81271724844138,
11.712803506961));
#52463=CARTESIAN_POINT('Ctrl Pts',(-4.2637084465507,3.40287291834831,11.947945241881));
#52464=CARTESIAN_POINT('Ctrl Pts',(-4.90879071026785,0.877594745028542,
12.0902972182242));
#52465=CARTESIAN_POINT('Ctrl Pts',(-4.91025820404979,-0.000922789237043017,
12.1398594359907));
#52466=CARTESIAN_POINT('Ctrl Pts',(-4.91272496910331,-0.00344323922728276,
10.7351405640093));
#52467=CARTESIAN_POINT('Ctrl Pts',(-4.91649650272064,-0.590307466122425,
10.7682905890157));
#52468=CARTESIAN_POINT('Ctrl Pts',(-4.54725795767594,-2.81558795146297,
10.8942485652378));
#52469=CARTESIAN_POINT('Ctrl Pts',(-1.23585923872538,-5.68439763247154,
11.1130144926756));
#52470=CARTESIAN_POINT('Ctrl Pts',(4.11408163504771,-4.11267027637206,11.3914383463227));
#52471=CARTESIAN_POINT('Ctrl Pts',(5.683973256732,1.23780956481465,11.6698621999699));
#52472=CARTESIAN_POINT('Ctrl Pts',(2.03138735756037,5.45098063705376,11.948286053617));
#52473=CARTESIAN_POINT('Ctrl Pts',(-3.35554793119657,4.67478434679984,12.2200455082968));
#52474=CARTESIAN_POINT('Ctrl Pts',(-4.91713426459589,1.51294879426531,12.3989970117609));
#52475=CARTESIAN_POINT('Ctrl Pts',(-4.92528291799711,-0.0021093695543929,
12.4851405640093));
#52476=CARTESIAN_POINT('Origin',(0.,0.,-13.2351405640096));
#52477=CARTESIAN_POINT('',(-4.92602698002101,-0.00118436696873579,8.63985943599069));
#52478=CARTESIAN_POINT('',(-4.91271654582281,0.00343891372668881,8.98514056400927));
#52479=CARTESIAN_POINT('',(-4.91825,6.88216836313478E-12,-13.2351405640096));
#52480=CARTESIAN_POINT('Ctrl Pts',(-4.92602698002101,-0.00118436696873587,
8.6398594359907));
#52481=CARTESIAN_POINT('Ctrl Pts',(-4.92623328301914,-0.0649550216871807,
8.64348678196981));
#52482=CARTESIAN_POINT('Ctrl Pts',(-4.89617722538597,-1.75981957052431,
8.73990388652567));
#52483=CARTESIAN_POINT('Ctrl Pts',(-2.9519787969659,-5.01209110013389,8.92911074965828));
#52484=CARTESIAN_POINT('Ctrl Pts',(2.61973672319965,-5.19347817121596,9.20748002538857));
#52485=CARTESIAN_POINT('Ctrl Pts',(5.7852820686703,-0.60477053474805,9.48584930111882));
#52486=CARTESIAN_POINT('Ctrl Pts',(3.63717393035499,4.53940544720601,9.7642185768491));
#52487=CARTESIAN_POINT('Ctrl Pts',(-1.8515979295839,5.51423803629642,10.0425878525794));
#52488=CARTESIAN_POINT('Ctrl Pts',(-4.68955809926782,2.45021259625737,10.2511348056266));
#52489=CARTESIAN_POINT('Ctrl Pts',(-4.921209269813,0.410138452901258,10.366892000097));
#52490=CARTESIAN_POINT('Ctrl Pts',(-4.91750913335068,0.00453909766118428,
10.3898594359907));
#52491=CARTESIAN_POINT('Ctrl Pts',(-4.91271654582281,0.00343891372668881,
8.98514056400927));
#52492=CARTESIAN_POINT('Ctrl Pts',(-4.90594095198635,-1.05231235329147,
9.04477621505475));
#52493=CARTESIAN_POINT('Ctrl Pts',(-4.05353352444506,-3.76105365087587,
9.19721981731594));
#52494=CARTESIAN_POINT('Ctrl Pts',(0.413836324351832,-5.80245327414518,
9.44247137079281));
#52495=CARTESIAN_POINT('Ctrl Pts',(5.10521894046314,-2.78863121834486,9.72089522443996));
#52496=CARTESIAN_POINT('Ctrl Pts',(5.10588786891966,2.78740624452375,9.99931907808708));
#52497=CARTESIAN_POINT('Ctrl Pts',(0.415228493207719,5.80235381551483,10.2777429317342));
#52498=CARTESIAN_POINT('Ctrl Pts',(-4.05303681619496,3.7618407912721,10.5230167603749));
#52499=CARTESIAN_POINT('Ctrl Pts',(-4.90593758736845,1.05269782661613,10.6754826378));
#52500=CARTESIAN_POINT('Ctrl Pts',(-4.91272496910331,-0.00344323922728276,
10.7351405640093));
#52501=CARTESIAN_POINT('Origin',(0.,0.,-13.2351405640096));
#52502=CARTESIAN_POINT('',(-4.9139270378835,-0.00394135086111479,6.88985943599069));
#52503=CARTESIAN_POINT('',(-4.92527608168861,0.00211578826967762,7.23514056400927));
#52504=CARTESIAN_POINT('',(-4.91825,6.88216836313478E-12,-13.2351405640096));
#52505=CARTESIAN_POINT('Ctrl Pts',(-4.9139270378835,-0.00394135086111511,
6.88985943599069));
#52506=CARTESIAN_POINT('Ctrl Pts',(-4.9179273163929,-0.538643264396417,
6.9200815638426));
#52507=CARTESIAN_POINT('Ctrl Pts',(-4.59072219571754,-2.71025635333059,
7.04309345027126));
#52508=CARTESIAN_POINT('Ctrl Pts',(-1.41549502262945,-5.64195089084342,
7.25889509527668));
#52509=CARTESIAN_POINT('Ctrl Pts',(3.98043042392857,-4.24162818432278,7.53726437100694));
#52510=CARTESIAN_POINT('Ctrl Pts',(5.72041865981625,1.05453609241393,7.81563364673722));
#52511=CARTESIAN_POINT('Ctrl Pts',(2.20632901676084,5.38213231754632,8.09400292246748));
#52512=CARTESIAN_POINT('Ctrl Pts',(-3.2620276900715,4.77438313269691,8.36874485221864));
#52513=CARTESIAN_POINT('Ctrl Pts',(-4.92095592444886,1.56633785461507,8.55069702339305));
#52514=CARTESIAN_POINT('Ctrl Pts',(-4.92602698002101,-0.00118436696873587,
8.6398594359907));
#52515=CARTESIAN_POINT('Ctrl Pts',(-4.92527608168861,0.00211578826967746,
7.23514056400927));
#52516=CARTESIAN_POINT('Ctrl Pts',(-4.91710852250278,-1.5125561816081,7.32126184109382));
#52517=CARTESIAN_POINT('Ctrl Pts',(-3.35622792132889,-4.67404284470821,
7.50019106939408));
#52518=CARTESIAN_POINT('Ctrl Pts',(2.03007944704129,-5.45146787027966,7.77192824891004));
#52519=CARTESIAN_POINT('Ctrl Pts',(5.68367610587452,-1.23917328308113,8.05035210255719));
#52520=CARTESIAN_POINT('Ctrl Pts',(4.11506826830211,4.1116830676992,8.32877595620429));
#52521=CARTESIAN_POINT('Ctrl Pts',(-1.23449534743867,5.68469398817063,8.60719980985145));
#52522=CARTESIAN_POINT('Ctrl Pts',(-4.54691952667732,2.81638686581082,8.82598801245309));
#52523=CARTESIAN_POINT('Ctrl Pts',(-4.9164854664036,0.590700012090972,8.95196826383904));
#52524=CARTESIAN_POINT('Ctrl Pts',(-4.91271654582281,0.00343891372668881,
8.98514056400927));
#52525=CARTESIAN_POINT('Origin',(0.,0.,-13.2351405640096));
#52526=CARTESIAN_POINT('',(-4.91175629129765,0.0028372364354037,5.13985943599068));
#52527=CARTESIAN_POINT('',(-4.91921671359201,-0.00447815882576141,5.48514056400926));
#52528=CARTESIAN_POINT('',(-4.91825,6.88216836313478E-12,-13.2351405640096));
#52529=CARTESIAN_POINT('Ctrl Pts',(-4.91175629129765,0.00283723643540366,
5.13985943599068));
#52530=CARTESIAN_POINT('Ctrl Pts',(-4.90649215527958,-1.00350635860451,
5.19667634571539));
#52531=CARTESIAN_POINT('Ctrl Pts',(-4.11530325360641,-3.66094378176031,
5.34628301401685));
#52532=CARTESIAN_POINT('Ctrl Pts',(0.236348835348182,-5.81200268769786,
5.58867944089506));
#52533=CARTESIAN_POINT('Ctrl Pts',(5.01672680831839,-2.94409377304407,5.86704871662534));
#52534=CARTESIAN_POINT('Ctrl Pts',(5.18935228697503,2.62790008475296,6.1454179923556));
#52535=CARTESIAN_POINT('Ctrl Pts',(0.59567259140266,5.78622590101952,6.42378726808587));
#52536=CARTESIAN_POINT('Ctrl Pts',(-3.98699126429463,3.86412609996948,6.67193441596424));
#52537=CARTESIAN_POINT('Ctrl Pts',(-4.90564542549013,1.10303007212689,6.82729180526584));
#52538=CARTESIAN_POINT('Ctrl Pts',(-4.9139270378835,-0.00394135086111511,
6.88985943599069));
#52539=CARTESIAN_POINT('Ctrl Pts',(-4.91921671359201,-0.00447815882576173,
5.48514056400926));
#52540=CARTESIAN_POINT('Ctrl Pts',(-4.92246523460304,-0.35381251212689,
5.50493951591718));
#52541=CARTESIAN_POINT('Ctrl Pts',(-4.72891150816308,-2.33708508363489,
5.6175464190408));
#52542=CARTESIAN_POINT('Ctrl Pts',(-2.03774229941179,-5.44860815467391,
5.82296127338016));
#52543=CARTESIAN_POINT('Ctrl Pts',(3.48222119030037,-4.65981330997436,6.10138512702726));
#52544=CARTESIAN_POINT('Ctrl Pts',(5.8026935727219,0.410453167953449,6.37980898067441));
#52545=CARTESIAN_POINT('Ctrl Pts',(2.79160731206521,5.10359217779156,6.65823283432152));
#52546=CARTESIAN_POINT('Ctrl Pts',(-2.78442881302834,5.10751218179347,6.93665668796867));
#52547=CARTESIAN_POINT('Ctrl Pts',(-4.86868991641874,1.86896893191072,7.12895926453124));
#52548=CARTESIAN_POINT('Ctrl Pts',(-4.92591023167537,0.119718757257634,
7.22845388987811));
#52549=CARTESIAN_POINT('Ctrl Pts',(-4.92527608168861,0.00211578826967746,
7.23514056400927));
#52550=CARTESIAN_POINT('Origin',(0.,0.,-13.2351405640096));
#52551=CARTESIAN_POINT('',(-4.92432229863308,0.00284067633764219,3.38985943599068));
#52552=CARTESIAN_POINT('',(-4.91009411058386,-3.50523742971845E-5,3.73514056400927));
#52553=CARTESIAN_POINT('',(-4.91825,6.88216836313478E-12,-13.2351405640096));
#52554=CARTESIAN_POINT('Ctrl Pts',(-4.92432229863308,0.00284067633764233,
3.38985943599068));
#52555=CARTESIAN_POINT('Ctrl Pts',(-4.91423935983455,-1.46492632453142,
3.47327112758818));
#52556=CARTESIAN_POINT('Ctrl Pts',(-3.43786451232597,-4.58308142280596,
3.64947257776244));
#52557=CARTESIAN_POINT('Ctrl Pts',(1.86893072420659,-5.50838760091319,3.91846378651344));
#52558=CARTESIAN_POINT('Ctrl Pts',(5.64416974217652,-1.40662146125979,4.19683306224373));
#52559=CARTESIAN_POINT('Ctrl Pts',(4.23536382377072,3.98709534549548,4.47520233797398));
#52560=CARTESIAN_POINT('Ctrl Pts',(-1.06352998838801,5.71875335869428,4.75357161370427));
#52561=CARTESIAN_POINT('Ctrl Pts',(-4.50343455021169,2.91649876511814,4.97512397970982));
#52562=CARTESIAN_POINT('Ctrl Pts',(-4.91508920697772,0.639989911809819,
5.10388658713863));
#52563=CARTESIAN_POINT('Ctrl Pts',(-4.91175629129765,0.00283723643540366,
5.13985943599068));
#52564=CARTESIAN_POINT('Ctrl Pts',(-4.91009445539168,-3.50508923821491E-5,
3.73514056400927));
#52565=CARTESIAN_POINT('Ctrl Pts',(-4.91014639846267,-0.820522449457762,
3.78142514195625));
#52566=CARTESIAN_POINT('Ctrl Pts',(-4.32593467034914,-3.28614823268589,
3.92051767111895));
#52567=CARTESIAN_POINT('Ctrl Pts',(-0.421994265891336,-5.80186567765455,
4.15241815149737));
#52568=CARTESIAN_POINT('Ctrl Pts',(4.65287774260152,-3.49148295347327,4.43084200514448));
#52569=CARTESIAN_POINT('Ctrl Pts',(5.45265056950567,2.02690065589327,4.70926585879163));
#52570=CARTESIAN_POINT('Ctrl Pts',(1.24248690619172,5.68295264716619,4.98768971243874));
#52571=CARTESIAN_POINT('Ctrl Pts',(-3.72871428411602,4.22878800043754,5.24631461417798));
#52572=CARTESIAN_POINT('Ctrl Pts',(-4.9072377326162,1.28369869401846,5.41213156470147));
#52573=CARTESIAN_POINT('Ctrl Pts',(-4.91921671359201,-0.00447815882576173,
5.48514056400926));
#52574=CARTESIAN_POINT('Origin',(0.,0.,-13.2351405640096));
#52575=CARTESIAN_POINT('',(-4.92059821462187,-0.00426705290350537,1.63985943599068));
#52576=CARTESIAN_POINT('',(-4.91908762937381,0.00449034157284686,1.98514056400927));
#52577=CARTESIAN_POINT('',(-4.91825,6.88216836313478E-12,-13.2351405640096));
#52578=CARTESIAN_POINT('Ctrl Pts',(-4.92059821462188,-0.00426705290350625,
1.63985943599068));
#52579=CARTESIAN_POINT('Ctrl Pts',(-4.92337363329955,-0.307820924709806,
1.65707615088422));
#52580=CARTESIAN_POINT('Ctrl Pts',(-4.75936158429057,-2.24439195417028,
1.76708262435452));
#52581=CARTESIAN_POINT('Ctrl Pts',(-2.18939161896353,-5.38904447491294,
1.96987885640157));
#52582=CARTESIAN_POINT('Ctrl Pts',(3.34919840410121,-4.75584966790831,2.24824813213183));
#52583=CARTESIAN_POINT('Ctrl Pts',(5.81162385012341,0.245487756220548,2.5266174078621));
#52584=CARTESIAN_POINT('Ctrl Pts',(2.93620146934825,5.02135011179013,2.80498668359237));
#52585=CARTESIAN_POINT('Ctrl Pts',(-2.63605694837504,5.18521357117537,3.08335595932264));
#52586=CARTESIAN_POINT('Ctrl Pts',(-4.84294757931317,1.96452831576599,3.27831354345541));
#52587=CARTESIAN_POINT('Ctrl Pts',(-4.92545593438113,0.167863312618859,
3.38048136901143));
#52588=CARTESIAN_POINT('Ctrl Pts',(-4.92432229863308,0.00284067633764233,
3.38985943599068));
#52589=CARTESIAN_POINT('Ctrl Pts',(-4.91908762937381,0.00449034157284679,
1.98514056400927));
#52590=CARTESIAN_POINT('Ctrl Pts',(-4.90714654187502,-1.27955959344367,
2.05791076799533));
#52591=CARTESIAN_POINT('Ctrl Pts',(-3.73499225470963,-4.22053784471989,
2.2234889231971));
#52592=CARTESIAN_POINT('Ctrl Pts',(1.22786565484881,-5.68612965343156,2.48187502961459));
#52593=CARTESIAN_POINT('Ctrl Pts',(5.44741913497888,-2.040918731811,2.76029888326171));
#52594=CARTESIAN_POINT('Ctrl Pts',(4.6618428064117,3.47950372184003,3.03872273690884));
#52595=CARTESIAN_POINT('Ctrl Pts',(-0.407069872025434,5.80293189872846,
3.31714659055597));
#52596=CARTESIAN_POINT('Ctrl Pts',(-4.32149470970697,3.29468394743748,3.54928586625612));
#52597=CARTESIAN_POINT('Ctrl Pts',(-4.91004224433159,0.82468547587703,3.68861719074055));
#52598=CARTESIAN_POINT('Ctrl Pts',(-4.91009445539168,-3.50508923821491E-5,
3.73514056400927));
#52599=CARTESIAN_POINT('Origin',(0.,0.,-13.2351405640096));
#52600=CARTESIAN_POINT('',(-4.91020579987568,-0.000754363845140739,-0.110140564009323));
#52601=CARTESIAN_POINT('',(-4.92534843309394,-0.00204667003549375,0.235140564009264));
#52602=CARTESIAN_POINT('',(-4.91825,6.88216836313478E-12,-13.2351405640096));
#52603=CARTESIAN_POINT('Ctrl Pts',(-4.91020579987568,-0.00075436384514127,
-0.110140564009323));
#52604=CARTESIAN_POINT('Ctrl Pts',(-4.91126562658971,-0.777357875070976,
-0.0663290672429879));
#52605=CARTESIAN_POINT('Ctrl Pts',(-4.37107385466396,-3.19736087635733,
0.070272188100103));
#52606=CARTESIAN_POINT('Ctrl Pts',(-0.577472308506603,-5.78807064112712,
0.299663202019953));
#52607=CARTESIAN_POINT('Ctrl Pts',(4.5565129461533,-3.61571926251521,0.578032477750221));
#52608=CARTESIAN_POINT('Ctrl Pts',(5.50544194895434,1.87759020035487,0.856401753480491));
#52609=CARTESIAN_POINT('Ctrl Pts',(1.3977444217788,5.64637463733703,1.13477102921076));
#52610=CARTESIAN_POINT('Ctrl Pts',(-3.66029468083591,4.31674594493847,1.39592359004749));
#52611=CARTESIAN_POINT('Ctrl Pts',(-4.90841547022119,1.32818749234986,1.56428639230746));
#52612=CARTESIAN_POINT('Ctrl Pts',(-4.92059821462188,-0.00426705290350625,
1.63985943599068));
#52613=CARTESIAN_POINT('Ctrl Pts',(-4.92534843309394,-0.0020466700354939,
0.235140564009264));
#52614=CARTESIAN_POINT('Ctrl Pts',(-4.92594291426159,-0.115445370532234,
0.241588442818691));
#52615=CARTESIAN_POINT('Ctrl Pts',(-4.87090317476765,-1.86046814152323,
0.340844272843828));
#52616=CARTESIAN_POINT('Ctrl Pts',(-2.79755665155426,-5.10033344825063,
0.532908054084678));
#52617=CARTESIAN_POINT('Ctrl Pts',(2.7784711114303,-5.11075559823943,0.811331907731805));
#52618=CARTESIAN_POINT('Ctrl Pts',(5.80161865024956,-0.425376937628951,
1.08975576137894));
#52619=CARTESIAN_POINT('Ctrl Pts',(3.49419519287011,4.65084126326794,1.36817961502607));
#52620=CARTESIAN_POINT('Ctrl Pts',(-2.02372117571978,5.45383141515521,1.64660346867319));
#52621=CARTESIAN_POINT('Ctrl Pts',(-4.72602242607254,2.34563150667623,1.85225711833426));
#52622=CARTESIAN_POINT('Ctrl Pts',(-4.92237568519668,0.358061812020196,
1.96510281677962));
#52623=CARTESIAN_POINT('Ctrl Pts',(-4.91908762937381,0.00449034157284679,
1.98514056400927));
#52624=CARTESIAN_POINT('Origin',(0.,0.,-13.2351405640096));
#52625=CARTESIAN_POINT('',(-4.91782085325031,0.00454258279844846,-1.86014056400932));
#52626=CARTESIAN_POINT('',(-4.9128074373708,-0.00348491184884558,-1.51485943599074));
#52627=CARTESIAN_POINT('',(-4.91825,6.88216836313478E-12,-13.2351405640096));
#52628=CARTESIAN_POINT('Ctrl Pts',(-4.91782085325031,0.0045425827984481,
-1.86014056400932));
#52629=CARTESIAN_POINT('Ctrl Pts',(-4.9064064990659,-1.23861424073828,-1.78973428537019));
#52630=CARTESIAN_POINT('Ctrl Pts',(-3.79628753361988,-4.13829632682806,
-1.62653824815431));
#52631=CARTESIAN_POINT('Ctrl Pts',(1.08150986877385,-5.71538033878776,-1.37055245236166));
#52632=CARTESIAN_POINT('Ctrl Pts',(5.39248056989081,-2.18091478914392,-1.0921831766314));
#52633=CARTESIAN_POINT('Ctrl Pts',(4.75057726644074,3.35667270511782,-0.813813900901123));
#52634=CARTESIAN_POINT('Ctrl Pts',(-0.254626070074851,5.81123064231236,
-0.535444625170857));
#52635=CARTESIAN_POINT('Ctrl Pts',(-4.27501848124952,3.38203525187861,-0.30088684620692));
#52636=CARTESIAN_POINT('Ctrl Pts',(-4.90902098597739,0.867435332995769,
-0.159118825819744));
#52637=CARTESIAN_POINT('Ctrl Pts',(-4.91020579987568,-0.00075436384514127,
-0.110140564009323));
#52638=CARTESIAN_POINT('Ctrl Pts',(-4.9128074373708,-0.00348491184884551,
-1.51485943599074));
#52639=CARTESIAN_POINT('Ctrl Pts',(-4.91660369838043,-0.586491446993301,
-1.48192593114224));
#52640=CARTESIAN_POINT('Ctrl Pts',(-4.55054125897033,-2.80782229127452,
-1.35618447507802));
#52641=CARTESIAN_POINT('Ctrl Pts',(-1.24911288418635,-5.68149993443013,
-1.1376350677981));
#52642=CARTESIAN_POINT('Ctrl Pts',(4.10447898256108,-4.12225384754937,-0.859211214150975));
#52643=CARTESIAN_POINT('Ctrl Pts',(5.68684458676181,1.22455018188017,-0.580787360503842));
#52644=CARTESIAN_POINT('Ctrl Pts',(2.04409447042155,5.44622826349031,-0.302363506856717));
#52645=CARTESIAN_POINT('Ctrl Pts',(-3.34892978181137,4.68198894529797,-0.0303875320190087));
#52646=CARTESIAN_POINT('Ctrl Pts',(-4.9173862119977,1.516765993031,0.148780491602981));
#52647=CARTESIAN_POINT('Ctrl Pts',(-4.92534843309394,-0.0020466700354939,
0.235140564009264));
#52648=CARTESIAN_POINT('Origin',(0.,0.,-13.2351405640096));
#52649=CARTESIAN_POINT('',(-4.92591231680323,-0.0013684910865338,-3.61014056400932));
#52650=CARTESIAN_POINT('',(-4.91263526682963,0.00339649852347107,-3.26485943599074));
#52651=CARTESIAN_POINT('',(-4.91825,6.88216836313478E-12,-13.2351405640096));
#52652=CARTESIAN_POINT('Ctrl Pts',(-4.92591231680324,-0.00136849108653464,
-3.61014056400932));
#52653=CARTESIAN_POINT('Ctrl Pts',(-4.92618524681776,-0.0754100048993439,
-3.60592926207415));
#52654=CARTESIAN_POINT('Ctrl Pts',(-4.89107484137784,-1.78058131512418,
-3.50892820156222));
#52655=CARTESIAN_POINT('Ctrl Pts',(-2.92039509627066,-5.03055946195533,
-3.31913738247355));
#52656=CARTESIAN_POINT('Ctrl Pts',(2.65235109881223,-5.17689768424732,-3.04076810674327));
#52657=CARTESIAN_POINT('Ctrl Pts',(5.78897154557153,-0.568370014814376,
-2.76239883101301));
#52658=CARTESIAN_POINT('Ctrl Pts',(3.60854980134286,4.56219293151739,-2.48402955528274));
#52659=CARTESIAN_POINT('Ctrl Pts',(-1.8862450334912,5.50248268361132,-2.20566027955247));
#52660=CARTESIAN_POINT('Ctrl Pts',(-4.69698430404261,2.42929695424461,-1.99769728246133));
#52661=CARTESIAN_POINT('Ctrl Pts',(-4.9214496910873,0.399765514002954,-1.88252404394695));
#52662=CARTESIAN_POINT('Ctrl Pts',(-4.91782085325031,0.0045425827984481,
-1.86014056400932));
#52663=CARTESIAN_POINT('Ctrl Pts',(-4.91263526682963,0.003396498523471,
-3.26485943599074));
#52664=CARTESIAN_POINT('Ctrl Pts',(-4.90597445027353,-1.0485653240634,-3.20544030510316));
#52665=CARTESIAN_POINT('Ctrl Pts',(-4.05835413227311,-3.75340131497428,
-3.05321322299988));
#52666=CARTESIAN_POINT('Ctrl Pts',(0.400302865534793,-5.80340263407658,
-2.80817818968088));
#52667=CARTESIAN_POINT('Ctrl Pts',(5.09870148282997,-2.80052989457494,-2.52975433603375));
#52668=CARTESIAN_POINT('Ctrl Pts',(5.11237470052847,2.77549084296867,-2.25133048238662));
#52669=CARTESIAN_POINT('Ctrl Pts',(0.42875946485938,5.80136965084335,-1.97290662873949));
#52670=CARTESIAN_POINT('Ctrl Pts',(-4.04820116206155,3.76949085150405,-1.72741627994086));
#52671=CARTESIAN_POINT('Ctrl Pts',(-4.90590568102076,1.05644459400893,-1.57473388235795));
#52672=CARTESIAN_POINT('Ctrl Pts',(-4.9128074373708,-0.00348491184884551,
-1.51485943599074));
#52673=CARTESIAN_POINT('Origin',(0.,0.,-13.2351405640096));
#52674=CARTESIAN_POINT('',(-4.91367359665507,-0.00385188715628437,-5.36014056400933));
#52675=CARTESIAN_POINT('',(-4.92520873866597,0.00217779940761373,-5.01485943599074));
#52676=CARTESIAN_POINT('',(-4.91825,6.88216836313478E-12,-13.2351405640096));
#52677=CARTESIAN_POINT('Ctrl Pts',(-4.91367359665507,-0.0038518871562844,
-5.36014056400933));
#52678=CARTESIAN_POINT('Ctrl Pts',(-4.91764492376584,-0.548956137439361,
-5.32933448020136));
#52679=CARTESIAN_POINT('Ctrl Pts',(-4.58222637382267,-2.73119860279941,
-5.20573863781664));
#52680=CARTESIAN_POINT('Ctrl Pts',(-1.37997979498124,-5.65074267591175,
-4.98935303685515));
#52681=CARTESIAN_POINT('Ctrl Pts',(4.00703078514331,-4.21650789487217,-4.7109837611249));
#52682=CARTESIAN_POINT('Ctrl Pts',(5.71367268487829,1.09049576997227,-4.43261448539462));
#52683=CARTESIAN_POINT('Ctrl Pts',(2.17243253669944,5.39590335156548,-4.15424520966435));
#52684=CARTESIAN_POINT('Ctrl Pts',(-3.28037882473082,4.75513584668186,-3.88008723586925));
#52685=CARTESIAN_POINT('Ctrl Pts',(-4.92017164091969,1.5559843470402,-3.69871902065091));
#52686=CARTESIAN_POINT('Ctrl Pts',(-4.92591231680324,-0.00136849108653464,
-3.61014056400932));
#52687=CARTESIAN_POINT('Ctrl Pts',(-4.92520873866597,0.00217779940761347,
-5.01485943599074));
#52688=CARTESIAN_POINT('Ctrl Pts',(-4.91686006964921,-1.50874087785573,
-4.92895467906409));
#52689=CARTESIAN_POINT('Ctrl Pts',(-3.36282907081669,-4.6668321718968,-4.75024197092173));
#52690=CARTESIAN_POINT('Ctrl Pts',(2.01736012333282,-5.4561876061593,-4.47872131156366));
#52691=CARTESIAN_POINT('Ctrl Pts',(5.68077069634635,-1.25242520393326,-4.20029745791653));
#52692=CARTESIAN_POINT('Ctrl Pts',(4.12464623088233,4.10207481179193,-3.9218736042694));
#52693=CARTESIAN_POINT('Ctrl Pts',(-1.22123428830395,5.68755759612714,-3.64344975062227));
#52694=CARTESIAN_POINT('Ctrl Pts',(-4.54362355430201,2.82415249350275,-3.42444502786272));
#52695=CARTESIAN_POINT('Ctrl Pts',(-4.91637811536861,0.594515280668979,
-3.29824825631887));
#52696=CARTESIAN_POINT('Ctrl Pts',(-4.91263526682963,0.003396498523471,
-3.26485943599074));
#52697=CARTESIAN_POINT('Origin',(0.,0.,-13.2351405640096));
#52698=CARTESIAN_POINT('',(-4.91193228603272,0.00296404864912429,-7.11014056400932));
#52699=CARTESIAN_POINT('',(-4.91933390470069,-0.00446651128636566,-6.76485943599074));
#52700=CARTESIAN_POINT('',(-4.91825,6.88216836313478E-12,-13.2351405640096));
#52701=CARTESIAN_POINT('Ctrl Pts',(-4.91193228603272,0.00296404864912413,
-7.11014056400932));
#52702=CARTESIAN_POINT('Ctrl Pts',(-4.9063561374784,-1.01362454442101,-7.05273969832856));
#52703=CARTESIAN_POINT('Ctrl Pts',(-4.10272486587694,-3.68163039196913,
-6.90254907407105));
#52704=CARTESIAN_POINT('Ctrl Pts',(0.272909909778823,-5.81040739879541,
-6.65956869123677));
#52705=CARTESIAN_POINT('Ctrl Pts',(5.03514064798181,-2.9124777495484,-6.38119941550651));
#52706=CARTESIAN_POINT('Ctrl Pts',(5.17272309584991,2.66048658894571,-6.10283013977622));
#52707=CARTESIAN_POINT('Ctrl Pts',(0.559264958796863,5.78985906598745,-5.82446086404598));
#52708=CARTESIAN_POINT('Ctrl Pts',(-4.00046112440602,3.84356270012795,-5.57689767212365));
#52709=CARTESIAN_POINT('Ctrl Pts',(-4.90568305006145,1.09293031908751,-5.42212423877812));
#52710=CARTESIAN_POINT('Ctrl Pts',(-4.91367359665507,-0.0038518871562844,
-5.36014056400933));
#52711=CARTESIAN_POINT('Ctrl Pts',(-4.91933390470069,-0.00446651128636628,
-6.76485943599074));
#52712=CARTESIAN_POINT('Ctrl Pts',(-4.92254636011847,-0.349960418775078,
-6.74527700424072));
#52713=CARTESIAN_POINT('Ctrl Pts',(-4.73152296147135,-2.32934242081634,
-6.632886621275));
#52714=CARTESIAN_POINT('Ctrl Pts',(-2.05044135574297,-5.44383565780062,
-6.42768828709357));
#52715=CARTESIAN_POINT('Ctrl Pts',(3.47134289591715,-4.66792459610127,-6.14926443344644));
#52716=CARTESIAN_POINT('Ctrl Pts',(5.803635743461,0.3969206476142,-5.8708405797993));
#52717=CARTESIAN_POINT('Ctrl Pts',(2.80350181475234,5.09706699486434,-5.59241672615218));
#52718=CARTESIAN_POINT('Ctrl Pts',(-2.77250943461248,5.11399248292585,-5.31399287250505));
#52719=CARTESIAN_POINT('Ctrl Pts',(-4.86667316554333,1.87667755337039,-5.12147377578457));
#52720=CARTESIAN_POINT('Ctrl Pts',(-4.92587962682559,0.123593254817412,
-5.0217626302798));
#52721=CARTESIAN_POINT('Ctrl Pts',(-4.92520873866597,0.00217779940761347,
-5.01485943599074));
#52722=CARTESIAN_POINT('Origin',(0.,0.,-13.2351405640096));
#52723=CARTESIAN_POINT('',(-4.9240923050422,0.00237935796991909,-8.86014056400933));
#52724=CARTESIAN_POINT('',(-4.91001919821333,6.39834157820096E-5,-8.51485943599074));
#52725=CARTESIAN_POINT('',(-4.91825,6.88216836313478E-12,-13.2351405640096));
#52726=CARTESIAN_POINT('Ctrl Pts',(-4.9240923050422,0.00237935796991912,
-8.86014056400933));
#52727=CARTESIAN_POINT('Ctrl Pts',(-4.91423502458648,-1.47557821261336,
-8.77614491645577));
#52728=CARTESIAN_POINT('Ctrl Pts',(-3.42124592657607,-4.6021663877554,-8.59935951032545));
#52729=CARTESIAN_POINT('Ctrl Pts',(1.90395420368265,-5.4968079578387,-8.32978434561839));
#52730=CARTESIAN_POINT('Ctrl Pts',(5.65268654860171,-1.37094194360677,-8.05141506988812));
#52731=CARTESIAN_POINT('Ctrl Pts',(4.21031778233782,4.01357646538516,-7.77304579415784));
#52732=CARTESIAN_POINT('Ctrl Pts',(-1.09954047142025,5.71199305956496,-7.49467651842759));
#52733=CARTESIAN_POINT('Ctrl Pts',(-4.51265656995462,2.89554900635168,-7.27370810837807));
#52734=CARTESIAN_POINT('Ctrl Pts',(-4.91537010394053,0.629713217198827,
-7.14552945690532));
#52735=CARTESIAN_POINT('Ctrl Pts',(-4.91193228603272,0.00296404864912413,
-7.11014056400932));
#52736=CARTESIAN_POINT('Ctrl Pts',(-4.91001919821333,6.39834157814545E-5,
-8.51485943599074));
#52737=CARTESIAN_POINT('Ctrl Pts',(-4.9102107675652,-0.816682238869538,
-8.46879137820165));
#52738=CARTESIAN_POINT('Ctrl Pts',(-4.33010667838534,-3.27874551411531,
-8.32991536919685));
#52739=CARTESIAN_POINT('Ctrl Pts',(-0.435410493021885,-5.80062512701066,
-8.09823140897635));
#52740=CARTESIAN_POINT('Ctrl Pts',(4.64466218789312,-3.50245220498147,-7.81980755532921));
#52741=CARTESIAN_POINT('Ctrl Pts',(5.45739468419239,2.01424609607877,-7.54138370168209));
#52742=CARTESIAN_POINT('Ctrl Pts',(1.25572029180289,5.68000375627327,-7.26295984803495));
#52743=CARTESIAN_POINT('Ctrl Pts',(-3.72299945840702,4.23627988132658,-7.00411842613784));
#52744=CARTESIAN_POINT('Ctrl Pts',(-4.90732141719504,1.28745530777343,-6.83808495545644));
#52745=CARTESIAN_POINT('Ctrl Pts',(-4.91933390470069,-0.00446651128636628,
-6.76485943599074));
#52746=CARTESIAN_POINT('Origin',(0.,0.,-9.5));
#52747=CARTESIAN_POINT('',(-3.54932990775846,-3.52168385944726,-10.));
#52748=CARTESIAN_POINT('Ctrl Pts',(3.34446487542469,-4.86859341898352,-9.08325));
#52749=CARTESIAN_POINT('Ctrl Pts',(3.19879863164306,-4.94736391093165,-9.10154508180626));
#52750=CARTESIAN_POINT('Ctrl Pts',(3.05033436817195,-5.02004566253132,-9.11988472965185));
#52751=CARTESIAN_POINT('Ctrl Pts',(2.89941768276307,-5.08638119286217,-9.13828856187511));
#52752=CARTESIAN_POINT('Ctrl Pts',(2.75120930712827,-5.15152628381466,-9.15636212393271));
#52753=CARTESIAN_POINT('Ctrl Pts',(2.60063505538134,-5.21055103333368,-9.17449758736774));
#52754=CARTESIAN_POINT('Ctrl Pts',(2.44801186022486,-5.26316298026786,-9.19271353316328));
#52755=CARTESIAN_POINT('Ctrl Pts',(2.29775466947289,-5.31495932313839,-9.21064709063678));
#52756=CARTESIAN_POINT('Ctrl Pts',(2.14551098203089,-5.36054028317659,-9.2286586544954));
#52757=CARTESIAN_POINT('Ctrl Pts',(1.99158237653721,-5.39957715606078,-9.24676595490747));
#52758=CARTESIAN_POINT('Ctrl Pts',(1.85900718724118,-5.43319872234177,-9.26236135884212));
#52759=CARTESIAN_POINT('Ctrl Pts',(1.72518191031146,-5.46196520161207,-9.2780277799907));
#52760=CARTESIAN_POINT('Ctrl Pts',(1.59030358846426,-5.48563510874125,-9.29377654605015));
#52761=CARTESIAN_POINT('Ctrl Pts',(1.53227521801134,-5.49581855498129,-9.30055209914541));
#52762=CARTESIAN_POINT('Ctrl Pts',(1.47405201016708,-5.50505826954835,-9.30734289393353));
#52763=CARTESIAN_POINT('Ctrl Pts',(1.41565008458091,-5.51333327452099,-9.31414983247631));
#52764=CARTESIAN_POINT('Ctrl Pts',(1.39022440435432,-5.5169358548845,-9.31711328001633));
#52765=CARTESIAN_POINT('Ctrl Pts',(1.36476184378213,-5.52035588011081,-9.32008013785663));
#52766=CARTESIAN_POINT('Ctrl Pts',(1.33928832028401,-5.52358866726458,-9.32304761925695));
#52767=CARTESIAN_POINT('Ctrl Pts',(1.28727163537636,-5.53018998689608,-9.32910718714441));
#52768=CARTESIAN_POINT('Ctrl Pts',(1.23518854185695,-5.53601374978223,-9.33517176846418));
#52769=CARTESIAN_POINT('Ctrl Pts',(1.18304992365009,-5.54105054431051,-9.34124208925133));
#52770=CARTESIAN_POINT('Ctrl Pts',(1.02673277346924,-5.55615139266026,-9.35944155979285));
#52771=CARTESIAN_POINT('Ctrl Pts',(0.869916237775008,-5.56418242497692,
-9.37769262036853));
#52772=CARTESIAN_POINT('Ctrl Pts',(0.713056273219087,-5.56532307499083,
-9.39601483683802));
#52773=CARTESIAN_POINT('Ctrl Pts',(0.554631282752025,-5.5664751055175,-9.41451985803785));
#52774=CARTESIAN_POINT('Ctrl Pts',(0.396161147779864,-5.56059828159109,
-9.43309746209029));
#52775=CARTESIAN_POINT('Ctrl Pts',(0.238126550129667,-5.54782555539949,
-9.45176780635592));
#52776=CARTESIAN_POINT('Ctrl Pts',(0.0814929446544512,-5.53516606067564,
-9.47027263619237));
#52777=CARTESIAN_POINT('Ctrl Pts',(-0.0747135674656943,-5.5157319593914,
-9.48886856922834));
#52778=CARTESIAN_POINT('Ctrl Pts',(-0.230002369134159,-5.48960759431231,
-9.50757523147196));
#52779=CARTESIAN_POINT('Ctrl Pts',(-0.341080017822252,-5.47092090850318,
-9.52095605503746));
#52780=CARTESIAN_POINT('Ctrl Pts',(-0.451687676746772,-5.4488102013679,
-9.53439353321513));
#52781=CARTESIAN_POINT('Ctrl Pts',(-0.561635393178398,-5.42329377189995,
-9.54789484876889));
#52782=CARTESIAN_POINT('Ctrl Pts',(-0.603914210286864,-5.41348179499175,
-9.55308658598315));
#52783=CARTESIAN_POINT('Ctrl Pts',(-0.64609533818728,-5.40316611823237,
-9.55828776268145));
#52784=CARTESIAN_POINT('Ctrl Pts',(-0.688167556291023,-5.39234740569837,
-9.56349878727855));
#52785=CARTESIAN_POINT('Ctrl Pts',(-0.712858909949692,-5.38599811703834,
-9.5665570346696));
#52786=CARTESIAN_POINT('Ctrl Pts',(-0.737512747340636,-5.37947556474227,
-9.56961867395688));
#52787=CARTESIAN_POINT('Ctrl Pts',(-0.762126759085168,-5.37277985131085,
-9.57268378769665));
#52788=CARTESIAN_POINT('Ctrl Pts',(-0.781035172201083,-5.36763622348695,
-9.57503839926669));
#52789=CARTESIAN_POINT('Ctrl Pts',(-0.799910762238151,-5.36239293904086,
-9.57739390086569));
#52790=CARTESIAN_POINT('Ctrl Pts',(-0.818751399856817,-5.35705067432398,
-9.57975018027239));
#52791=CARTESIAN_POINT('Ctrl Pts',(-0.966624994112708,-5.31512110160247,
-9.59824379561558));
#52792=CARTESIAN_POINT('Ctrl Pts',(-1.11237269054818,-5.26709116156679,
-9.61678848533419));
#52793=CARTESIAN_POINT('Ctrl Pts',(-1.2555573640261,-5.21309665032415,-9.635405210757));
#52794=CARTESIAN_POINT('Ctrl Pts',(-1.34560868000601,-5.17913856895281,
-9.64711359115024));
#52795=CARTESIAN_POINT('Ctrl Pts',(-1.43464583115756,-5.14282031676834,
-9.65885046432624));
#52796=CARTESIAN_POINT('Ctrl Pts',(-1.5225544255541,-5.10416673508712,-9.67062104462566));
#52797=CARTESIAN_POINT('Ctrl Pts',(-1.66238523492523,-5.04268285346346,
-9.68934378477791));
#52798=CARTESIAN_POINT('Ctrl Pts',(-1.79936268643465,-4.97529188425519,
-9.70815180838046));
#52799=CARTESIAN_POINT('Ctrl Pts',(-1.93314075803419,-4.90216296398429,
-9.72706610067654));
#52800=CARTESIAN_POINT('Ctrl Pts',(-2.06568174395399,-4.82971028862378,
-9.74580548687731));
#52801=CARTESIAN_POINT('Ctrl Pts',(-2.19508269636191,-4.75162475819703,
-9.76464918546239));
#52802=CARTESIAN_POINT('Ctrl Pts',(-2.32096600124785,-4.66804080983962,
-9.78361760487156));
#52803=CARTESIAN_POINT('Ctrl Pts',(-2.37965096368007,-4.62907519105692,
-9.79246040560224));
#52804=CARTESIAN_POINT('Ctrl Pts',(-2.4375708125932,-4.58891422837344,-9.80133031176665));
#52805=CARTESIAN_POINT('Ctrl Pts',(-2.49468378132543,-4.547569770274,-9.810229391057));
#52806=CARTESIAN_POINT('Ctrl Pts',(-2.52796808704415,-4.52347503988782,
-9.81541559801297));
#52807=CARTESIAN_POINT('Ctrl Pts',(-2.56097830625555,-4.49897833648104,
-9.8206117131173));
#52808=CARTESIAN_POINT('Ctrl Pts',(-2.59370579156265,-4.47408185876841,
-9.82581814563082));
#52809=CARTESIAN_POINT('Ctrl Pts',(-2.60830979622556,-4.4629722891454,-9.82814141501712));
#52810=CARTESIAN_POINT('Ctrl Pts',(-2.62285735082004,-4.45178316892005,
-9.83046672058383));
#52811=CARTESIAN_POINT('Ctrl Pts',(-2.63733749771883,-4.44052277762685,
-9.83279244866301));
#52812=CARTESIAN_POINT('Ctrl Pts',(-2.75344399409984,-4.35023332199701,
-9.85144088784646));
#52813=CARTESIAN_POINT('Ctrl Pts',(-2.86539772416489,-4.25522984404488,
-9.87014472889391));
#52814=CARTESIAN_POINT('Ctrl Pts',(-2.97290571973465,-4.15568845804594,
-9.88892585516935));
#52815=CARTESIAN_POINT('Ctrl Pts',(-3.07913398797304,-4.05733196840369,
-9.9074834192764));
#52816=CARTESIAN_POINT('Ctrl Pts',(-3.18102210231045,-3.95454441586392,
-9.92611643962443));
#52817=CARTESIAN_POINT('Ctrl Pts',(-3.2782462026002,-3.84746691787586,-9.94484602737331));
#52818=CARTESIAN_POINT('Ctrl Pts',(-3.37316798191902,-3.74292507481694,
-9.96313208802836));
#52819=CARTESIAN_POINT('Ctrl Pts',(-3.46364424021495,-3.63429354697869,
-9.98151019669632));
#52820=CARTESIAN_POINT('Ctrl Pts',(-3.54932990775845,-3.52168385944727,
-10.));
#52821=CARTESIAN_POINT('',(3.54932990775696,-3.52168385944877,-10.));
#52822=CARTESIAN_POINT('Ctrl Pts',(3.54751238410166,-3.52143928316711,-10.));
#52823=CARTESIAN_POINT('Ctrl Pts',(3.65508312862553,-3.41996290417742,-9.99476917353171));
#52824=CARTESIAN_POINT('Ctrl Pts',(3.75814035868601,-3.31372395112702,-9.98954665627179));
#52825=CARTESIAN_POINT('Ctrl Pts',(3.85646778381177,-3.20303931222073,-9.98432713957975));
#52826=CARTESIAN_POINT('Ctrl Pts',(3.923641246713,-3.12742388269231,-9.98076136929311));
#52827=CARTESIAN_POINT('Ctrl Pts',(3.98860659175575,-3.04973273944966,-9.97719699939839));
#52828=CARTESIAN_POINT('Ctrl Pts',(4.05128444657531,-2.97005757844254,-9.97363233730264));
#52829=CARTESIAN_POINT('Ctrl Pts',(4.07561399842648,-2.93913021236477,-9.97224864873289));
#52830=CARTESIAN_POINT('Ctrl Pts',(4.099598786423,-2.90790383263907,-9.97086491613587));
#52831=CARTESIAN_POINT('Ctrl Pts',(4.12323378449639,-2.8763835412882,-9.96948104051677));
#52832=CARTESIAN_POINT('Ctrl Pts',(4.13398915280514,-2.86203988271776,-9.96885129255018));
#52833=CARTESIAN_POINT('Ctrl Pts',(4.14467115873595,-2.84763653652582,-9.96822156758605));
#52834=CARTESIAN_POINT('Ctrl Pts',(4.15527382809579,-2.83318170099535,-9.96759218868572));
#52835=CARTESIAN_POINT('Ctrl Pts',(4.24378373503389,-2.71251433844854,-9.96233820348577));
#52836=CARTESIAN_POINT('Ctrl Pts',(4.32687797709647,-2.58811568558574,-9.95710189140309));
#52837=CARTESIAN_POINT('Ctrl Pts',(4.4043694477894,-2.46033758996999,-9.95187801813126));
#52838=CARTESIAN_POINT('Ctrl Pts',(4.45485165672787,-2.37709590591168,-9.94847489957359));
#52839=CARTESIAN_POINT('Ctrl Pts',(4.50295544391612,-2.29241912223262,-9.94507705996846));
#52840=CARTESIAN_POINT('Ctrl Pts',(4.54862070762841,-2.20639609047384,-9.94168305216942));
#52841=CARTESIAN_POINT('Ctrl Pts',(4.61880161012226,-2.07419113832192,-9.9364669533003));
#52842=CARTESIAN_POINT('Ctrl Pts',(4.6832252135784,-1.93880757714367,-9.93125990486675));
#52843=CARTESIAN_POINT('Ctrl Pts',(4.74171890553884,-1.80071137001634,-9.92605665382018));
#52844=CARTESIAN_POINT('Ctrl Pts',(4.77596862098491,-1.71985212451872,-9.92301000277514));
#52845=CARTESIAN_POINT('Ctrl Pts',(4.80818447948761,-1.63806232182356,-9.91996465363939));
#52846=CARTESIAN_POINT('Ctrl Pts',(4.83832430884422,-1.55543201942794,-9.91691955189195));
#52847=CARTESIAN_POINT('Ctrl Pts',(4.8532086808827,-1.51462554544438,-9.91541574685153));
#52848=CARTESIAN_POINT('Ctrl Pts',(4.86758665820026,-1.4736140570085,-9.91391200214463));
#52849=CARTESIAN_POINT('Ctrl Pts',(4.88145262570607,-1.43240824637402,-9.91240819076519));
#52850=CARTESIAN_POINT('Ctrl Pts',(4.89270606139725,-1.39896615588277,-9.9111877173548));
#52851=CARTESIAN_POINT('Ctrl Pts',(4.9036222434836,-1.36539606845859,-9.90996720002901));
#52852=CARTESIAN_POINT('Ctrl Pts',(4.91419799178983,-1.33170366495726,-9.90874657089416));
#52853=CARTESIAN_POINT('Ctrl Pts',(4.92037675597896,-1.31201925018379,-9.90803343179815));
#52854=CARTESIAN_POINT('Ctrl Pts',(4.92643945384592,-1.29229242931547,-9.90732023154963));
#52855=CARTESIAN_POINT('Ctrl Pts',(4.93238098424579,-1.27253967687844,-9.90660750838836));
#52856=CARTESIAN_POINT('Ctrl Pts',(4.97609052146227,-1.12722633003541,-9.90136428022223));
#52857=CARTESIAN_POINT('Ctrl Pts',(5.01330854498342,-0.980316288849063,
-9.89613976777481));
#52858=CARTESIAN_POINT('Ctrl Pts',(5.04390188651618,-0.832299452109599,
-9.8909287871518));
#52859=CARTESIAN_POINT('Ctrl Pts',(5.07450394234213,-0.684240453839277,
-9.88571632221846));
#52860=CARTESIAN_POINT('Ctrl Pts',(5.09847787962514,-0.535073232147375,
-9.88051739681951));
#52861=CARTESIAN_POINT('Ctrl Pts',(5.11564390371681,-0.385264822007308,
-9.8753268226296));
#52862=CARTESIAN_POINT('Ctrl Pts',(5.13254133760872,-0.237800406643843,
-9.87021746336465));
#52863=CARTESIAN_POINT('Ctrl Pts',(5.14284243623783,-0.089713929354489,
-9.86511619601691));
#52864=CARTESIAN_POINT('Ctrl Pts',(5.14632684128669,0.0585599414038308,
-9.86001807200956));
#52865=CARTESIAN_POINT('Ctrl Pts',(5.14782497925894,0.122311059015022,-9.85782610722489));
#52866=CARTESIAN_POINT('Ctrl Pts',(5.1480623354105,0.186096887079666,-9.85563472352268));
#52867=CARTESIAN_POINT('Ctrl Pts',(5.14701840430152,0.249882961654822,-9.85344352757947));
#52868=CARTESIAN_POINT('Ctrl Pts',(5.14523776540626,0.358683211391727,-9.84970599289919));
#52869=CARTESIAN_POINT('Ctrl Pts',(5.13973005118594,0.467484324210803,-9.84596900449073));
#52870=CARTESIAN_POINT('Ctrl Pts',(5.13058176480017,0.576148493099822,-9.84223061043461));
#52871=CARTESIAN_POINT('Ctrl Pts',(5.12862737772094,0.599362878690334,-9.84143196151477));
#52872=CARTESIAN_POINT('Ctrl Pts',(5.12650678498253,0.622571005372613,-9.84063324844177));
#52873=CARTESIAN_POINT('Ctrl Pts',(5.12422074716705,0.645771512820038,-9.83983445218403));
#52874=CARTESIAN_POINT('Ctrl Pts',(5.12234618145826,0.664796078115013,-9.83917943411612));
#52875=CARTESIAN_POINT('Ctrl Pts',(5.12036039172749,0.683814766160387,-9.83852438594634));
#52876=CARTESIAN_POINT('Ctrl Pts',(5.11826539452591,0.702813831563803,-9.83786974525181));
#52877=CARTESIAN_POINT('Ctrl Pts',(5.10210352212495,0.849382271156973,-9.83281951446132));
#52878=CARTESIAN_POINT('Ctrl Pts',(5.07942731567127,0.994985322764188,-9.82778654540807));
#52879=CARTESIAN_POINT('Ctrl Pts',(5.05055882614455,1.13928743301165,-9.82276620697614));
#52880=CARTESIAN_POINT('Ctrl Pts',(5.02102945684531,1.28689301868713,-9.81763093907698));
#52881=CARTESIAN_POINT('Ctrl Pts',(4.98502090518309,1.43313803605949,-9.81250888671849));
#52882=CARTESIAN_POINT('Ctrl Pts',(4.94282336643821,1.57766552599623,-9.80739509339072));
#52883=CARTESIAN_POINT('Ctrl Pts',(4.89995783591708,1.72448090232613,-9.80220034814039));
#52884=CARTESIAN_POINT('Ctrl Pts',(4.85070560322117,1.86952465184268,-9.7970141254732));
#52885=CARTESIAN_POINT('Ctrl Pts',(4.79531809543285,2.01241464363871,-9.79183122974702));
#52886=CARTESIAN_POINT('Ctrl Pts',(4.74368240911756,2.14562559839358,-9.78699941137121));
#52887=CARTESIAN_POINT('Ctrl Pts',(4.68671374369661,2.27696508058455,-9.78217048448318));
#52888=CARTESIAN_POINT('Ctrl Pts',(4.62457829497681,2.4061090829116,-9.77734023935897));
#52889=CARTESIAN_POINT('Ctrl Pts',(4.60514189625996,2.4465062213058,-9.77582930522928));
#52890=CARTESIAN_POINT('Ctrl Pts',(4.58519968636458,2.48668840236422,-9.77431824211259));
#52891=CARTESIAN_POINT('Ctrl Pts',(4.56475608548958,2.52664530516031,-9.77280692115941));
#52892=CARTESIAN_POINT('Ctrl Pts',(4.55525175077551,2.54522147384181,-9.77210430031061));
#52893=CARTESIAN_POINT('Ctrl Pts',(4.5456390427194,2.56374894853136,-9.77140162373386));
#52894=CARTESIAN_POINT('Ctrl Pts',(4.53591838330546,2.58222667542352,-9.77069887848196));
#52895=CARTESIAN_POINT('Ctrl Pts',(4.52641793441604,2.6002858103501,-9.77001205312747));
#52896=CARTESIAN_POINT('Ctrl Pts',(4.51681805327452,2.6182903808933,-9.76932542975162));
#52897=CARTESIAN_POINT('Ctrl Pts',(4.50712198593273,2.63623477492454,-9.76863917841065));
#52898=CARTESIAN_POINT('Ctrl Pts',(4.43327641607358,2.77289987390772,-9.76341266547974));
#52899=CARTESIAN_POINT('Ctrl Pts',(4.35380963597557,2.90616348574592,-9.75820438137484));
#52900=CARTESIAN_POINT('Ctrl Pts',(4.2690165533173,3.03565215533473,-9.75300919073388));
#52901=CARTESIAN_POINT('Ctrl Pts',(4.18369488725524,3.16594803182743,-9.74778161429604));
#52902=CARTESIAN_POINT('Ctrl Pts',(4.09297996159635,3.29242249771891,-9.74256729507512));
#52903=CARTESIAN_POINT('Ctrl Pts',(3.99712250040057,3.41467782938133,-9.73736100107061));
#52904=CARTESIAN_POINT('Ctrl Pts',(3.90251511176284,3.53533883512192,-9.73222260209674));
#52905=CARTESIAN_POINT('Ctrl Pts',(3.80289797907067,3.65189067996929,-9.72709202039119));
#52906=CARTESIAN_POINT('Ctrl Pts',(3.69847007959931,3.76392400377687,-9.7219642259865));
#52907=CARTESIAN_POINT('Ctrl Pts',(3.62190098220249,3.84606958484991,-9.71820440134969));
#52908=CARTESIAN_POINT('Ctrl Pts',(3.54274464208819,3.92578541816275,-9.71444607521657));
#52909=CARTESIAN_POINT('Ctrl Pts',(3.46106691159086,4.0028976587042,-9.71068726479984));
#52910=CARTESIAN_POINT('Ctrl Pts',(3.42356702701269,4.03830143525703,-9.70896151953342));
#52911=CARTESIAN_POINT('Ctrl Pts',(3.38553551647611,4.07315623363686,-9.70723567218425));
#52912=CARTESIAN_POINT('Ctrl Pts',(3.3469780762519,4.10744433178595,-9.7055095308612));
#52913=CARTESIAN_POINT('Ctrl Pts',(3.32402527509264,4.12785564266054,-9.70448197876411));
#52914=CARTESIAN_POINT('Ctrl Pts',(3.30088609320679,4.14806612156554,-9.70345432249197));
#52915=CARTESIAN_POINT('Ctrl Pts',(3.27756166527489,4.168071925129,-9.70242652156505));
#52916=CARTESIAN_POINT('Ctrl Pts',(3.26270593229633,4.18081396864784,-9.70177189731574));
#52917=CARTESIAN_POINT('Ctrl Pts',(3.24777526204805,4.19347273003535,-9.70111722521979));
#52918=CARTESIAN_POINT('Ctrl Pts',(3.23278066815151,4.20603842872606,-9.70046295819114));
#52919=CARTESIAN_POINT('Ctrl Pts',(3.11335631773141,4.30611785829023,-9.69525205248491));
#52920=CARTESIAN_POINT('Ctrl Pts',(2.98971082178213,4.40044304867354,-9.69005933831205));
#52921=CARTESIAN_POINT('Ctrl Pts',(2.86208820640147,4.48862411075741,-9.68487973117774));
#52922=CARTESIAN_POINT('Ctrl Pts',(2.7970006164004,4.53359649122191,-9.68223812926009));
#52923=CARTESIAN_POINT('Ctrl Pts',(2.73087789159375,4.57697031785747,-9.67959993648905));
#52924=CARTESIAN_POINT('Ctrl Pts',(2.66374840647643,4.61869047738687,-9.67696447839955));
#52925=CARTESIAN_POINT('Ctrl Pts',(2.53534702353607,4.69849037709868,-9.67192352712782));
#52926=CARTESIAN_POINT('Ctrl Pts',(2.40326422843609,4.77224301178556,-9.66689258091221));
#52927=CARTESIAN_POINT('Ctrl Pts',(2.26796505031953,4.84000307398862,-9.66186691989815));
#52928=CARTESIAN_POINT('Ctrl Pts',(2.13014247260833,4.90902689637023,-9.65674752770892));
#52929=CARTESIAN_POINT('Ctrl Pts',(1.98898175619273,4.97183275027531,-9.65163361970313));
#52930=CARTESIAN_POINT('Ctrl Pts',(1.84494702971633,5.0284315690857,-9.64652020698713));
#52931=CARTESIAN_POINT('Ctrl Pts',(1.7580990880663,5.06255869268814,-9.64343699656937));
#52932=CARTESIAN_POINT('Ctrl Pts',(1.67020576767861,5.09442822583008,-9.6403539662227));
#52933=CARTESIAN_POINT('Ctrl Pts',(1.58136572634967,5.12403406159239,-9.63727002228997));
#52934=CARTESIAN_POINT('Ctrl Pts',(1.55287794159396,5.13352758122716,-9.63628111312648));
#52935=CARTESIAN_POINT('Ctrl Pts',(1.52429279737253,5.14278828576354,-9.63529211002327));
#52936=CARTESIAN_POINT('Ctrl Pts',(1.49561351608857,5.15181583211708,-9.63430297691988));
#52937=CARTESIAN_POINT('Ctrl Pts',(1.47064629134486,5.1596749125613,-9.63344187066519));
#52938=CARTESIAN_POINT('Ctrl Pts',(1.44560369716888,5.16735840950949,-9.63258052873048));
#52939=CARTESIAN_POINT('Ctrl Pts',(1.42051478324143,5.17485823755497,-9.63171984848409));
#52940=CARTESIAN_POINT('Ctrl Pts',(1.27281033665945,5.21901152191478,-9.62665281768929));
#52941=CARTESIAN_POINT('Ctrl Pts',(1.12333461568641,5.25685764911356,-9.62160289217849));
#52942=CARTESIAN_POINT('Ctrl Pts',(0.972565836059491,5.28847001595391,-9.61656539809095));
#52943=CARTESIAN_POINT('Ctrl Pts',(0.817722274810746,5.32093676054902,-9.61139175719385));
#52944=CARTESIAN_POINT('Ctrl Pts',(0.661514135419789,5.34682850300569,-9.60623122876099));
#52945=CARTESIAN_POINT('Ctrl Pts',(0.504434245978927,5.366176087194,-9.60107874964041));
#52946=CARTESIAN_POINT('Ctrl Pts',(0.346736308694608,5.38559979654847,-9.5959059975325));
#52947=CARTESIAN_POINT('Ctrl Pts',(0.188158926194008,5.39842785415446,-9.59074135820327));
#52948=CARTESIAN_POINT('Ctrl Pts',(0.0291872541970131,5.40464051199876,
-9.58557970850075));
#52949=CARTESIAN_POINT('Ctrl Pts',(-0.0807427828887296,5.40893660889857,
-9.58201039117462));
#52950=CARTESIAN_POINT('Ctrl Pts',(-0.190861650141258,5.41006828149116,
-9.57844250343431));
#52951=CARTESIAN_POINT('Ctrl Pts',(-0.30100952587624,5.40801441897329,-9.57487435122625));
#52952=CARTESIAN_POINT('Ctrl Pts',(-0.397441723071222,5.40621630462915,
-9.57175050743849));
#52953=CARTESIAN_POINT('Ctrl Pts',(-0.493896213953238,5.40197642027737,
-9.56862646094568));
#52954=CARTESIAN_POINT('Ctrl Pts',(-0.590264680648783,5.39527294553146,
-9.56550107499785));
#52955=CARTESIAN_POINT('Ctrl Pts',(-0.615978987046301,5.39348423591041,
-9.56466711826253));
#52956=CARTESIAN_POINT('Ctrl Pts',(-0.641690795569914,5.39151970479417,
-9.56383294798454));
#52957=CARTESIAN_POINT('Ctrl Pts',(-0.667371531977541,5.3893812707165,-9.56299940297276));
#52958=CARTESIAN_POINT('Ctrl Pts',(-0.829270594756447,5.37589994107338,
-9.5577444852769));
#52959=CARTESIAN_POINT('Ctrl Pts',(-0.990135744404899,5.35549932104634,
-9.55250787197851));
#52960=CARTESIAN_POINT('Ctrl Pts',(-1.14945847310104,5.32820571619838,-9.54728435100756));
#52961=CARTESIAN_POINT('Ctrl Pts',(-1.30657774605491,5.30128958574357,-9.54213307206618));
#52962=CARTESIAN_POINT('Ctrl Pts',(-1.46219782294251,5.26766974957298,-9.536994525819));
#52963=CARTESIAN_POINT('Ctrl Pts',(-1.61583449285355,5.22731999533615,-9.53186371346998));
#52964=CARTESIAN_POINT('Ctrl Pts',(-1.77270308583972,5.1861214378685,-9.52662496861479));
#52965=CARTESIAN_POINT('Ctrl Pts',(-1.92750487728277,5.13790710889339,-9.52139428646294));
#52966=CARTESIAN_POINT('Ctrl Pts',(-2.07971463146265,5.08259314212322,-9.51616634606952));
#52967=CARTESIAN_POINT('Ctrl Pts',(-2.22307874051765,5.03049373754149,-9.51124222658235));
#52968=CARTESIAN_POINT('Ctrl Pts',(-2.36414389577942,4.97209550169895,-9.50632053943975));
#52969=CARTESIAN_POINT('Ctrl Pts',(-2.50245210566454,4.90728144565132,-9.50139683850687));
#52970=CARTESIAN_POINT('Ctrl Pts',(-2.51098579900357,4.90328238240823,-9.50109304342566));
#52971=CARTESIAN_POINT('Ctrl Pts',(-2.5195089888609,4.89925887980383,-9.50078924067803));
#52972=CARTESIAN_POINT('Ctrl Pts',(-2.52802156438008,4.89521090457976,-9.50048542921963));
#52973=CARTESIAN_POINT('Ctrl Pts',(-2.57132234240826,4.87462013551746,-9.49894003646592));
#52974=CARTESIAN_POINT('Ctrl Pts',(-2.61434850193029,4.85339618259019,-9.49739441832657));
#52975=CARTESIAN_POINT('Ctrl Pts',(-2.65709309431552,4.83154930784417,-9.49584843734864));
#52976=CARTESIAN_POINT('Ctrl Pts',(-2.6760615610272,4.82185447410616,-9.49516238825845));
#52977=CARTESIAN_POINT('Ctrl Pts',(-2.69496807459095,4.81204025654554,-9.4944765024017));
#52978=CARTESIAN_POINT('Ctrl Pts',(-2.71380592953414,4.80211114530722,-9.49379099483116));
#52979=CARTESIAN_POINT('Ctrl Pts',(-2.84926842013991,4.73071118273708,-9.48886152897028));
#52980=CARTESIAN_POINT('Ctrl Pts',(-2.98128317523458,4.65332256785403,-9.48394795579456));
#52981=CARTESIAN_POINT('Ctrl Pts',(-3.10968019447802,4.57039549293769,-9.47904597111631));
#52982=CARTESIAN_POINT('Ctrl Pts',(-3.24115785230975,4.48547874296108,-9.47402637277968));
#52983=CARTESIAN_POINT('Ctrl Pts',(-3.36884257048857,4.39475421907267,-9.4690189256989));
#52984=CARTESIAN_POINT('Ctrl Pts',(-3.49253305551556,4.2986536163194,-9.46401900838148));
#52985=CARTESIAN_POINT('Ctrl Pts',(-3.61846974796904,4.20080783577377,-9.45892829304183));
#52986=CARTESIAN_POINT('Ctrl Pts',(-3.74026635650893,4.09738848130592,-9.45384538342829));
#52987=CARTESIAN_POINT('Ctrl Pts',(-3.85768343310466,3.98880461048543,-9.44876540167088));
#52988=CARTESIAN_POINT('Ctrl Pts',(-3.97901726934032,3.87659863515419,-9.44351596357802));
#52989=CARTESIAN_POINT('Ctrl Pts',(-4.09567526725608,3.7588773848341,-9.43826965193208));
#52990=CARTESIAN_POINT('Ctrl Pts',(-4.20735462904591,3.63604990000422,-9.43302108425564));
#52991=CARTESIAN_POINT('Ctrl Pts',(-4.23973848882022,3.600433399503,-9.43149914791103));
#52992=CARTESIAN_POINT('Ctrl Pts',(-4.27170344532821,3.56438730989727,-9.42997702187123));
#52993=CARTESIAN_POINT('Ctrl Pts',(-4.30324139350661,3.52792105998702,-9.42845457490134));
#52994=CARTESIAN_POINT('Ctrl Pts',(-4.31633871211275,3.51277707881412,-9.42782232156284));
#52995=CARTESIAN_POINT('Ctrl Pts',(-4.32936416131798,3.49755852787676,-9.42718992591442));
#52996=CARTESIAN_POINT('Ctrl Pts',(-4.34231115280572,3.48227315974663,-9.42655767144258));
#52997=CARTESIAN_POINT('Ctrl Pts',(-4.44720672844005,3.35843222802825,-9.42143519207479));
#52998=CARTESIAN_POINT('Ctrl Pts',(-4.54678702961592,3.23041013060237,-9.4163302350616));
#52999=CARTESIAN_POINT('Ctrl Pts',(-4.64084015186826,3.09865692394184,-9.41123798111106));
#53000=CARTESIAN_POINT('Ctrl Pts',(-4.7358219581732,2.96560278118293,-9.40609544605424));
#53001=CARTESIAN_POINT('Ctrl Pts',(-4.82516742957498,2.82874288782327,-9.4009658661596));
#53002=CARTESIAN_POINT('Ctrl Pts',(-4.90862468068945,2.6884992822051,-9.39584427796333));
#53003=CARTESIAN_POINT('Ctrl Pts',(-4.99196861908384,2.54844609005268,-9.39072964351981));
#53004=CARTESIAN_POINT('Ctrl Pts',(-5.06944080169255,2.4050177011056,-9.3856229790882));
#53005=CARTESIAN_POINT('Ctrl Pts',(-5.14074940665675,2.25860287614353,-9.38051934139442));
#53006=CARTESIAN_POINT('Ctrl Pts',(-5.20678494943055,2.12301499805566,-9.37579310273924));
#53007=CARTESIAN_POINT('Ctrl Pts',(-5.26753466845846,1.98486530433382,-9.37106945973583));
#53008=CARTESIAN_POINT('Ctrl Pts',(-5.32272986425895,1.84444578167446,-9.36634448663887));
#53009=CARTESIAN_POINT('Ctrl Pts',(-5.34342806268413,1.7917884606772,-9.36457262172751));
#53010=CARTESIAN_POINT('Ctrl Pts',(-5.3633447702337,1.73881181882729,-9.36280056977174));
#53011=CARTESIAN_POINT('Ctrl Pts',(-5.38246436805708,1.68553087368646,-9.36102812374983));
#53012=CARTESIAN_POINT('Ctrl Pts',(-5.39270432228341,1.6569949994271,-9.36007884823156));
#53013=CARTESIAN_POINT('Ctrl Pts',(-5.40271562012224,1.62837183624343,-9.35912945967968));
#53014=CARTESIAN_POINT('Ctrl Pts',(-5.41249576240362,1.59966367478316,-9.35817992629075));
#53015=CARTESIAN_POINT('Ctrl Pts',(-5.41876862300425,1.58125062006888,-9.35757090748377));
#53016=CARTESIAN_POINT('Ctrl Pts',(-5.42494329014966,1.56281169347572,-9.35696212990386));
#53017=CARTESIAN_POINT('Ctrl Pts',(-5.43101927383042,1.54434791027037,-9.35635359557542));
#53018=CARTESIAN_POINT('Ctrl Pts',(-5.4823982305406,1.38821682634118,-9.35120778535601));
#53019=CARTESIAN_POINT('Ctrl Pts',(-5.52672684681361,1.23030346915463,-9.34607912837171));
#53020=CARTESIAN_POINT('Ctrl Pts',(-5.56374821171423,1.0710197864802,-9.3409627306753));
#53021=CARTESIAN_POINT('Ctrl Pts',(-5.60035869324713,0.913503921284557,
-9.33590311756048));
#53022=CARTESIAN_POINT('Ctrl Pts',(-5.62982360628131,0.754647288089156,
-9.33085549312306));
#53023=CARTESIAN_POINT('Ctrl Pts',(-5.65184871534535,0.594826257001726,
-9.32581512456111));
#53024=CARTESIAN_POINT('Ctrl Pts',(-5.65448373952039,0.575705703302327,
-9.32521210856818));
#53025=CARTESIAN_POINT('Ctrl Pts',(-5.65701221878381,0.55657132707348,-9.32460919642916));
#53026=CARTESIAN_POINT('Ctrl Pts',(-5.65943360070479,0.537423758590119,
-9.32400638003972));
#53027=CARTESIAN_POINT('Ctrl Pts',(-5.67950244104725,0.378725334558598,
-9.31901013150466));
#53028=CARTESIAN_POINT('Ctrl Pts',(-5.69221872259358,0.219121256265095,
-9.31402046037817));
#53029=CARTESIAN_POINT('Ctrl Pts',(-5.69781027578945,0.0590179871714817,
-9.3090327524765));
#53030=CARTESIAN_POINT('Ctrl Pts',(-5.70163108079481,-0.0503833456066027,
-9.30562456540425));
#53031=CARTESIAN_POINT('Ctrl Pts',(-5.7021240585946,-0.160017990101504,
-9.3022172950059));
#53032=CARTESIAN_POINT('Ctrl Pts',(-5.69934808129051,-0.26975677675946,
-9.29880946909734));
#53033=CARTESIAN_POINT('Ctrl Pts',(-5.69780356414277,-0.330813989840834,
-9.29691339972224));
#53034=CARTESIAN_POINT('Ctrl Pts',(-5.69524689311437,-0.391903436918231,
-9.29501715837992));
#53035=CARTESIAN_POINT('Ctrl Pts',(-5.69168677241887,-0.453002721037327,
-9.29312049150345));
#53036=CARTESIAN_POINT('Ctrl Pts',(-5.68974201274654,-0.486378955700753,
-9.29208441391825));
#53037=CARTESIAN_POINT('Ctrl Pts',(-5.68749780355416,-0.519758123083858,
-9.29104820935261));
#53038=CARTESIAN_POINT('Ctrl Pts',(-5.68495543794551,-0.553136547526968,
-9.29001183647358));
#53039=CARTESIAN_POINT('Ctrl Pts',(-5.68342487061243,-0.573231189268683,
-9.28938791422254));
#53040=CARTESIAN_POINT('Ctrl Pts',(-5.68178623914004,-0.593324946043118,
-9.28876395002797));
#53041=CARTESIAN_POINT('Ctrl Pts',(-5.68004112120349,-0.613403791375216,
-9.28814034562909));
#53042=CARTESIAN_POINT('Ctrl Pts',(-5.66613823063394,-0.773366613123692,
-9.28317225520109));
#53043=CARTESIAN_POINT('Ctrl Pts',(-5.6454650766378,-0.932600507598867,
-9.27822022219613));
#53044=CARTESIAN_POINT('Ctrl Pts',(-5.61829635714927,-1.09070410950735,
-9.27327984623788));
#53045=CARTESIAN_POINT('Ctrl Pts',(-5.58917703401029,-1.26015890752813,
-9.26798477136262));
#53046=CARTESIAN_POINT('Ctrl Pts',(-5.55259634674091,-1.4283160454691,-9.26270308747931));
#53047=CARTESIAN_POINT('Ctrl Pts',(-5.5088289095376,-1.59468685397629,-9.25742937674837));
#53048=CARTESIAN_POINT('Ctrl Pts',(-5.46655380827193,-1.75538492602971,
-9.25233548344682));
#53049=CARTESIAN_POINT('Ctrl Pts',(-5.41757308364143,-1.91441717627524,
-9.24724902884695));
#53050=CARTESIAN_POINT('Ctrl Pts',(-5.36208030098775,-2.07133656286447,
-9.24216513062297));
#53051=CARTESIAN_POINT('Ctrl Pts',(-5.31874665211625,-2.19387303111163,
-9.23819517543237));
#53052=CARTESIAN_POINT('Ctrl Pts',(-5.27144095230737,-2.31512109201928,
-9.23422677908423));
#53053=CARTESIAN_POINT('Ctrl Pts',(-5.22023454988606,-2.43486046781029,
-9.23025761673876));
#53054=CARTESIAN_POINT('Ctrl Pts',(-5.19766184574894,-2.48764374051623,
-9.22850793851377));
#53055=CARTESIAN_POINT('Ctrl Pts',(-5.17433092507079,-2.54013373595243,
-9.2267581114398));
#53056=CARTESIAN_POINT('Ctrl Pts',(-5.15024683751494,-2.59231099174797,
-9.22500793637109));
#53057=CARTESIAN_POINT('Ctrl Pts',(-5.13639526128057,-2.62231990259733,
-9.22400135128326));
#53058=CARTESIAN_POINT('Ctrl Pts',(-5.12229454146471,-2.65222535832149,
-9.22299465108607));
#53059=CARTESIAN_POINT('Ctrl Pts',(-5.10794554487069,-2.68202359114896,
-9.22198779789358));
#53060=CARTESIAN_POINT('Ctrl Pts',(-5.095685933705,-2.70748284507627,-9.22112755456158));
#53061=CARTESIAN_POINT('Ctrl Pts',(-5.0832428176014,-2.73286821067675,-9.22026704943273));
#53062=CARTESIAN_POINT('Ctrl Pts',(-5.07063039957229,-2.75815032754945,
-9.21940717965711));
#53063=CARTESIAN_POINT('Ctrl Pts',(-4.99566720805045,-2.90841716494984,
-9.21429645604136));
#53064=CARTESIAN_POINT('Ctrl Pts',(-4.91465075447715,-3.05520204842461,
-9.20920264493437));
#53065=CARTESIAN_POINT('Ctrl Pts',(-4.82781920673447,-3.19807080861358,
-9.20412095685482));
#53066=CARTESIAN_POINT('Ctrl Pts',(-4.74101616741469,-3.34089266231361,
-9.19904093718862));
#53067=CARTESIAN_POINT('Ctrl Pts',(-4.64840155481371,-3.47980172218689,
-9.19397303259074));
#53068=CARTESIAN_POINT('Ctrl Pts',(-4.55016419752807,-3.61434871789838,
-9.18891245829572));
#53069=CARTESIAN_POINT('Ctrl Pts',(-4.45302663040113,-3.74738942856866,
-9.18390853831187));
#53070=CARTESIAN_POINT('Ctrl Pts',(-4.35039115846723,-3.87616588444105,
-9.17891178542071));
#53071=CARTESIAN_POINT('Ctrl Pts',(-4.24239726756525,-4.00021786115194,
-9.17391757376416));
#53072=CARTESIAN_POINT('Ctrl Pts',(-4.14727373351209,-4.10948573114406,
-9.16951855583255));
#53073=CARTESIAN_POINT('Ctrl Pts',(-4.04799214062475,-4.21508806575459,
-9.16512150951696));
#53074=CARTESIAN_POINT('Ctrl Pts',(-3.94462271981528,-4.3166870024335,-9.16072327356863));
#53075=CARTESIAN_POINT('Ctrl Pts',(-3.89293800941055,-4.36748647077295,
-9.15852415559446));
#53076=CARTESIAN_POINT('Ctrl Pts',(-3.84023098885666,-4.41728470755125,
-9.1563247402121));
#53077=CARTESIAN_POINT('Ctrl Pts',(-3.78650840229268,-4.46603693343018,
-9.15412463226547));
#53078=CARTESIAN_POINT('Ctrl Pts',(-3.76979768336693,-4.48120159313429,
-9.15344027605975));
#53079=CARTESIAN_POINT('Ctrl Pts',(-3.75298869317158,-4.49626503182372,
-9.1527558528445));
#53080=CARTESIAN_POINT('Ctrl Pts',(-3.73608160926019,-4.51122586421657,
-9.15207135072695));
#53081=CARTESIAN_POINT('Ctrl Pts',(-3.72066822985047,-4.52486493924364,
-9.15144732289933));
#53082=CARTESIAN_POINT('Ctrl Pts',(-3.70517980652966,-4.53841298498712,
-9.15082349226079));
#53083=CARTESIAN_POINT('Ctrl Pts',(-3.68961891476628,-4.55186726085941,
-9.1501999389971));
#53084=CARTESIAN_POINT('Ctrl Pts',(-3.6673746372544,-4.57110013329215,-9.14930857029843));
#53085=CARTESIAN_POINT('Ctrl Pts',(-3.64498081745003,-4.59014268141462,
-9.14841770939315));
#53086=CARTESIAN_POINT('Ctrl Pts',(-3.62243853028556,-4.60899255635498,
-9.1475273308598));
#53087=CARTESIAN_POINT('Ctrl Pts',(-3.50034074186636,-4.71109080509985,
-9.14270469467454));
#53088=CARTESIAN_POINT('Ctrl Pts',(-3.373890663402,-4.80753926503602,-9.137896209963));
#53089=CARTESIAN_POINT('Ctrl Pts',(-3.24356761447411,-4.89836659707662,
-9.1330978372056));
#53090=CARTESIAN_POINT('Ctrl Pts',(-3.10895860137107,-4.99218098853959,
-9.12814165925635));
#53091=CARTESIAN_POINT('Ctrl Pts',(-2.97021723316815,-5.07999878946387,
-9.12319626930637));
#53092=CARTESIAN_POINT('Ctrl Pts',(-2.82783156379497,-5.16181301723526,
-9.11825721603946));
#53093=CARTESIAN_POINT('Ctrl Pts',(-2.68343867607943,-5.24478058452017,
-9.11324853667636));
#53094=CARTESIAN_POINT('Ctrl Pts',(-2.53529736368481,-5.32157438622776,
-9.10824637391274));
#53095=CARTESIAN_POINT('Ctrl Pts',(-2.38388466705377,-5.39214360897498,
-9.10324608551482));
#53096=CARTESIAN_POINT('Ctrl Pts',(-2.23107388974751,-5.4633644380193,-9.09819962657284));
#53097=CARTESIAN_POINT('Ctrl Pts',(-2.07493030423668,-5.5282454698157,-9.09315507677058));
#53098=CARTESIAN_POINT('Ctrl Pts',(-1.91592251661704,-5.58668647934873,
-9.08810766408999));
#53099=CARTESIAN_POINT('Ctrl Pts',(-1.86492339105374,-5.6054304693623,-9.08648878971332));
#53100=CARTESIAN_POINT('Ctrl Pts',(-1.81362950493446,-5.6235115915611,-9.08486962083241));
#53101=CARTESIAN_POINT('Ctrl Pts',(-1.76205604469197,-5.64092543727167,
-9.08325));
#53102=CARTESIAN_POINT('Origin',(0.,0.,-10.));
#53103=CARTESIAN_POINT('Origin',(0.,0.,-10.));
#53104=CARTESIAN_POINT('',(2.85706463458463,-4.00329423553975,-10.));
#53105=CARTESIAN_POINT('Ctrl Pts',(3.54751238410106,-3.52143928316762,-10.));
#53106=CARTESIAN_POINT('Ctrl Pts',(3.43727113798793,-3.61340023595403,-10.));
#53107=CARTESIAN_POINT('Ctrl Pts',(3.32309228486466,-3.70055940759421,-10.));
#53108=CARTESIAN_POINT('Ctrl Pts',(3.20515669348447,-3.78259068630623,-10.));
#53109=CARTESIAN_POINT('Ctrl Pts',(3.09250600088469,-3.86094600087759,-10.));
#53110=CARTESIAN_POINT('Ctrl Pts',(2.97642721282368,-3.93462271815296,-10.));
#53111=CARTESIAN_POINT('Ctrl Pts',(2.85706463458369,-4.00329423554042,-10.));
#53112=CARTESIAN_POINT('',(-2.85706463458558,-4.00329423553907,-10.));
#53113=CARTESIAN_POINT('Origin',(0.,0.,-10.));
#53114=CARTESIAN_POINT('Ctrl Pts',(-2.85711522928017,-4.00149011032074,
-10.));
#53115=CARTESIAN_POINT('Ctrl Pts',(-2.98510663627035,-3.92827452489103,
-10.));
#53116=CARTESIAN_POINT('Ctrl Pts',(-3.10954218075165,-3.84942396520819,
-10.));
#53117=CARTESIAN_POINT('Ctrl Pts',(-3.2300790650384,-3.76515943171096,-10.));
#53118=CARTESIAN_POINT('Ctrl Pts',(-3.33981495603391,-3.68844562151621,
-10.));
#53119=CARTESIAN_POINT('Ctrl Pts',(-3.4463200216345,-3.60724388606328,-10.));
#53120=CARTESIAN_POINT('Ctrl Pts',(-3.54932990765358,-3.52168385953437,
-10.));
#53121=CARTESIAN_POINT('Origin',(0.,0.,147.5));
#53122=CARTESIAN_POINT('',(-5.,-6.12323399573677E-16,147.));
#53123=CARTESIAN_POINT('Origin',(0.,0.,147.));
#53124=CARTESIAN_POINT('',(-5.,-6.12323399573677E-16,148.));
#53125=CARTESIAN_POINT('',(-5.,-6.12323399573677E-16,147.5));
#53126=CARTESIAN_POINT('Origin',(0.,0.,148.));
#53127=CARTESIAN_POINT('Origin',(9.,0.,147.));
#53128=CARTESIAN_POINT('Origin',(5.,0.,148.));
#53129=CARTESIAN_POINT('',(-5.91675,-7.2459289488551E-16,148.));
#53130=CARTESIAN_POINT('Origin',(0.,0.,148.));
#53131=CARTESIAN_POINT('Origin',(0.,0.,-10.));
#53132=CARTESIAN_POINT('',(-5.91675,7.2459289488551E-16,162.));
#53133=CARTESIAN_POINT('Origin',(0.,0.,162.));
#53134=CARTESIAN_POINT('',(-5.91675,-7.2459289488551E-16,-10.));
#53135=CARTESIAN_POINT('Origin',(7.01450167938425E-16,2.84304068604708E-16,
130.));
#53136=CARTESIAN_POINT('Ctrl Pts',(2.86417334265909,-4.00661193697115,130.));
#53137=CARTESIAN_POINT('Ctrl Pts',(2.96578276202768,-3.94896682571219,130.));
#53138=CARTESIAN_POINT('Ctrl Pts',(3.06499684984438,-3.88759437514104,130.));
#53139=CARTESIAN_POINT('Ctrl Pts',(3.16157834138731,-3.82254108203266,130.));
#53140=CARTESIAN_POINT('Ctrl Pts',(3.2788139169888,-3.74357605322128,130.));
#53141=CARTESIAN_POINT('Ctrl Pts',(3.39217184567194,-3.65918923033172,130.));
#53142=CARTESIAN_POINT('Ctrl Pts',(3.50155723888932,-3.56980772067352,130.));
#53143=CARTESIAN_POINT('Ctrl Pts',(3.57830130427611,-3.50709824713396,130.));
#53144=CARTESIAN_POINT('Ctrl Pts',(3.65308960208866,-3.44192910170494,130.));
#53145=CARTESIAN_POINT('Ctrl Pts',(3.72588284987221,-3.37443414400712,130.));
#53146=CARTESIAN_POINT('Ctrl Pts',(3.76351932356994,-3.33953705839175,130.));
#53147=CARTESIAN_POINT('Ctrl Pts',(3.80062238017016,-3.30401805771336,130.));
#53148=CARTESIAN_POINT('Ctrl Pts',(3.83718593267987,-3.26789459823601,130.));
#53149=CARTESIAN_POINT('Ctrl Pts',(3.8553536472403,-3.24994555730117,130.));
#53150=CARTESIAN_POINT('Ctrl Pts',(3.87338815622643,-3.23184727089816,130.));
#53151=CARTESIAN_POINT('Ctrl Pts',(3.89128866818473,-3.21360182011092,130.));
#53152=CARTESIAN_POINT('Ctrl Pts',(3.90755204940963,-3.19702504719714,130.));
#53153=CARTESIAN_POINT('Ctrl Pts',(3.92369773306074,-3.18033401739892,130.));
#53154=CARTESIAN_POINT('Ctrl Pts',(3.93972478721132,-3.16353123186673,130.));
#53155=CARTESIAN_POINT('Ctrl Pts',(4.04018601889038,-3.05820753891966,130.));
#53156=CARTESIAN_POINT('Ctrl Pts',(4.13599554083928,-2.94848917560709,130.));
#53157=CARTESIAN_POINT('Ctrl Pts',(4.22705195107335,-2.83481997013712,130.));
#53158=CARTESIAN_POINT('Ctrl Pts',(4.32452800844826,-2.7131368731902,130.));
#53159=CARTESIAN_POINT('Ctrl Pts',(4.41655796319061,-2.58692609159507,130.));
#53160=CARTESIAN_POINT('Ctrl Pts',(4.50298379913026,-2.45667794374954,130.));
#53161=CARTESIAN_POINT('Ctrl Pts',(4.54079510235386,-2.39969437906712,130.));
#53162=CARTESIAN_POINT('Ctrl Pts',(4.57753324901869,-2.34193738296473,130.));
#53163=CARTESIAN_POINT('Ctrl Pts',(4.61318252808862,-2.2834452270631,130.));
#53164=CARTESIAN_POINT('Ctrl Pts',(4.6392253424799,-2.24071504010746,130.));
#53165=CARTESIAN_POINT('Ctrl Pts',(4.66468702707171,-2.19759248458433,130.));
#53166=CARTESIAN_POINT('Ctrl Pts',(4.68956089066644,-2.15409199395247,130.));
#53167=CARTESIAN_POINT('Ctrl Pts',(4.69918353646736,-2.13726349395196,130.));
#53168=CARTESIAN_POINT('Ctrl Pts',(4.70871686517466,-2.12038070842633,130.));
#53169=CARTESIAN_POINT('Ctrl Pts',(4.71815642930611,-2.1034520684253,130.));
#53170=CARTESIAN_POINT('Ctrl Pts',(4.79232967335433,-1.97043192801249,130.));
#53171=CARTESIAN_POINT('Ctrl Pts',(4.86079223538357,-1.83445140446128,130.));
#53172=CARTESIAN_POINT('Ctrl Pts',(4.9234351422813,-1.69597533119363,130.));
#53173=CARTESIAN_POINT('Ctrl Pts',(4.98692662668076,-1.5556234241545,130.));
#53174=CARTESIAN_POINT('Ctrl Pts',(5.04444021787131,-1.41270730386396,130.));
#53175=CARTESIAN_POINT('Ctrl Pts',(5.09582801483642,-1.26766968144916,130.));
#53176=CARTESIAN_POINT('Ctrl Pts',(5.14739091908899,-1.12213783382644,130.));
#53177=CARTESIAN_POINT('Ctrl Pts',(5.19278668030377,-0.974469303347938,
130.));
#53178=CARTESIAN_POINT('Ctrl Pts',(5.23182419840718,-0.825079944137655,
130.));
#53179=CARTESIAN_POINT('Ctrl Pts',(5.26318419108894,-0.705071054249778,
130.));
#53180=CARTESIAN_POINT('Ctrl Pts',(5.29044026624906,-0.583950896370881,
130.));
#53181=CARTESIAN_POINT('Ctrl Pts',(5.31347082763723,-0.461925133621565,
130.));
#53182=CARTESIAN_POINT('Ctrl Pts',(5.32241008870535,-0.414561105803583,
130.));
#53183=CARTESIAN_POINT('Ctrl Pts',(5.33071251100927,-0.367060569029899,
130.));
#53184=CARTESIAN_POINT('Ctrl Pts',(5.33837008369061,-0.319435324949108,
130.));
#53185=CARTESIAN_POINT('Ctrl Pts',(5.34328214856315,-0.288885397677037,
130.));
#53186=CARTESIAN_POINT('Ctrl Pts',(5.34792886200234,-0.258284154039901,
130.));
#53187=CARTESIAN_POINT('Ctrl Pts',(5.35230799414418,-0.227634691612514,
130.));
#53188=CARTESIAN_POINT('Ctrl Pts',(5.35503902012298,-0.208520292819688,
130.));
#53189=CARTESIAN_POINT('Ctrl Pts',(5.3576652805494,-0.189391776026415,130.));
#53190=CARTESIAN_POINT('Ctrl Pts',(5.36018540154735,-0.170257938742505,
130.));
#53191=CARTESIAN_POINT('Ctrl Pts',(5.38088704007115,-0.0130822383109732,
130.));
#53192=CARTESIAN_POINT('Ctrl Pts',(5.39445343673034,0.144612493973096,130.));
#53193=CARTESIAN_POINT('Ctrl Pts',(5.40073333988398,0.302371939349598,130.));
#53194=CARTESIAN_POINT('Ctrl Pts',(5.40532221026111,0.417650412263869,130.));
#53195=CARTESIAN_POINT('Ctrl Pts',(5.40601960721486,0.532964206250372,130.));
#53196=CARTESIAN_POINT('Ctrl Pts',(5.40275094325442,0.648144274292171,130.));
#53197=CARTESIAN_POINT('Ctrl Pts',(5.39842112123799,0.800717068711322,130.));
#53198=CARTESIAN_POINT('Ctrl Pts',(5.38713445618709,0.953055205515926,130.));
#53199=CARTESIAN_POINT('Ctrl Pts',(5.36917158042469,1.10477541171324,130.));
#53200=CARTESIAN_POINT('Ctrl Pts',(5.35092698461533,1.25887511572479,130.));
#53201=CARTESIAN_POINT('Ctrl Pts',(5.32579502801831,1.4123380456589,130.));
#53202=CARTESIAN_POINT('Ctrl Pts',(5.29401591504677,1.56476615531412,130.));
#53203=CARTESIAN_POINT('Ctrl Pts',(5.27817026521515,1.64076961243561,130.));
#53204=CARTESIAN_POINT('Ctrl Pts',(5.26067117500297,1.71651578167034,130.));
#53205=CARTESIAN_POINT('Ctrl Pts',(5.24154366365584,1.79195479764749,130.));
#53206=CARTESIAN_POINT('Ctrl Pts',(5.2352532364493,1.81676427912813,130.));
#53207=CARTESIAN_POINT('Ctrl Pts',(5.22878666396949,1.8415405356193,130.));
#53208=CARTESIAN_POINT('Ctrl Pts',(5.22214476416494,1.86628177640074,130.));
#53209=CARTESIAN_POINT('Ctrl Pts',(5.21735806229335,1.88411235907121,130.));
#53210=CARTESIAN_POINT('Ctrl Pts',(5.2124811310063,1.90192154477755,130.));
#53211=CARTESIAN_POINT('Ctrl Pts',(5.20751665209725,1.91970078810442,130.));
#53212=CARTESIAN_POINT('Ctrl Pts',(5.16515981846288,2.0713929325444,130.));
#53213=CARTESIAN_POINT('Ctrl Pts',(5.11638897344517,2.22107460978644,130.));
#53214=CARTESIAN_POINT('Ctrl Pts',(5.0615294421976,2.3683471330429,130.));
#53215=CARTESIAN_POINT('Ctrl Pts',(5.00580294678831,2.51794705496218,130.));
#53216=CARTESIAN_POINT('Ctrl Pts',(4.94379366704092,2.66506178406266,130.));
#53217=CARTESIAN_POINT('Ctrl Pts',(4.87578870350513,2.80927707437429,130.));
#53218=CARTESIAN_POINT('Ctrl Pts',(4.80697460991496,2.9552082530509,130.));
#53219=CARTESIAN_POINT('Ctrl Pts',(4.7320211223972,3.09817137776604,130.));
#53220=CARTESIAN_POINT('Ctrl Pts',(4.65117345482382,3.23772952533661,130.));
#53221=CARTESIAN_POINT('Ctrl Pts',(4.64031025008783,3.25648144206022,130.));
#53222=CARTESIAN_POINT('Ctrl Pts',(4.62934055615847,3.27517186246557,130.));
#53223=CARTESIAN_POINT('Ctrl Pts',(4.61826490004014,3.29379970385774,130.));
#53224=CARTESIAN_POINT('Ctrl Pts',(4.55640877022608,3.3978338272541,130.));
#53225=CARTESIAN_POINT('Ctrl Pts',(4.49124877272854,3.499916689806,130.));
#53226=CARTESIAN_POINT('Ctrl Pts',(4.42288946352048,3.5999300492289,130.));
#53227=CARTESIAN_POINT('Ctrl Pts',(4.39298226574196,3.64368589397642,130.));
#53228=CARTESIAN_POINT('Ctrl Pts',(4.3624625121461,3.68704552115934,130.));
#53229=CARTESIAN_POINT('Ctrl Pts',(4.3313381114467,3.72999850731393,130.));
#53230=CARTESIAN_POINT('Ctrl Pts',(4.31168386061072,3.75712220271259,130.));
#53231=CARTESIAN_POINT('Ctrl Pts',(4.29178849095401,3.78408373943631,130.));
#53232=CARTESIAN_POINT('Ctrl Pts',(4.27165389347949,3.81088041853506,130.));
#53233=CARTESIAN_POINT('Ctrl Pts',(4.25892564129572,3.82782016067234,130.));
#53234=CARTESIAN_POINT('Ctrl Pts',(4.24610132908206,3.84469453115168,130.));
#53235=CARTESIAN_POINT('Ctrl Pts',(4.23319137984965,3.8614901296792,130.));
#53236=CARTESIAN_POINT('Ctrl Pts',(4.1334204286307,3.99129024052502,130.));
#53237=CARTESIAN_POINT('Ctrl Pts',(4.02840245584316,4.11657006442815,130.));
#53238=CARTESIAN_POINT('Ctrl Pts',(3.91847912791786,4.2370855331423,130.));
#53239=CARTESIAN_POINT('Ctrl Pts',(3.80717191983546,4.3591182318105,130.));
#53240=CARTESIAN_POINT('Ctrl Pts',(3.69083477586065,4.47626647053335,130.));
#53241=CARTESIAN_POINT('Ctrl Pts',(3.56977267870164,4.58825804551576,130.));
#53242=CARTESIAN_POINT('Ctrl Pts',(3.4488161551608,4.70015195693499,130.));
#53243=CARTESIAN_POINT('Ctrl Pts',(3.32314251076017,4.80689878301852,130.));
#53244=CARTESIAN_POINT('Ctrl Pts',(3.19301198855863,4.908199402403,130.));
#53245=CARTESIAN_POINT('Ctrl Pts',(3.06455341841885,5.00819848409614,130.));
#53246=CARTESIAN_POINT('Ctrl Pts',(2.93175130061798,5.1028909152538,130.));
#53247=CARTESIAN_POINT('Ctrl Pts',(2.79481968753776,5.19195398985847,130.));
#53248=CARTESIAN_POINT('Ctrl Pts',(2.72556825359359,5.236996515022,130.));
#53249=CARTESIAN_POINT('Ctrl Pts',(2.65526008082166,5.28059861334327,130.));
#53250=CARTESIAN_POINT('Ctrl Pts',(2.58391981634458,5.32271443393329,130.));
#53251=CARTESIAN_POINT('Ctrl Pts',(-2.59168464642813,5.32810255942583,130.));
#53252=CARTESIAN_POINT('Ctrl Pts',(-2.71132798771431,5.25826632968106,130.));
#53253=CARTESIAN_POINT('Ctrl Pts',(-2.82813785948501,5.18406707412924,130.));
#53254=CARTESIAN_POINT('Ctrl Pts',(-2.94183908547589,5.10549286651818,130.));
#53255=CARTESIAN_POINT('Ctrl Pts',(-3.07753195615672,5.01172114418801,130.));
#53256=CARTESIAN_POINT('Ctrl Pts',(-3.20879856093728,4.91171884717559,130.));
#53257=CARTESIAN_POINT('Ctrl Pts',(-3.33544390790157,4.80592591755381,130.));
#53258=CARTESIAN_POINT('Ctrl Pts',(-3.41766258017248,4.73724471909174,130.));
#53259=CARTESIAN_POINT('Ctrl Pts',(-3.49793277631496,4.6661221713314,130.));
#53260=CARTESIAN_POINT('Ctrl Pts',(-3.57619172699311,4.59267182290119,130.));
#53261=CARTESIAN_POINT('Ctrl Pts',(-3.62721998191113,4.54477898673313,130.));
#53262=CARTESIAN_POINT('Ctrl Pts',(-3.67739297975411,4.49589635854078,130.));
#53263=CARTESIAN_POINT('Ctrl Pts',(-3.72669148950679,4.44605450340122,130.));
#53264=CARTESIAN_POINT('Ctrl Pts',(-3.74722649737596,4.42529316816736,130.));
#53265=CARTESIAN_POINT('Ctrl Pts',(-3.76760975587872,4.40436539092426,130.));
#53266=CARTESIAN_POINT('Ctrl Pts',(-3.78783979790461,4.38327335155342,130.));
#53267=CARTESIAN_POINT('Ctrl Pts',(-3.80599703519715,4.36434243863936,130.));
#53268=CARTESIAN_POINT('Ctrl Pts',(-3.82402508596036,4.34528516998115,130.));
#53269=CARTESIAN_POINT('Ctrl Pts',(-3.8419196208096,4.32610718559679,130.));
#53270=CARTESIAN_POINT('Ctrl Pts',(-3.95373953775787,4.20626720991925,130.));
#53271=CARTESIAN_POINT('Ctrl Pts',(-4.06039477934112,4.0816687766888,130.));
#53272=CARTESIAN_POINT('Ctrl Pts',(-4.16169333226532,3.95274377575036,130.));
#53273=CARTESIAN_POINT('Ctrl Pts',(-4.26401219978641,3.82252019692935,130.));
#53274=CARTESIAN_POINT('Ctrl Pts',(-4.36086631611474,3.68788169668274,130.));
#53275=CARTESIAN_POINT('Ctrl Pts',(-4.45201053252839,3.54924911468795,130.));
#53276=CARTESIAN_POINT('Ctrl Pts',(-4.53334388495471,3.42553909673154,130.));
#53277=CARTESIAN_POINT('Ctrl Pts',(-4.61012992925456,3.29864786635624,130.));
#53278=CARTESIAN_POINT('Ctrl Pts',(-4.68215943876187,3.16886588604444,130.));
#53279=CARTESIAN_POINT('Ctrl Pts',(-4.69302130707921,3.14929509082797,130.));
#53280=CARTESIAN_POINT('Ctrl Pts',(-4.70377084455898,3.12966591564697,130.));
#53281=CARTESIAN_POINT('Ctrl Pts',(-4.71440565460736,3.10998302703064,130.));
#53282=CARTESIAN_POINT('Ctrl Pts',(-4.79134796001078,2.96757833712556,130.));
#53283=CARTESIAN_POINT('Ctrl Pts',(-4.86232208226549,2.82230393704696,130.));
#53284=CARTESIAN_POINT('Ctrl Pts',(-4.92714211255705,2.67456634541395,130.));
#53285=CARTESIAN_POINT('Ctrl Pts',(-4.99165161938617,2.52753649779587,130.));
#53286=CARTESIAN_POINT('Ctrl Pts',(-5.05006608621869,2.37806623720806,130.));
#53287=CARTESIAN_POINT('Ctrl Pts',(-5.10215320174004,2.22654123991806,130.));
#53288=CARTESIAN_POINT('Ctrl Pts',(-5.15352370275379,2.07710092346008,130.));
#53289=CARTESIAN_POINT('Ctrl Pts',(-5.19873989699047,1.92566131722251,130.));
#53290=CARTESIAN_POINT('Ctrl Pts',(-5.23752848087705,1.77258862010428,130.));
#53291=CARTESIAN_POINT('Ctrl Pts',(-5.26873343336441,1.64944346340934,130.));
#53292=CARTESIAN_POINT('Ctrl Pts',(-5.29577752888173,1.52524116094855,130.));
#53293=CARTESIAN_POINT('Ctrl Pts',(-5.31849325398757,1.40017510822192,130.));
#53294=CARTESIAN_POINT('Ctrl Pts',(-5.32868054202697,1.34408691833846,130.));
#53295=CARTESIAN_POINT('Ctrl Pts',(-5.33799698071074,1.28782506394763,130.));
#53296=CARTESIAN_POINT('Ctrl Pts',(-5.34642591588743,1.23140734783872,130.));
#53297=CARTESIAN_POINT('Ctrl Pts',(-5.35149623877264,1.19746996059804,130.));
#53298=CARTESIAN_POINT('Ctrl Pts',(-5.35624540188262,1.16347618014318,130.));
#53299=CARTESIAN_POINT('Ctrl Pts',(-5.36066960833698,1.12942993355321,130.));
#53300=CARTESIAN_POINT('Ctrl Pts',(-5.36337465687219,1.1086133757326,130.));
#53301=CARTESIAN_POINT('Ctrl Pts',(-5.36595716110829,1.08778520479147,130.));
#53302=CARTESIAN_POINT('Ctrl Pts',(-5.36841592606578,1.06695188444939,130.));
#53303=CARTESIAN_POINT('Ctrl Pts',(-5.38643209853856,0.914299354031173,
130.));
#53304=CARTESIAN_POINT('Ctrl Pts',(-5.39782132330128,0.76127519594384,130.));
#53305=CARTESIAN_POINT('Ctrl Pts',(-5.40237196850048,0.60822166947751,130.));
#53306=CARTESIAN_POINT('Ctrl Pts',(-5.40579165332522,0.493206149937382,
130.));
#53307=CARTESIAN_POINT('Ctrl Pts',(-5.40534852701692,0.37817386832857,130.));
#53308=CARTESIAN_POINT('Ctrl Pts',(-5.4009333780326,0.263271286956652,130.));
#53309=CARTESIAN_POINT('Ctrl Pts',(-5.39498435461679,0.10845020401096,130.));
#53310=CARTESIAN_POINT('Ctrl Pts',(-5.38182560150715,-0.0461364505366216,
130.));
#53311=CARTESIAN_POINT('Ctrl Pts',(-5.36166329395989,-0.200029125946722,
130.));
#53312=CARTESIAN_POINT('Ctrl Pts',(-5.34151584033518,-0.353808425946975,
130.));
#53313=CARTESIAN_POINT('Ctrl Pts',(-5.31437470356353,-0.506895541187959,
130.));
#53314=CARTESIAN_POINT('Ctrl Pts',(-5.28039992254779,-0.658807623106542,
130.));
#53315=CARTESIAN_POINT('Ctrl Pts',(-5.26472627071547,-0.728889519440523,
130.));
#53316=CARTESIAN_POINT('Ctrl Pts',(-5.24759763676859,-0.798720925805533,
130.));
#53317=CARTESIAN_POINT('Ctrl Pts',(-5.22902684970209,-0.868251994011044,
130.));
#53318=CARTESIAN_POINT('Ctrl Pts',(-5.22301676236688,-0.890754421664162,
130.));
#53319=CARTESIAN_POINT('Ctrl Pts',(-5.21685561466066,-0.913225379026263,
130.));
#53320=CARTESIAN_POINT('Ctrl Pts',(-5.21054380404271,-0.935663135660378,
130.));
#53321=CARTESIAN_POINT('Ctrl Pts',(-5.20486822320544,-0.955839169019444,
130.));
#53322=CARTESIAN_POINT('Ctrl Pts',(-5.19907277575825,-0.975981308264116,
130.));
#53323=CARTESIAN_POINT('Ctrl Pts',(-5.19316007549178,-0.996081558145602,
130.));
#53324=CARTESIAN_POINT('Ctrl Pts',(-5.15023736011681,-1.14199751291171,
130.));
#53325=CARTESIAN_POINT('Ctrl Pts',(-5.1011075998424,-1.28582149559654,130.));
#53326=CARTESIAN_POINT('Ctrl Pts',(-5.04599926784503,-1.42713283539364,
130.));
#53327=CARTESIAN_POINT('Ctrl Pts',(-4.99026887878914,-1.5700392827395,130.));
#53328=CARTESIAN_POINT('Ctrl Pts',(-4.9284237967488,-1.71037686011977,130.));
#53329=CARTESIAN_POINT('Ctrl Pts',(-4.86065301345585,-1.84768459305006,
130.));
#53330=CARTESIAN_POINT('Ctrl Pts',(-4.7928822301629,-1.98499232598035,130.));
#53331=CARTESIAN_POINT('Ctrl Pts',(-4.71918527961721,-2.11927098094242,
130.));
#53332=CARTESIAN_POINT('Ctrl Pts',(-4.63971068055132,-2.25002196879991,
130.));
#53333=CARTESIAN_POINT('Ctrl Pts',(-4.5849160685212,-2.34016963530484,130.));
#53334=CARTESIAN_POINT('Ctrl Pts',(-4.52737412606546,-2.4286395222737,130.));
#53335=CARTESIAN_POINT('Ctrl Pts',(-4.46715124519521,-2.51531152444212,
130.));
#53336=CARTESIAN_POINT('Ctrl Pts',(-4.43566885186282,-2.56062058345327,
130.));
#53337=CARTESIAN_POINT('Ctrl Pts',(-4.40345369451756,-2.60543813700367,
130.));
#53338=CARTESIAN_POINT('Ctrl Pts',(-4.37051460776245,-2.64974581524745,
130.));
#53339=CARTESIAN_POINT('Ctrl Pts',(-4.3498704560937,-2.67751508634336,130.));
#53340=CARTESIAN_POINT('Ctrl Pts',(-4.32894193686738,-2.70508406168616,
130.));
#53341=CARTESIAN_POINT('Ctrl Pts',(-4.30773114742818,-2.73244804114046,
130.));
#53342=CARTESIAN_POINT('Ctrl Pts',(-4.29561742812669,-2.74807591614397,
130.));
#53343=CARTESIAN_POINT('Ctrl Pts',(-4.28341758933611,-2.76362923604917,
130.));
#53344=CARTESIAN_POINT('Ctrl Pts',(-4.27113373590674,-2.77910551783698,
130.));
#53345=CARTESIAN_POINT('Ctrl Pts',(-4.17940507365103,-2.89467337553329,
130.));
#53346=CARTESIAN_POINT('Ctrl Pts',(-4.08296782193032,-3.00598297629126,
130.));
#53347=CARTESIAN_POINT('Ctrl Pts',(-3.98206514775803,-3.11276944435602,
130.));
#53348=CARTESIAN_POINT('Ctrl Pts',(-3.88164013777467,-3.21905039488049,
130.));
#53349=CARTESIAN_POINT('Ctrl Pts',(-3.77679132028946,-3.32085136116889,
130.));
#53350=CARTESIAN_POINT('Ctrl Pts',(-3.66772668560753,-3.41787103111659,
130.));
#53351=CARTESIAN_POINT('Ctrl Pts',(-3.55974446398038,-3.51392782838216,
130.));
#53352=CARTESIAN_POINT('Ctrl Pts',(-3.44762915219098,-3.60529811873874,
130.));
#53353=CARTESIAN_POINT('Ctrl Pts',(-3.33155962241286,-3.69164424731295,
130.));
#53354=CARTESIAN_POINT('Ctrl Pts',(-3.21783010743005,-3.7762495984517,130.));
#53355=CARTESIAN_POINT('Ctrl Pts',(-3.10030370603907,-3.85603155384217,
130.));
#53356=CARTESIAN_POINT('Ctrl Pts',(-2.97913416561654,-3.93062466590592,
130.));
#53357=CARTESIAN_POINT('Ctrl Pts',(-2.93884537173577,-3.95542682745891,
130.));
#53358=CARTESIAN_POINT('Ctrl Pts',(-2.89815371868312,-3.97965491914145,
130.));
#53359=CARTESIAN_POINT('Ctrl Pts',(-2.85706463458608,-4.00329423553871,
130.));
#53360=CARTESIAN_POINT('Ctrl Pts',(-3.49129836376668,-3.46410432834522,
-10.0471983845063));
#53361=CARTESIAN_POINT('Ctrl Pts',(-2.91414933031449,-4.04578411773647,
-10.0007944088984));
#53362=CARTESIAN_POINT('Ctrl Pts',(-1.46740602186593,-4.90364861172812,
-9.90798645768269));
#53363=CARTESIAN_POINT('Ctrl Pts',(1.92453937789233,-5.07348089440844,-9.72237055525127));
#53364=CARTESIAN_POINT('Ctrl Pts',(5.43970692864372,-2.05961707410548,-9.49035067721199));
#53365=CARTESIAN_POINT('Ctrl Pts',(4.67141455431437,3.47170793039274,-9.21192682356487));
#53366=CARTESIAN_POINT('Ctrl Pts',(-0.394303111254869,5.8022423708097,-8.93350296991773));
#53367=CARTESIAN_POINT('Ctrl Pts',(-5.09502701080405,2.80733175830066,-8.65507911627061));
#53368=CARTESIAN_POINT('Ctrl Pts',(-5.11582220422363,-2.76998183349922,
-8.37665526262347));
#53369=CARTESIAN_POINT('Ctrl Pts',(-0.435410493021885,-5.80062512701066,
-8.09823140897635));
#53370=CARTESIAN_POINT('Ctrl Pts',(4.64466218789312,-3.50245220498147,-7.81980755532921));
#53371=CARTESIAN_POINT('Ctrl Pts',(5.45739468419239,2.01424609607877,-7.54138370168209));
#53372=CARTESIAN_POINT('Ctrl Pts',(1.25572029180289,5.68000375627327,-7.26295984803495));
#53373=CARTESIAN_POINT('Ctrl Pts',(-4.09966034597428,4.1270561564691,-6.98453599438783));
#53374=CARTESIAN_POINT('Ctrl Pts',(-5.68827338584756,-1.21792801260327,
-6.70611214074069));
#53375=CARTESIAN_POINT('Ctrl Pts',(-2.05044135574297,-5.44383565780062,
-6.42768828709357));
#53376=CARTESIAN_POINT('Ctrl Pts',(3.47134289591715,-4.66792459610127,-6.14926443344644));
#53377=CARTESIAN_POINT('Ctrl Pts',(5.803635743461,0.3969206476142,-5.8708405797993));
#53378=CARTESIAN_POINT('Ctrl Pts',(2.80350181475234,5.09706699486434,-5.59241672615218));
#53379=CARTESIAN_POINT('Ctrl Pts',(-2.77250943461248,5.11399248292585,-5.31399287250505));
#53380=CARTESIAN_POINT('Ctrl Pts',(-5.80111878332751,0.43214162495672,-5.03556901885792));
#53381=CARTESIAN_POINT('Ctrl Pts',(-3.49961605198755,-4.64676344512396,
-4.75714516521079));
#53382=CARTESIAN_POINT('Ctrl Pts',(2.01736012333282,-5.4561876061593,-4.47872131156366));
#53383=CARTESIAN_POINT('Ctrl Pts',(5.68077069634635,-1.25242520393326,-4.20029745791653));
#53384=CARTESIAN_POINT('Ctrl Pts',(4.12464623088233,4.10207481179193,-3.9218736042694));
#53385=CARTESIAN_POINT('Ctrl Pts',(-1.22123428830395,5.68755759612714,-3.64344975062227));
#53386=CARTESIAN_POINT('Ctrl Pts',(-5.44503554290356,2.04726950927692,-3.36502589697514));
#53387=CARTESIAN_POINT('Ctrl Pts',(-4.66589704313019,-3.47406523478677,
-3.08660204332801));
#53388=CARTESIAN_POINT('Ctrl Pts',(0.400302865534793,-5.80340263407658,
-2.80817818968088));
#53389=CARTESIAN_POINT('Ctrl Pts',(5.09870148282997,-2.80052989457494,-2.52975433603375));
#53390=CARTESIAN_POINT('Ctrl Pts',(5.11237470052847,2.77549084296867,-2.25133048238662));
#53391=CARTESIAN_POINT('Ctrl Pts',(0.42875946485938,5.80136965084335,-1.97290662873949));
#53392=CARTESIAN_POINT('Ctrl Pts',(-4.64880320297601,3.49690624434093,-1.69448277509236));
#53393=CARTESIAN_POINT('Ctrl Pts',(-5.45501040680013,-2.02054100754454,
-1.41605892144523));
#53394=CARTESIAN_POINT('Ctrl Pts',(-1.24911288418635,-5.68149993443013,
-1.1376350677981));
#53395=CARTESIAN_POINT('Ctrl Pts',(4.10447898256108,-4.12225384754937,-0.859211214150975));
#53396=CARTESIAN_POINT('Ctrl Pts',(5.68684458676181,1.22455018188017,-0.580787360503842));
#53397=CARTESIAN_POINT('Ctrl Pts',(2.04409447042155,5.44622826349031,-0.302363506856717));
#53398=CARTESIAN_POINT('Ctrl Pts',(-3.47678507055683,4.66387071809777,-0.0239396532095809));
#53399=CARTESIAN_POINT('Ctrl Pts',(-5.80316825208324,-0.403686437716624,
0.254484200437544));
#53400=CARTESIAN_POINT('Ctrl Pts',(-2.79755665155426,-5.10033344825063,
0.532908054084678));
#53401=CARTESIAN_POINT('Ctrl Pts',(2.7784711114303,-5.11075559823943,0.811331907731805));
#53402=CARTESIAN_POINT('Ctrl Pts',(5.80161865024956,-0.425376937628951,
1.08975576137894));
#53403=CARTESIAN_POINT('Ctrl Pts',(3.49419519287011,4.65084126326794,1.36817961502607));
#53404=CARTESIAN_POINT('Ctrl Pts',(-2.02372117571978,5.45383141515521,1.64660346867319));
#53405=CARTESIAN_POINT('Ctrl Pts',(-5.68222725659244,1.24580010693086,1.92502732232033));
#53406=CARTESIAN_POINT('Ctrl Pts',(-4.11986005471321,-4.10688174063604,
2.20345117596745));
#53407=CARTESIAN_POINT('Ctrl Pts',(1.22786565484881,-5.68612965343156,2.48187502961459));
#53408=CARTESIAN_POINT('Ctrl Pts',(5.44741913497888,-2.040918731811,2.76029888326171));
#53409=CARTESIAN_POINT('Ctrl Pts',(4.6618428064117,3.47950372184003,3.03872273690884));
#53410=CARTESIAN_POINT('Ctrl Pts',(-0.407069872025434,5.80293189872846,
3.31714659055597));
#53411=CARTESIAN_POINT('Ctrl Pts',(-5.10196368020262,2.79458245680537,3.59557044420311));
#53412=CARTESIAN_POINT('Ctrl Pts',(-5.10913475841737,-2.78145043499297,
3.87399429785023));
#53413=CARTESIAN_POINT('Ctrl Pts',(-0.421994265891336,-5.80186567765455,
4.15241815149737));
#53414=CARTESIAN_POINT('Ctrl Pts',(4.65287774260152,-3.49148295347327,4.43084200514448));
#53415=CARTESIAN_POINT('Ctrl Pts',(5.45265056950567,2.02690065589327,4.70926585879163));
#53416=CARTESIAN_POINT('Ctrl Pts',(1.24248690619172,5.68295264716619,4.98768971243874));
#53417=CARTESIAN_POINT('Ctrl Pts',(-4.10928310262335,4.11746486135404,5.26611356608589));
#53418=CARTESIAN_POINT('Ctrl Pts',(-5.68541278715194,-1.23118071040779,
5.544537419733));
#53419=CARTESIAN_POINT('Ctrl Pts',(-2.03774229941179,-5.44860815467391,
5.82296127338016));
#53420=CARTESIAN_POINT('Ctrl Pts',(3.48222119030037,-4.65981330997436,6.10138512702726));
#53421=CARTESIAN_POINT('Ctrl Pts',(5.8026935727219,0.410453167953449,6.37980898067441));
#53422=CARTESIAN_POINT('Ctrl Pts',(2.79160731206521,5.10359217779156,6.65823283432152));
#53423=CARTESIAN_POINT('Ctrl Pts',(-2.78442881302834,5.10751218179347,6.93665668796867));
#53424=CARTESIAN_POINT('Ctrl Pts',(-5.80211073277071,0.41861145070098,7.21508054161579));
#53425=CARTESIAN_POINT('Ctrl Pts',(-3.48876952718026,-4.65491264023392,
7.49350439526292));
#53426=CARTESIAN_POINT('Ctrl Pts',(2.03007944704129,-5.45146787027966,7.77192824891004));
#53427=CARTESIAN_POINT('Ctrl Pts',(5.68367610587452,-1.23917328308113,8.05035210255719));
#53428=CARTESIAN_POINT('Ctrl Pts',(4.11506826830211,4.1116830676992,8.32877595620429));
#53429=CARTESIAN_POINT('Ctrl Pts',(-1.23449534743867,5.68469398817063,8.60719980985145));
#53430=CARTESIAN_POINT('Ctrl Pts',(-5.4497953221667,2.03456517430157,8.88562366349855));
#53431=CARTESIAN_POINT('Ctrl Pts',(-4.6577822294781,-3.48493747501288,9.16404751714571));
#53432=CARTESIAN_POINT('Ctrl Pts',(0.413836324351832,-5.80245327414518,
9.44247137079281));
#53433=CARTESIAN_POINT('Ctrl Pts',(5.10521894046314,-2.78863121834486,9.72089522443996));
#53434=CARTESIAN_POINT('Ctrl Pts',(5.10588786891966,2.78740624452375,9.99931907808708));
#53435=CARTESIAN_POINT('Ctrl Pts',(0.415228493207719,5.80235381551483,10.2777429317342));
#53436=CARTESIAN_POINT('Ctrl Pts',(-4.6569459554733,3.48605491491343,10.5561667853813));
#53437=CARTESIAN_POINT('Ctrl Pts',(-5.45028331787931,-2.03325754808326,
10.8345906390285));
#53438=CARTESIAN_POINT('Ctrl Pts',(-1.23585923872538,-5.68439763247154,
11.1130144926756));
#53439=CARTESIAN_POINT('Ctrl Pts',(4.11408163504771,-4.11267027637206,11.3914383463227));
#53440=CARTESIAN_POINT('Ctrl Pts',(5.683973256732,1.23780956481465,11.6698621999699));
#53441=CARTESIAN_POINT('Ctrl Pts',(2.03138735756037,5.45098063705376,11.948286053617));
#53442=CARTESIAN_POINT('Ctrl Pts',(-3.48765257505427,4.65574956561328,12.2267099072641));
#53443=CARTESIAN_POINT('Ctrl Pts',(-5.80221100307997,-0.417219340070512,
12.5051337609113));
#53444=CARTESIAN_POINT('Ctrl Pts',(-2.78565417665601,-5.10684396766439,
12.7835576145584));
#53445=CARTESIAN_POINT('Ctrl Pts',(2.79038272846711,-5.10426182034811,13.0619814682055));
#53446=CARTESIAN_POINT('Ctrl Pts',(5.80259492580427,-0.411845394561442,
13.3404053218526));
#53447=CARTESIAN_POINT('Ctrl Pts',(3.48333911759557,4.65897768762844,13.6188291754998));
#53448=CARTESIAN_POINT('Ctrl Pts',(-2.03643495793874,5.4490969127073,13.8972530291469));
#53449=CARTESIAN_POINT('Ctrl Pts',(-5.68511722671199,1.2325447742511,14.175676882794));
#53450=CARTESIAN_POINT('Ctrl Pts',(-4.11027088637907,-4.11647880385354,
14.4541007364412));
#53451=CARTESIAN_POINT('Ctrl Pts',(1.2411233614091,-5.68325059308101,14.7325245900883));
#53452=CARTESIAN_POINT('Ctrl Pts',(5.45216409893207,-2.0282088502685,15.0109484437354));
#53453=CARTESIAN_POINT('Ctrl Pts',(4.65371531907096,3.49036648950155,15.2893722973825));
#53454=CARTESIAN_POINT('Ctrl Pts',(-0.420602213959508,5.80196675960862,
15.5677961510297));
#53455=CARTESIAN_POINT('Ctrl Pts',(-5.10846725884286,2.78267618801067,15.8462200046768));
#53456=CARTESIAN_POINT('Ctrl Pts',(-5.10263403663162,-2.79335826384653,
16.1246438583239));
#53457=CARTESIAN_POINT('Ctrl Pts',(-0.408462155912262,-5.8028340635571,
16.4030677119711));
#53458=CARTESIAN_POINT('Ctrl Pts',(4.66100783600869,-3.48062213614987,16.6814915656182));
#53459=CARTESIAN_POINT('Ctrl Pts',(5.4479086551669,2.03961167552763,16.9599154192653));
#53460=CARTESIAN_POINT('Ctrl Pts',(1.22922989078505,5.68583488835121,17.2383392729125));
#53461=CARTESIAN_POINT('Ctrl Pts',(-4.11887457330181,4.10787009913883,17.5167631265596));
#53462=CARTESIAN_POINT('Ctrl Pts',(-5.68252599746333,-1.24443673609558,
17.7951869802067));
#53463=CARTESIAN_POINT('Ctrl Pts',(-2.02502965350643,-5.45334570739934,
18.0736108338538));
#53464=CARTESIAN_POINT('Ctrl Pts',(3.49307921743211,-4.65167949054264,18.352034687501));
#53465=CARTESIAN_POINT('Ctrl Pts',(5.80172054381419,0.4239849448688,18.6304585411481));
#53466=CARTESIAN_POINT('Ctrl Pts',(2.77969725342115,5.11008881344677,18.9088823947953));
#53467=CARTESIAN_POINT('Ctrl Pts',(-2.79633284965052,5.10100451832347,19.1873062484423));
#53468=CARTESIAN_POINT('Ctrl Pts',(-5.803071228692,0.40507877841031,19.4657301020895));
#53469=CARTESIAN_POINT('Ctrl Pts',(-3.47790397149999,-4.66303639992394,
19.7441539557366));
#53470=CARTESIAN_POINT('Ctrl Pts',(2.04278769977008,-5.44671854566206,20.0225778093838));
#53471=CARTESIAN_POINT('Ctrl Pts',(5.68655061714523,-1.22591458945406,20.3010016630309));
#53472=CARTESIAN_POINT('Ctrl Pts',(4.10546791546748,4.12126894257805,20.579425516678));
#53473=CARTESIAN_POINT('Ctrl Pts',(-1.2477496877477,5.68179947012534,20.8578493703251));
#53474=CARTESIAN_POINT('Ctrl Pts',(-5.45452546205389,2.02184976835486,21.1362732239723));
#53475=CARTESIAN_POINT('Ctrl Pts',(-4.64964208072038,-3.49579075792379,
21.4146970776194));
#53476=CARTESIAN_POINT('Ctrl Pts',(0.427367531648445,-5.80147235578038,
21.6931209312665));
#53477=CARTESIAN_POINT('Ctrl Pts',(5.1117086309249,-2.77671737390015,21.9715447849137));
#53478=CARTESIAN_POINT('Ctrl Pts',(5.09937326597762,2.79930648486794,22.2499686385608));
#53479=CARTESIAN_POINT('Ctrl Pts',(0.401695263205706,5.80330642112832,22.5283924922079));
#53480=CARTESIAN_POINT('Ctrl Pts',(-4.66506337868458,3.47518462456994,22.8068163458551));
#53481=CARTESIAN_POINT('Ctrl Pts',(-5.44552658459737,-2.04596302958645,
23.0852401995022));
#53482=CARTESIAN_POINT('Ctrl Pts',(-1.222598871385,-5.68726441285079,23.3636640531493));
#53483=CARTESIAN_POINT('Ctrl Pts',(4.12366191086833,-4.10306433618151,23.6420879067964));
#53484=CARTESIAN_POINT('Ctrl Pts',(5.68107101131397,1.25106221523925,23.9205117604436));
#53485=CARTESIAN_POINT('Ctrl Pts',(2.01866919589476,5.45570336249478,24.1989356140907));
#53486=CARTESIAN_POINT('Ctrl Pts',(-3.49850111005493,4.64760309029668,24.4773594677378));
#53487=CARTESIAN_POINT('Ctrl Pts',(-5.80122219559149,-0.430749973148619,
24.755783321385));
#53488=CARTESIAN_POINT('Ctrl Pts',(-2.77373655046063,-5.11332671072659,
25.0342071750321));
#53489=CARTESIAN_POINT('Ctrl Pts',(2.80227916848797,-5.09774028014861,25.3126310286793));
#53490=CARTESIAN_POINT('Ctrl Pts',(5.80353964078615,-0.39831161144852,25.5910548823263));
#53491=CARTESIAN_POINT('Ctrl Pts',(3.47246409628408,4.66708877160151,25.8694787359735));
#53492=CARTESIAN_POINT('Ctrl Pts',(-2.04913766389717,5.44433277237802,26.1479025896206));
#53493=CARTESIAN_POINT('Ctrl Pts',(-5.68797627522524,1.21928273770528,26.4263264432677));
#53494=CARTESIAN_POINT('Ctrl Pts',(-4.10065936209809,-4.12605347735923,
26.7047502969149));
#53495=CARTESIAN_POINT('Ctrl Pts',(1.2543743174442,-5.68034062127683,26.983174150562));
#53496=CARTESIAN_POINT('Ctrl Pts',(5.45687940832144,-2.01548793720741,27.2615980042091));
#53497=CARTESIAN_POINT('Ctrl Pts',(4.64556251996484,3.50121027290405,27.5400218578563));
#53498=CARTESIAN_POINT('Ctrl Pts',(-0.434132268219488,5.80097006333265,
27.8184457115034));
#53499=CARTESIAN_POINT('Ctrl Pts',(-5.11494305230171,2.77075478411592,28.0968695651505));
#53500=CARTESIAN_POINT('Ctrl Pts',(-5.09610556139159,-2.8052508994999,28.3752934187976));
#53501=CARTESIAN_POINT('Ctrl Pts',(-0.394927824289227,-5.80377088758623,
28.6537172724448));
#53502=CARTESIAN_POINT('Ctrl Pts',(4.6691125779863,-3.46974238756726,28.9321411260919));
#53503=CARTESIAN_POINT('Ctrl Pts',(5.4431371094098,2.0523116016232,29.210564979739));
#53504=CARTESIAN_POINT('Ctrl Pts',(1.215966189542,5.68868620402655,29.4889888333862));
#53505=CARTESIAN_POINT('Ctrl Pts',(-4.12844364123772,4.09825299403475,29.7674126870333));
#53506=CARTESIAN_POINT('Ctrl Pts',(-5.67960830026223,-1.25768599323653,
30.0458365406804));
#53507=CARTESIAN_POINT('Ctrl Pts',(-2.01230599337432,-5.4580535991341,30.3242603943276));
#53508=CARTESIAN_POINT('Ctrl Pts',(3.50391824555016,-4.64352037041854,30.6026842479747));
#53509=CARTESIAN_POINT('Ctrl Pts',(5.80071595908955,0.437514415711182,30.8811081016218));
#53510=CARTESIAN_POINT('Ctrl Pts',(2.76777207587959,5.11655765510094,31.1595319552689));
#53511=CARTESIAN_POINT('Ctrl Pts',(-2.80822167689368,5.0944691102622,31.4379558089161));
#53512=CARTESIAN_POINT('Ctrl Pts',(-5.80400016144989,0.391543902877945,
31.7163796625632));
#53513=CARTESIAN_POINT('Ctrl Pts',(-3.46701949934472,-4.67113479715094,
31.9948035162103));
#53514=CARTESIAN_POINT('Ctrl Pts',(2.05548484168548,-5.44193959609919,32.2732273698575));
#53515=CARTESIAN_POINT('Ctrl Pts',(5.68939419901335,-1.21264922802275,32.5516512235046));
#53516=CARTESIAN_POINT('Ctrl Pts',(4.09584523280961,4.13083240169122,32.8300750771517));
#53517=CARTESIAN_POINT('Ctrl Pts',(-1.26099724149055,5.67887404851917,33.1084989307988));
#53518=CARTESIAN_POINT('Ctrl Pts',(-5.45922593453371,2.00912336547695,33.386922784446));
#53519=CARTESIAN_POINT('Ctrl Pts',(-4.64147664235183,-3.50662502707285,
33.6653466380932));
#53520=CARTESIAN_POINT('Ctrl Pts',(0.440896414474084,-5.80045988294852,
33.9437704917402));
#53521=CARTESIAN_POINT('Ctrl Pts',(5.11817051857534,-2.76478842676563,34.2221943453874));
#53522=CARTESIAN_POINT('Ctrl Pts',(5.09283092731677,2.81119149965931,34.5006181990345));
#53523=CARTESIAN_POINT('Ctrl Pts',(0.388159848365178,5.80422746229918,34.7790420526816));
#53524=CARTESIAN_POINT('Ctrl Pts',(-4.67315542840794,3.46429543254218,35.0574659063288));
#53525=CARTESIAN_POINT('Ctrl Pts',(-5.44074023285332,-2.05865738300537,
35.3358897599759));
#53526=CARTESIAN_POINT('Ctrl Pts',(-1.20933185427489,-5.69010025994507,
35.614313613623));
#53527=CARTESIAN_POINT('Ctrl Pts',(4.13321975790782,-4.09343607924097,35.8927374672701));
#53528=CARTESIAN_POINT('Ctrl Pts',(5.67813786629717,1.26430806108067,36.1711613209173));
#53529=CARTESIAN_POINT('Ctrl Pts',(2.00594005459731,5.46039641412169,36.4495851745644));
#53530=CARTESIAN_POINT('Ctrl Pts',(-3.50933061655186,4.63943133645954,36.7280090282115));
#53531=CARTESIAN_POINT('Ctrl Pts',(-5.80020183499662,-0.444278263358354,
37.0064328818587));
#53532=CARTESIAN_POINT('Ctrl Pts',(-2.76180383778841,-5.11978164217659,
37.2848567355058));
#53533=CARTESIAN_POINT('Ctrl Pts',(2.81416036678732,-5.09119101311223,37.5632805891529));
#53534=CARTESIAN_POINT('Ctrl Pts',(5.80445279005691,-0.384775661901064,
37.8417044428));
#53535=CARTESIAN_POINT('Ctrl Pts',(3.46157018808544,4.67517447107051,38.1201282964472));
#53536=CARTESIAN_POINT('Ctrl Pts',(-2.06182922450441,5.4395390200798,38.3985521500943));
#53537=CARTESIAN_POINT('Ctrl Pts',(-5.69080438658164,1.20601406942624,38.6769760037414));
#53538=CARTESIAN_POINT('Ctrl Pts',(-4.0910255341479,-4.13560570907586,38.9553998573886));
#53539=CARTESIAN_POINT('Ctrl Pts',(1.26761845088123,-5.6773997538465,39.2338237110357));
#53540=CARTESIAN_POINT('Ctrl Pts',(5.46156503750013,-2.00275606181767,39.5122475646828));
#53541=CARTESIAN_POINT('Ctrl Pts',(4.63738445343698,3.51203501306753,39.79067141833));
#53542=CARTESIAN_POINT('Ctrl Pts',(-0.447659961214595,5.79994181532161,
40.0690952719771));
#53543=CARTESIAN_POINT('Ctrl Pts',(-5.12139102535709,2.75881830996228,40.3475191256242));
#53544=CARTESIAN_POINT('Ctrl Pts',(-5.08954936820597,-2.81712827726845,
40.6259429792714));
#53545=CARTESIAN_POINT('Ctrl Pts',(-0.381391344636143,-5.80467614464644,
40.9043668329184));
#53546=CARTESIAN_POINT('Ctrl Pts',(4.67719192445218,-3.45884376690104,41.1827906865657));
#53547=CARTESIAN_POINT('Ctrl Pts',(5.43833595818706,2.06500036510422,41.4612145402126));
#53548=CARTESIAN_POINT('Ctrl Pts',(1.20269587460476,5.69150657868371,41.7396383938599));
#53549=CARTESIAN_POINT('Ctrl Pts',(-4.13799025438433,4.08861359834987,42.018062247507));
#53550=CARTESIAN_POINT('Ctrl Pts',(-5.67665971141812,-1.27092840976715,
42.2964861011541));
#53551=CARTESIAN_POINT('Ctrl Pts',(-1.99957138822013,-5.46273180427181,
42.5749099548013));
#53552=CARTESIAN_POINT('Ctrl Pts',(3.51473821570051,-4.6353359939799,42.8533338084484));
#53553=CARTESIAN_POINT('Ctrl Pts',(5.79967982401188,0.45104150689311,43.1317576620956));
#53554=CARTESIAN_POINT('Ctrl Pts',(2.75583184430228,5.12299866756965,43.4101815157427));
#53555=CARTESIAN_POINT('Ctrl Pts',(-2.82009523009366,5.08790599315611,43.6886053693897));
#53556=CARTESIAN_POINT('Ctrl Pts',(-5.80489752599187,0.378006897721008,
43.967029223037));
#53557=CARTESIAN_POINT('Ctrl Pts',(-3.45611616991583,-4.67920778786726,
44.245453076684));
#53558=CARTESIAN_POINT('Ctrl Pts',(2.06817080372702,-5.43713104758401,44.5238769303312));
#53559=CARTESIAN_POINT('Ctrl Pts',(5.69220683601255,-1.19937727093821,44.8023007839783));
#53560=CARTESIAN_POINT('Ctrl Pts',(4.08620027266672,4.14037339302263,45.0807246376255));
#53561=CARTESIAN_POINT('Ctrl Pts',(-1.27423793661312,5.67591773926357,45.3591484912725));
#53562=CARTESIAN_POINT('Ctrl Pts',(-5.46389671404001,1.99638603488747,45.6375723449197));
#53563=CARTESIAN_POINT('Ctrl Pts',(-4.63328595878473,-3.51744022353175,
45.9159961985668));
#53564=CARTESIAN_POINT('Ctrl Pts',(0.454422899244266,-5.79941586115651,
46.1944200522139));
#53565=CARTESIAN_POINT('Ctrl Pts',(5.12460456826788,-2.75284444182363,46.4728439058611));
#53566=CARTESIAN_POINT('Ctrl Pts',(5.08626088852126,2.82306122425459,46.7512677595082));
#53567=CARTESIAN_POINT('Ctrl Pts',(0.374622322305924,5.8051169340179,47.0296916131553));
#53568=CARTESIAN_POINT('Ctrl Pts',(-4.68122206063041,3.45338739805693,47.3081154668025));
#53569=CARTESIAN_POINT('Ctrl Pts',(-5.43592428868028,-2.07134053929494,
47.5865393204495));
#53570=CARTESIAN_POINT('Ctrl Pts',(-1.19605825955486,-5.69290515833011,
47.8649631740968));
#53571=CARTESIAN_POINT('Ctrl Pts',(4.14275512418048,-4.08378555791893,48.1433870277438));
#53572=CARTESIAN_POINT('Ctrl Pts',(5.67517383763514,1.27754703029398,48.421810881391));
#53573=CARTESIAN_POINT('Ctrl Pts',(1.99320000290249,5.46505976640885,48.7002347350381));
#53574=CARTESIAN_POINT('Ctrl Pts',(-3.52014103564295,4.63123434854828,48.9786585886852));
#53575=CARTESIAN_POINT('Ctrl Pts',(-5.79914992684515,-0.457804137118822,
49.2570824423324));
#53576=CARTESIAN_POINT('Ctrl Pts',(-2.7498561035418,-5.1262087269058,49.5355062959795));
#53577=CARTESIAN_POINT('Ctrl Pts',(2.82602625874287,-5.08461405486067,49.8139301496266));
#53578=CARTESIAN_POINT('Ctrl Pts',(5.80533436864992,-0.371237619541609,
50.0923540032738));
#53579=CARTESIAN_POINT('Ctrl Pts',(3.4506574522521,4.68323474205681,50.3707778569208));
#53580=CARTESIAN_POINT('Ctrl Pts',(-2.07450957073036,5.43471568188616,50.649201710568));
#53581=CARTESIAN_POINT('Ctrl Pts',(-5.69360154539906,1.19273884158297,50.9276255642152));
#53582=CARTESIAN_POINT('Ctrl Pts',(-4.08136945492725,-4.14513544704848,
51.2060494178623));
#53583=CARTESIAN_POINT('Ctrl Pts',(1.28085568968505,-5.67442800678559,51.4844732715094));
#53584=CARTESIAN_POINT('Ctrl Pts',(5.4662209609829,-1.99001329334819,51.7628971251566));
#53585=CARTESIAN_POINT('Ctrl Pts',(4.62918116396803,3.52284065111588,52.0413209788037));
#53586=CARTESIAN_POINT('Ctrl Pts',(-0.461185219367196,5.79888202116823,
52.3197448324508));
#53587=CARTESIAN_POINT('Ctrl Pts',(-5.12781114293802,2.74686683047278,52.5981686860979));
#53588=CARTESIAN_POINT('Ctrl Pts',(-5.08296549273427,-2.82899033255045,
52.8765925397451));
#53589=CARTESIAN_POINT('Ctrl Pts',(-0.367852790578618,-5.80554982981413,
53.1550163933922));
#53590=CARTESIAN_POINT('Ctrl Pts',(4.68524583146246,-3.4479263334292,53.4334402470393));
#53591=CARTESIAN_POINT('Ctrl Pts',(5.43350522761236,2.0776778969562,53.7118641006865));
#53592=CARTESIAN_POINT('Ctrl Pts',(1.18941901815086,5.69429599698262,53.9902879543335));
#53593=CARTESIAN_POINT('Ctrl Pts',(-4.14751436081733,4.07895196451306,54.2687118079807));
#53594=CARTESIAN_POINT('Ctrl Pts',(-5.67368024696851,-1.28416391366144,
54.5471356616279));
#53595=CARTESIAN_POINT('Ctrl Pts',(-1.98682590730801,-5.46738029736734,
54.8255595152749));
#53596=CARTESIAN_POINT('Ctrl Pts',(3.52553906903275,-4.627126405742,55.1039833689222));
#53597=CARTESIAN_POINT('Ctrl Pts',(5.7986121442169,0.464566144840059,55.3824072225692));
#53598=CARTESIAN_POINT('Ctrl Pts',(2.74387662363257,5.12941181581999,55.6608310762164));
#53599=CARTESIAN_POINT('Ctrl Pts',(-2.83195344466994,5.08131520270228,55.9392549298634));
#53600=CARTESIAN_POINT('Ctrl Pts',(-5.80576331743716,0.364467836567547,
56.2176787835106));
#53601=CARTESIAN_POINT('Ctrl Pts',(-3.44519404251673,-4.68725532816361,
56.4961026371577));
#53602=CARTESIAN_POINT('Ctrl Pts',(2.08084551689526,-5.43229292627044,56.7745264908049));
#53603=CARTESIAN_POINT('Ctrl Pts',(5.69498851284468,-1.18609879038724,57.052950344452));
#53604=CARTESIAN_POINT('Ctrl Pts',(4.07653308749828,4.14989186467828,57.3313741980992));
#53605=CARTESIAN_POINT('Ctrl Pts',(-1.2874717010986,5.67293055843817,57.6097980517462));
#53606=CARTESIAN_POINT('Ctrl Pts',(-5.46853777516823,1.98363784586525,57.8882219053935));
#53607=CARTESIAN_POINT('Ctrl Pts',(-4.62507007456854,-3.52823628847641,
58.1666457590405));
#53608=CARTESIAN_POINT('Ctrl Pts',(0.467946912388112,-5.79834029608278,
58.4450696126877));
#53609=CARTESIAN_POINT('Ctrl Pts',(5.13101074500744,-2.7408854840378,58.7234934663347));
#53610=CARTESIAN_POINT('Ctrl Pts',(5.07966318532585,2.83491559409379,59.001917319982));
#53611=CARTESIAN_POINT('Ctrl Pts',(0.361082758659297,5.80597483144648,59.2803411736289));
#53612=CARTESIAN_POINT('Ctrl Pts',(-4.68926323147709,3.44246058044367,59.5587650272763));
#53613=CARTESIAN_POINT('Ctrl Pts',(-5.43107877827254,-2.08401242947076,
59.8371888809232));
#53614=CARTESIAN_POINT('Ctrl Pts',(-1.18277815942064,-5.69567909274991,
60.1156127345705));
#53615=CARTESIAN_POINT('Ctrl Pts',(4.15226795782324,-4.07411282470503,60.3940365882174));
#53616=CARTESIAN_POINT('Ctrl Pts',(5.67217894144929,1.29077905087206,60.6724604418648));
#53617=CARTESIAN_POINT('Ctrl Pts',(1.98044911010386,5.469693393992,60.9508842955118));
#53618=CARTESIAN_POINT('Ctrl Pts',(-3.53093230852989,4.62301217114679,61.229308149159));
#53619=CARTESIAN_POINT('Ctrl Pts',(-5.79806647685838,-0.47132752086214,
61.507732002806));
#53620=CARTESIAN_POINT('Ctrl Pts',(-2.73789341270518,-5.13260792995689,
61.7861558564532));
#53621=CARTESIAN_POINT('Ctrl Pts',(2.83787677981535,-5.07800944116647,62.0645797101003));
#53622=CARTESIAN_POINT('Ctrl Pts',(5.80618437177022,-0.357697558004235,
62.3430035637474));
#53623=CARTESIAN_POINT('Ctrl Pts',(3.4397259481389,4.69126954072045,62.6214274173947));
#53624=CARTESIAN_POINT('Ctrl Pts',(-2.08717863360625,5.42986278403133,62.8998512710416));
#53625=CARTESIAN_POINT('Ctrl Pts',(-5.69636773646354,1.17945712637986,63.178275124689));
#53626=CARTESIAN_POINT('Ctrl Pts',(-4.07169117695603,-4.15464263944444,
63.4566989783358));
#53627=CARTESIAN_POINT('Ctrl Pts',(1.29408596185757,-5.67142539625746,63.7351228319832));
#53628=CARTESIAN_POINT('Ctrl Pts',(5.47084715344585,-1.97725970110767,64.0135466856302));
#53629=CARTESIAN_POINT('Ctrl Pts',(4.62095269617623,3.53362712827672,64.2919705392774));
#53630=CARTESIAN_POINT('Ctrl Pts',(-0.474707969112876,5.79779068663673,
64.5703943929245));
#53631=CARTESIAN_POINT('Ctrl Pts',(-5.1342033701254,2.73490041065189,64.8488182465717));
#53632=CARTESIAN_POINT('Ctrl Pts',(-5.07635397078635,-2.84083700082785,
65.1272421002188));
#53633=CARTESIAN_POINT('Ctrl Pts',(-0.354312235753313,-5.80639193833713,
65.4056659538659));
#53634=CARTESIAN_POINT('Ctrl Pts',(4.69327425521161,-3.4369901465322,65.684089807513));
#53635=CARTESIAN_POINT('Ctrl Pts',(5.42864494396021,2.09034412822534,65.9625136611601));
#53636=CARTESIAN_POINT('Ctrl Pts',(1.1761356923939,5.69705444375144,66.2409375148073));
#53637=CARTESIAN_POINT('Ctrl Pts',(-4.15701590873452,4.06926814507461,66.5193613684544));
#53638=CARTESIAN_POINT('Ctrl Pts',(-5.67066992311886,-1.29739243293082,
66.7977852221016));
#53639=CARTESIAN_POINT('Ctrl Pts',(-1.97406961996107,-5.47199905313755,
67.0762090757487));
#53640=CARTESIAN_POINT('Ctrl Pts',(3.53632074680071,-4.61889165035702,67.3546329293958));
#53641=CARTESIAN_POINT('Ctrl Pts',(5.79751292551162,0.478088255991047,67.633056783043));
#53642=CARTESIAN_POINT('Ctrl Pts',(2.73190647889548,5.13579706497058,67.91148063669));
#53643=CARTESIAN_POINT('Ctrl Pts',(-2.843796256125,5.07469677474826,68.1899044903372));
#53644=CARTESIAN_POINT('Ctrl Pts',(-5.80659753107665,0.350926793057335,
68.4683283439843));
#53645=CARTESIAN_POINT('Ctrl Pts',(-3.43425317655358,-4.69527737426908,
68.7467521976315));
#53646=CARTESIAN_POINT('Ctrl Pts',(2.09350891225194,-5.42742525847318,69.0251760512785));
#53647=CARTESIAN_POINT('Ctrl Pts',(5.69773921438019,-1.17281385859187,69.3035999049257));
#53648=CARTESIAN_POINT('Ctrl Pts',(4.06684372988438,4.15938776488691,69.5820237585728));
#53649=CARTESIAN_POINT('Ctrl Pts',(-1.30069846296805,5.66991252229023,69.8604476122199));
#53650=CARTESIAN_POINT('Ctrl Pts',(-5.47314909267551,1.97087886774828,70.1388714658671));
#53651=CARTESIAN_POINT('Ctrl Pts',(-4.61682903438977,-3.5390131631864,70.4172953195142));
#53652=CARTESIAN_POINT('Ctrl Pts',(0.481468380347833,-5.79723319357744,
70.6957191731614));
#53653=CARTESIAN_POINT('Ctrl Pts',(5.13738901395058,-2.72891161845354,70.9741430268085));
#53654=CARTESIAN_POINT('Ctrl Pts',(5.07303785361562,2.84675454470068,71.2525668804556));
#53655=CARTESIAN_POINT('Ctrl Pts',(0.347541231067252,5.80680114991893,71.5309907341027));
#53656=CARTESIAN_POINT('Ctrl Pts',(-4.69727889721183,3.43151503913349,71.8094145877499));
#53657=CARTESIAN_POINT('Ctrl Pts',(-5.42620372798489,-2.09667298461008,
72.087838441397));
#53658=CARTESIAN_POINT('Ctrl Pts',(-1.16949162610311,-5.69842204811702,
72.3662622950442));
#53659=CARTESIAN_POINT('Ctrl Pts',(4.16175820709524,-4.06441793220953,72.6446861486912));
#53660=CARTESIAN_POINT('Ctrl Pts',(5.66915319402907,1.30400405084528,72.9231100023384));
#53661=CARTESIAN_POINT('Ctrl Pts',(1.96768744555408,5.47429727166879,73.2015338559855));
#53662=CARTESIAN_POINT('Ctrl Pts',(-3.54170437651841,4.61476484897565,73.4799577096326));
#53663=CARTESIAN_POINT('Ctrl Pts',(-5.7969514909293,-0.484848341034039,
73.7583815632798));
#53664=CARTESIAN_POINT('Ctrl Pts',(-2.72591583034415,-5.13897921652443,
74.0368054169269));
#53665=CARTESIAN_POINT('Ctrl Pts',(2.84971186554951,-5.07137720795222,74.315229270574));
#53666=CARTESIAN_POINT('Ctrl Pts',(5.80700279479466,-0.344155550933751,
74.5936531242212));
#53667=CARTESIAN_POINT('Ctrl Pts',(3.42877573520264,4.69927882335965,74.8720769778683));
#53668=CARTESIAN_POINT('Ctrl Pts',(-2.09983634422443,5.42498035291051,75.1505008315154));
#53669=CARTESIAN_POINT('Ctrl Pts',(-5.6991029447297,1.16616899605683,75.4289246851625));
#53670=CARTESIAN_POINT('Ctrl Pts',(-4.06199075287477,-4.16412723455357,
75.7073485388097));
#53671=CARTESIAN_POINT('Ctrl Pts',(1.30730919543873,-5.66839193859359,75.9857723924568));
#53672=CARTESIAN_POINT('Ctrl Pts',(5.475443589727,-1.96449535446343,76.264196246104));
#53673=CARTESIAN_POINT('Ctrl Pts',(4.61269909481645,3.54439438588181,76.542620099751));
#53674=CARTESIAN_POINT('Ctrl Pts',(-0.488228136900599,5.79666781766301,
76.8210439533983));
#53675=CARTESIAN_POINT('Ctrl Pts',(-5.14056767215146,2.72291911558574,77.0994678070453));
#53676=CARTESIAN_POINT('Ctrl Pts',(-5.06971483832266,-2.85266821766606,
77.3778916606925));
#53677=CARTESIAN_POINT('Ctrl Pts',(-0.340769753807865,-5.80720246563535,
77.6563155143396));
#53678=CARTESIAN_POINT('Ctrl Pts',(4.70127715203259,-3.42603526569229,77.9347393679867));
#53679=CARTESIAN_POINT('Ctrl Pts',(5.42375513366596,2.1029989900195,78.2131632216339));
#53680=CARTESIAN_POINT('Ctrl Pts',(1.16284596958247,5.69978190398691,78.4915870752809));
#53681=CARTESIAN_POINT('Ctrl Pts',(-4.16649484645678,4.05956219270503,78.7700109289282));
#53682=CARTESIAN_POINT('Ctrl Pts',(-5.66762875624243,-1.31061389562501,
79.0484347825752));
#53683=CARTESIAN_POINT('Ctrl Pts',(-1.96130259556129,-5.47658804646063,
79.3268586362224));
#53684=CARTESIAN_POINT('Ctrl Pts',(3.54708319036234,-4.61063177261423,79.6052824898694));
#53685=CARTESIAN_POINT('Ctrl Pts',(5.79638217387485,0.491607766798655,79.8837063435167));
#53686=CARTESIAN_POINT('Ctrl Pts',(2.71992147519714,5.14215438029163,80.1621301971638));
#53687=CARTESIAN_POINT('Ctrl Pts',(-2.85562360004527,5.06805074529212,80.4405540508108));
#53688=CARTESIAN_POINT('Ctrl Pts',(-5.80740016237305,0.33738384084066,80.7189779044581));
#53689=CARTESIAN_POINT('Ctrl Pts',(-3.42329363153413,-4.70327388255127,
80.997401758105));
#53690=CARTESIAN_POINT('Ctrl Pts',(2.10616092092011,-5.42252807066782,81.2758256117524));
#53691=CARTESIAN_POINT('Ctrl Pts',(5.7004589256578,-1.15952254780973,81.5542494653993));
#53692=CARTESIAN_POINT('Ctrl Pts',(4.05713225252595,4.16886104199992,81.8326733190467));
#53693=CARTESIAN_POINT('Ctrl Pts',(-1.31391815028062,5.6668636472351,82.1110971726936));
#53694=CARTESIAN_POINT('Ctrl Pts',(-5.47773064148054,1.95810916993311,82.3895210263409));
#53695=CARTESIAN_POINT('Ctrl Pts',(-4.60856288307185,-3.54977078904587,
82.6679448799879));
#53696=CARTESIAN_POINT('Ctrl Pts',(0.494987229579467,-5.79609455966206,
82.946368733635));
#53697=CARTESIAN_POINT('Ctrl Pts',(5.14373934040566,-2.71692291019715,83.2247925872822));
#53698=CARTESIAN_POINT('Ctrl Pts',(5.06638492942612,2.85857801168262,83.5032164409293));
#53699=CARTESIAN_POINT('Ctrl Pts',(0.333997813182944,5.80759588494068,83.7816402945764));
#53700=CARTESIAN_POINT('Ctrl Pts',(-4.70526901423705,3.42055083365993,84.0600641482237));
#53701=CARTESIAN_POINT('Ctrl Pts',(-5.42129916433304,-2.10932213585141,
84.3384880018706));
#53702=CARTESIAN_POINT('Ctrl Pts',(-1.15619873186854,-5.70113400951219,
84.6169118555179));
#53703=CARTESIAN_POINT('Ctrl Pts',(4.1712258203786,-4.05470093316368,84.8953357091649));
#53704=CARTESIAN_POINT('Ctrl Pts',(5.66609661183164,1.31722195828223,85.1737595628121));
#53705=CARTESIAN_POINT('Ctrl Pts',(1.95491507866457,5.47887137439827,85.4521834164592));
#53706=CARTESIAN_POINT('Ctrl Pts',(-3.55245718101874,4.60649242689272,85.7306072701064));
#53707=CARTESIAN_POINT('Ctrl Pts',(-5.79580497512237,-0.498366524094111,
86.0090311237535));
#53708=CARTESIAN_POINT('Ctrl Pts',(-2.71392342160519,-5.14532255195471,
86.2874549774007));
#53709=CARTESIAN_POINT('Ctrl Pts',(2.86153145157372,-5.06471739129104,86.5658788310476));
#53710=CARTESIAN_POINT('Ctrl Pts',(5.80778963327165,-0.330611671985869,
86.844302684695));
#53711=CARTESIAN_POINT('Ctrl Pts',(3.4178068730022,4.70726254641164,87.1227265383419));
#53712=CARTESIAN_POINT('Ctrl Pts',(-2.11248263373895,5.42006841507948,87.4011503919893));
#53713=CARTESIAN_POINT('Ctrl Pts',(-5.70180715532063,1.15287452288852,87.6795742456361));
#53714=CARTESIAN_POINT('Ctrl Pts',(-4.05226823544451,-4.173589180789,87.9579980992835));
#53715=CARTESIAN_POINT('Ctrl Pts',(1.32052531850694,-5.66532765029288,88.2364219529305));
#53716=CARTESIAN_POINT('Ctrl Pts',(5.48001024482615,-1.95172032284121,88.5148458065777));
#53717=CARTESIAN_POINT('Ctrl Pts',(4.60442040478046,3.5551423653677,88.7932696602248));
#53718=CARTESIAN_POINT('Ctrl Pts',(-0.501745649193681,5.79551342035425,
89.071693513872));
#53719=CARTESIAN_POINT('Ctrl Pts',(-5.14690401440058,2.71092301044105,89.3501173675189));
#53720=CARTESIAN_POINT('Ctrl Pts',(-5.06304813145374,-2.86448391871446,
89.6285412211663));
#53721=CARTESIAN_POINT('Ctrl Pts',(-0.327225418400649,-5.80798140730008,
89.9069650748132));
#53722=CARTESIAN_POINT('Ctrl Pts',(4.70925447839735,-3.41506175049384,90.1853889284604));
#53723=CARTESIAN_POINT('Ctrl Pts',(5.41883582332552,2.11564241350824,90.4638127821077));
#53724=CARTESIAN_POINT('Ctrl Pts',(1.14954992199983,5.70247836285427,90.7422366357546));
#53725=CARTESIAN_POINT('Ctrl Pts',(-4.17595112242768,4.04983416019552,91.0206604894019));
#53726=CARTESIAN_POINT('Ctrl Pts',(-5.66455676288018,-1.3238282298317,91.2990843430488));
#53727=CARTESIAN_POINT('Ctrl Pts',(-1.94852490354921,-5.48114725237695,
91.5775081966962));
#53728=CARTESIAN_POINT('Ctrl Pts',(3.55782634118013,-4.60234681743952,91.8559320503431));
#53729=CARTESIAN_POINT('Ctrl Pts',(5.79521989545676,0.505124603729757,92.1343559039904));
#53730=CARTESIAN_POINT('Ctrl Pts',(2.70792167772444,5.14848372720567,92.4127797576374));
#53731=CARTESIAN_POINT('Ctrl Pts',(-2.86743541210141,5.06137715048165,92.6912036112847));
#53732=CARTESIAN_POINT('Ctrl Pts',(-5.8081712069608,0.323839053578139,92.9696274649316));
#53733=CARTESIAN_POINT('Ctrl Pts',(-3.41231546706785,-4.71124480951695,
93.2480513185789));
#53734=CARTESIAN_POINT('Ctrl Pts',(2.11880147408499,-5.4176013894902,93.526475172226));
#53735=CARTESIAN_POINT('Ctrl Pts',(5.70314763188498,-1.14622493033275,93.8048990258731));
#53736=CARTESIAN_POINT('Ctrl Pts',(4.04739870824418,4.17831164449162,94.0833228795204));
#53737=CARTESIAN_POINT('Ctrl Pts',(-1.32713069113358,5.66378394985563,94.3617467331672));
#53738=CARTESIAN_POINT('Ctrl Pts',(-5.48228239666421,1.94532882187493,94.6401705868147));
#53739=CARTESIAN_POINT('Ctrl Pts',(-4.6002716655748,-3.56050910754356,94.9185944404615));
#53740=CARTESIAN_POINT('Ctrl Pts',(0.508503386553553,-5.7949244005297,95.1970182941089));
#53741=CARTESIAN_POINT('Ctrl Pts',(5.15006168983296,-2.70491942447578,95.4754421477558));
#53742=CARTESIAN_POINT('Ctrl Pts',(5.05970444894282,2.87038593073113,95.7538660014031));
#53743=CARTESIAN_POINT('Ctrl Pts',(0.320452578669648,5.80835903218928,96.0322898550501));
#53744=CARTESIAN_POINT('Ctrl Pts',(-4.71323353909406,3.40956802365781,96.3107137086973));
#53745=CARTESIAN_POINT('Ctrl Pts',(-5.41636511399308,-2.12195981439559,
96.5891375623444));
#53746=CARTESIAN_POINT('Ctrl Pts',(-1.14289954901735,-5.70381496218517,
96.8675614159915));
#53747=CARTESIAN_POINT('Ctrl Pts',(4.18067074617859,-4.04496188041834,97.1459852696388));
#53748=CARTESIAN_POINT('Ctrl Pts',(5.66300921148187,1.33043270129022,97.4244091232857));
#53749=CARTESIAN_POINT('Ctrl Pts',(1.94213207890468,5.4834156773019,97.702832976933));
#53750=CARTESIAN_POINT('Ctrl Pts',(-3.56319066354585,4.59819494989182,97.9812568305801));
#53751=CARTESIAN_POINT('Ctrl Pts',(-5.79462693567359,-0.511881996516395,
98.2596806842271));
#53752=CARTESIAN_POINT('Ctrl Pts',(-2.70191625171569,-5.15163790174596,
98.5381045378744));
#53753=CARTESIAN_POINT('Ctrl Pts',(2.87333547360048,-5.05803002740593,98.8165283915213));
#53754=CARTESIAN_POINT('Ctrl Pts',(5.80854488292173,-0.31706599482648,99.0949522451687));
#53755=CARTESIAN_POINT('Ctrl Pts',(3.40681942119772,4.71522066645252,99.3733760988158));
#53756=CARTESIAN_POINT('Ctrl Pts',(-2.12511743336623,5.41512699725444,99.6517999524627));
#53757=CARTESIAN_POINT('Ctrl Pts',(-5.70448035352804,1.1395737791842,99.9302238061101));
#53758=CARTESIAN_POINT('Ctrl Pts',(-4.0425236775464,-4.18302842668654,100.208647659757));
#53759=CARTESIAN_POINT('Ctrl Pts',(1.33373425917899,-5.66223254802231,100.487071513404));
#53760=CARTESIAN_POINT('Ctrl Pts',(5.48454709390498,-1.93893467572513,100.765495367051));
#53761=CARTESIAN_POINT('Ctrl Pts',(4.59611667109638,3.56587100827567,101.043919220699));
#53762=CARTESIAN_POINT('Ctrl Pts',(-0.515260432469941,5.79432750098943,
101.322343074346));
#53763=CARTESIAN_POINT('Ctrl Pts',(-5.15321236240903,2.69891216046496,101.600766927993));
#53764=CARTESIAN_POINT('Ctrl Pts',(-5.05635388644005,-2.87628403970705,
101.87919078164));
#53765=CARTESIAN_POINT('Ctrl Pts',(-0.313679303199746,-5.8087287590948,
102.157614635287));
#53766=CARTESIAN_POINT('Ctrl Pts',(4.71720619091674,-3.40406966062208,102.436038488934));
#53767=CARTESIAN_POINT('Ctrl Pts',(5.41388703969527,2.12827432992347,102.714462342581));
#53768=CARTESIAN_POINT('Ctrl Pts',(1.13624762196393,5.70514380568731,102.992886196228));
#53769=CARTESIAN_POINT('Ctrl Pts',(-4.1853846852139,4.0400841004573,103.271310049876));
#53770=CARTESIAN_POINT('Ctrl Pts',(-5.66145395974103,-1.33703536367746,
103.549733903523));
#53771=CARTESIAN_POINT('Ctrl Pts',(-1.93573661342329,-5.48567664608875,
103.82815775717));
#53772=CARTESIAN_POINT('Ctrl Pts',(3.56855014082175,-4.59403682989503,104.106581610817));
#53773=CARTESIAN_POINT('Ctrl Pts',(5.79402609657907,0.518638693265626,104.385005464464));
#53774=CARTESIAN_POINT('Ctrl Pts',(2.69590715174485,5.15478507128686,104.663429318111));
#53775=CARTESIAN_POINT('Ctrl Pts',(-2.87923162804837,5.05467602661504,104.941853171758));
#53776=CARTESIAN_POINT('Ctrl Pts',(-5.80891066064616,0.310292504940642,
105.220277025406));
#53777=CARTESIAN_POINT('Ctrl Pts',(-3.4013187428654,-4.71919011181193,105.498700879052));
#53778=CARTESIAN_POINT('Ctrl Pts',(2.13143050299427,-5.4126452417369,105.7771247327));
#53779=CARTESIAN_POINT('Ctrl Pts',(5.70580531843759,-1.13292107848706,106.055548586347));
#53780=CARTESIAN_POINT('Ctrl Pts',(4.03764314998017,4.18773952095986,106.333972439994));
#53781=CARTESIAN_POINT('Ctrl Pts',(-1.34033601366353,5.66067344690254,106.612396293641));
#53782=CARTESIAN_POINT('Ctrl Pts',(-5.48680433346917,1.93253789308644,106.890820147288));
#53783=CARTESIAN_POINT('Ctrl Pts',(-4.59195542699491,-3.57122806027332,
107.169244000935));
#53784=CARTESIAN_POINT('Ctrl Pts',(0.522016777754955,-5.79372272254491,
107.447667854582));
#53785=CARTESIAN_POINT('Ctrl Pts',(5.15635602784475,-2.69290122657703,107.72609170823));
#53786=CARTESIAN_POINT('Ctrl Pts',(5.05299644850137,2.88217823762239,108.004515561877));
#53787=CARTESIAN_POINT('Ctrl Pts',(0.306905601200556,5.8090905875139,108.282939415524));
#53788=CARTESIAN_POINT('Ctrl Pts',(-4.72117242846357,3.39856666886297,108.561363269171));
#53789=CARTESIAN_POINT('Ctrl Pts',(-5.41140160380157,-2.13458595150567,
108.839787122818));
#53790=CARTESIAN_POINT('Ctrl Pts',(-1.1295941498845,-5.70646489155393,109.118210976465));
#53791=CARTESIAN_POINT('Ctrl Pts',(4.19009293312384,-4.03520082694487,109.396634830112));
#53792=CARTESIAN_POINT('Ctrl Pts',(5.65989100977229,1.34363620801531,109.675058683759));
#53793=CARTESIAN_POINT('Ctrl Pts',(1.92933851580168,5.48793015566298,109.953482537407));
#53794=CARTESIAN_POINT('Ctrl Pts',(-3.5739047657201,4.58987246310338,110.231906391054));
#53795=CARTESIAN_POINT('Ctrl Pts',(-5.79341737899019,-0.525394684789773,
110.510330244701));
#53796=CARTESIAN_POINT('Ctrl Pts',(-2.68989438598306,-5.1579252315488,110.788754098348));
#53797=CARTESIAN_POINT('Ctrl Pts',(2.88512386742743,-5.05131515266979,111.067177951995));
#53798=CARTESIAN_POINT('Ctrl Pts',(5.80926853963687,-0.303518593130995,
111.345601805642));
#53799=CARTESIAN_POINT('Ctrl Pts',(3.39581343955041,4.72315314019781,111.62402565929));
#53800=CARTESIAN_POINT('Ctrl Pts',(-2.13774067438488,5.41015612631201,111.902449512937));
#53801=CARTESIAN_POINT('Ctrl Pts',(-5.70712252481211,1.12626683728736,112.180873366584));
#53802=CARTESIAN_POINT('Ctrl Pts',(-4.03275713218176,-4.19244492090577,
112.459297220231));
#53803=CARTESIAN_POINT('Ctrl Pts',(1.34693594561081,-5.65910664861623,112.737721073878));
#53804=CARTESIAN_POINT('Ctrl Pts',(5.48905411228744,-1.92613848265676,113.016144927525));
#53805=CARTESIAN_POINT('Ctrl Pts',(4.58778793892862,3.57658025625215,113.294568781172));
#53806=CARTESIAN_POINT('Ctrl Pts',(-0.528772413221697,5.79311006601865,
113.572992634819));
#53807=CARTESIAN_POINT('Ctrl Pts',(-5.1594926818655,2.68688663098524,113.851416488466));
#53808=CARTESIAN_POINT('Ctrl Pts',(-5.04963213969196,-2.88806851646232,
114.129840342114));
#53809=CARTESIAN_POINT('Ctrl Pts',(-0.300131481883046,-5.80944451695458,
114.408264195761));
#53810=CARTESIAN_POINT('Ctrl Pts',(4.72513224634132,-3.39305905586345,114.686688049408));
#53811=CARTESIAN_POINT('Ctrl Pts',(5.40890880969165,2.14089467055971,114.965111903055));
#53812=CARTESIAN_POINT('Ctrl Pts',(1.12293914182643,5.70777821798859,115.243535756702));
#53813=CARTESIAN_POINT('Ctrl Pts',(-4.19479548350608,4.03031206652138,115.521959610349));
#53814=CARTESIAN_POINT('Ctrl Pts',(-5.65832036370105,-1.3502352253282,115.800383463996));
#53815=CARTESIAN_POINT('Ctrl Pts',(-1.92293779473958,-5.49017620296048,
116.078807317644));
#53816=CARTESIAN_POINT('Ctrl Pts',(3.57925453095985,-4.58570185517924,116.35723117129));
#53817=CARTESIAN_POINT('Ctrl Pts',(5.79280078373477,0.532149961902354,116.635655024938));
#53818=CARTESIAN_POINT('Ctrl Pts',(2.68387796260612,5.16105837826204,116.914078878585));
#53819=CARTESIAN_POINT('Ctrl Pts',(-2.89101218372597,5.04794741013998,117.192502732232));
#53820=CARTESIAN_POINT('Ctrl Pts',(-5.80961851940719,0.296744268608284,
117.470926585879));
#53821=CARTESIAN_POINT('Ctrl Pts',(-3.39030351873854,-4.72710974622134,
117.749350439526));
#53822=CARTESIAN_POINT('Ctrl Pts',(2.14404793895791,-5.40765965436446,118.027774293173));
#53823=CARTESIAN_POINT('Ctrl Pts',(5.70843197086043,-1.11961106463314,118.306198146821));
#53824=CARTESIAN_POINT('Ctrl Pts',(4.02786563079502,4.19714462012598,118.584622000468));
#53825=CARTESIAN_POINT('Ctrl Pts',(-1.35353404604633,5.65753215529382,118.863045854115));
#53826=CARTESIAN_POINT('Ctrl Pts',(-5.49129642730031,1.91973645313823,119.141469707762));
#53827=CARTESIAN_POINT('Ctrl Pts',(-4.58361421256499,-3.58192758893474,
119.419893561409));
#53828=CARTESIAN_POINT('Ctrl Pts',(0.535527329685027,-5.79248953224288,
119.698317415056));
#53829=CARTESIAN_POINT('Ctrl Pts',(5.16262232020387,-2.68086838186981,119.976741268703));
#53830=CARTESIAN_POINT('Ctrl Pts',(5.04626096459074,2.89395486822036,120.25516512235));
#53831=CARTESIAN_POINT('Ctrl Pts',(0.29335695445051,5.80979054693031,120.533588975998));
#53832=CARTESIAN_POINT('Ctrl Pts',(-4.72908563915093,3.38754682912243,120.812012829645));
#53833=CARTESIAN_POINT('Ctrl Pts',(-5.40640866078271,-2.14720047852628,
121.090436683292));
#53834=CARTESIAN_POINT('Ctrl Pts',(-1.11628260678685,-5.7090837831698,121.368860536939));
#53835=CARTESIAN_POINT('Ctrl Pts',(4.19949232986848,-4.02541782590159,121.647284390586));
#53836=CARTESIAN_POINT('Ctrl Pts',(5.65674202384814,1.35683240677064,121.925708244233));
#53837=CARTESIAN_POINT('Ctrl Pts',(1.9165344585906,5.49241478468641,122.20413209788));
#53838=CARTESIAN_POINT('Ctrl Pts',(-3.58459942860632,4.58152501224816,122.482555951528));
#53839=CARTESIAN_POINT('Ctrl Pts',(-5.79217631289823,-0.538904516276096,
122.760979805174));
#53840=CARTESIAN_POINT('Ctrl Pts',(-2.67785788744019,-5.1641845055458,123.039403658822));
#53841=CARTESIAN_POINT('Ctrl Pts',(2.89689656449083,-5.04457280666451,123.317827512469));
#53842=CARTESIAN_POINT('Ctrl Pts',(5.80996060787651,-0.289969534807391,
123.596251366116));
#53843=CARTESIAN_POINT('Ctrl Pts',(3.3847889720702,4.73105991359457,123.874675219763));
#53844=CARTESIAN_POINT('Ctrl Pts',(-2.15035225820507,5.40515584988507,124.15309907341));
#53845=CARTESIAN_POINT('Ctrl Pts',(-5.70973371131906,1.11295373068523,124.431522927057));
#53846=CARTESIAN_POINT('Ctrl Pts',(-4.02296854575556,-4.20183853879829,
124.709946780705));
#53847=CARTESIAN_POINT('Ctrl Pts',(1.36013010449734,-5.65595010773044,124.988370634352));
#53848=CARTESIAN_POINT('Ctrl Pts',(5.49353165593364,-1.91333155142861,125.266794487999));
#53849=CARTESIAN_POINT('Ctrl Pts',(4.57943353516515,3.58726955670461,125.545218341646));
#53850=CARTESIAN_POINT('Ctrl Pts',(-0.542280161447921,5.79186205548623,
125.823642195293));
#53851=CARTESIAN_POINT('Ctrl Pts',(-5.16574749997522,2.67484472491793,126.10206604894));
#53852=CARTESIAN_POINT('Ctrl Pts',(-5.04287809139271,-2.89983395694199,
126.380489902587));
#53853=CARTESIAN_POINT('Ctrl Pts',(-0.286591160200441,-5.81013496081811,
126.658913756234));
#53854=CARTESIAN_POINT('Ctrl Pts',(4.73304984475302,-3.38201813095182,126.937337609882));
#53855=CARTESIAN_POINT('Ctrl Pts',(5.40386860173048,2.15348096294236,127.215761463529));
#53856=CARTESIAN_POINT('Ctrl Pts',(1.10968603140598,5.71042388849744,127.494185317176));
#53857=CARTESIAN_POINT('Ctrl Pts',(-4.2042995484988,4.02043823411284,127.772609170823));
#53858=CARTESIAN_POINT('Ctrl Pts',(-5.65493680070571,-1.36327691301718,
128.05103302447));
#53859=CARTESIAN_POINT('Ctrl Pts',(-1.91054242683083,-5.49493073827346,
128.329456878117));
#53860=CARTESIAN_POINT('Ctrl Pts',(3.59072126358126,-4.5768037590934,128.607880731764));
#53861=CARTESIAN_POINT('Ctrl Pts',(5.79006558455199,0.54463932997096,128.886304585412));
#53862=CARTESIAN_POINT('Ctrl Pts',(2.67464333335573,5.16925071277719,129.164728439058));
#53863=CARTESIAN_POINT('Ctrl Pts',(-2.90822559480448,5.03732645866885,129.443152292706));
#53864=CARTESIAN_POINT('Ctrl Pts',(-5.31707737445595,1.08293508440448,129.675172170745));
#53865=CARTESIAN_POINT('Ctrl Pts',(-4.603565324725,-2.23746205360027,129.860788073176));
#53866=CARTESIAN_POINT('Ctrl Pts',(-3.52404725972245,-3.52728314116456,
129.953596024392));
#53867=CARTESIAN_POINT('Ctrl Pts',(-2.85706463458608,-4.00329423553871,
130.));
#53868=CARTESIAN_POINT('Ctrl Pts',(-3.72756542462615,-3.69853108392275,
-9.85503696991097));
#53869=CARTESIAN_POINT('Ctrl Pts',(-3.11135891409689,-4.31957496079135,
-9.80863299430312));
#53870=CARTESIAN_POINT('Ctrl Pts',(-1.56670996892205,-5.23549382352855,
-9.7158250430874));
#53871=CARTESIAN_POINT('Ctrl Pts',(2.05477896642027,-5.41681918703043,-9.53020914065599));
#53872=CARTESIAN_POINT('Ctrl Pts',(5.80782888043916,-2.19899779207675,-9.2981892626167));
#53873=CARTESIAN_POINT('Ctrl Pts',(4.98754376236452,3.70664924546102,-9.01976540896959));
#53874=CARTESIAN_POINT('Ctrl Pts',(-0.420986833893069,6.19489822788983,
-8.74134155532244));
#53875=CARTESIAN_POINT('Ctrl Pts',(-5.43982339639458,2.99731266347737,-8.46291770167533));
#53876=CARTESIAN_POINT('Ctrl Pts',(-5.46202586547939,-2.9574351526511,-8.18449384802818));
#53877=CARTESIAN_POINT('Ctrl Pts',(-0.46487608052925,-6.1931715401536,-7.90606999438107));
#53878=CARTESIAN_POINT('Ctrl Pts',(4.95898097978158,-3.73947408110051,-7.62764614073393));
#53879=CARTESIAN_POINT('Ctrl Pts',(5.82671362163038,2.15055641831008,-7.34922228708681));
#53880=CARTESIAN_POINT('Ctrl Pts',(1.34069880457724,6.06438734465265,-7.07079843343967));
#53881=CARTESIAN_POINT('Ctrl Pts',(-4.37709716160729,4.40634693213311,-6.79237457979254));
#53882=CARTESIAN_POINT('Ctrl Pts',(-6.07321660587955,-1.30034900384963,
-6.51395072614541));
#53883=CARTESIAN_POINT('Ctrl Pts',(-2.18920112420409,-5.81223701358888,
-6.23552687249829));
#53884=CARTESIAN_POINT('Ctrl Pts',(3.70625950796275,-4.98381762778274,-5.95710301885116));
#53885=CARTESIAN_POINT('Ctrl Pts',(6.19638589441884,0.423781507110357,-5.67867916520402));
#53886=CARTESIAN_POINT('Ctrl Pts',(2.99322353569123,5.44200143254548,-5.4002553115569));
#53887=CARTESIAN_POINT('Ctrl Pts',(-2.96013380442341,5.46007232122862,-5.12183145790976));
#53888=CARTESIAN_POINT('Ctrl Pts',(-6.19369860373471,0.461385997955999,
-4.84340760426264));
#53889=CARTESIAN_POINT('Ctrl Pts',(-3.73644599677842,-4.9612244356498,-4.5649837506155));
#53890=CARTESIAN_POINT('Ctrl Pts',(2.15388118151106,-5.82542485685804,-4.28655989696838));
#53891=CARTESIAN_POINT('Ctrl Pts',(6.06520618595503,-1.3371807278235,-4.00813604332125));
#53892=CARTESIAN_POINT('Ctrl Pts',(4.40377391935758,4.3796750218653,-3.72971218967412));
#53893=CARTESIAN_POINT('Ctrl Pts',(-1.30387902554989,6.0724523764339,-3.45128833602699));
#53894=CARTESIAN_POINT('Ctrl Pts',(-5.81351809866303,2.1858146289845,-3.17286448237986));
#53895=CARTESIAN_POINT('Ctrl Pts',(-4.98165286397166,-3.70916607600341,
-2.89444062873273));
#53896=CARTESIAN_POINT('Ctrl Pts',(0.427392610277646,-6.19613700979456,
-2.6160167750856));
#53897=CARTESIAN_POINT('Ctrl Pts',(5.44374653141498,-2.99005049639645,-2.33759292143847));
#53898=CARTESIAN_POINT('Ctrl Pts',(5.45834505844533,2.96331697399165,-2.05916906779134));
#53899=CARTESIAN_POINT('Ctrl Pts',(0.45777495652505,6.1939664482386,-1.78074521414421));
#53900=CARTESIAN_POINT('Ctrl Pts',(-4.96340223028426,3.73355280798775,-1.50232136049708));
#53901=CARTESIAN_POINT('Ctrl Pts',(-5.82416799274277,-2.15727732608879,
-1.22389750684995));
#53902=CARTESIAN_POINT('Ctrl Pts',(-1.33364425305754,-6.06598477385677,
-0.945473653202821));
#53903=CARTESIAN_POINT('Ctrl Pts',(4.38224189037673,-4.40121963597495,-0.667049799555694));
#53904=CARTESIAN_POINT('Ctrl Pts',(6.07169111549865,1.30741931599734,-0.388625945908561));
#53905=CARTESIAN_POINT('Ctrl Pts',(2.18242472533663,5.81479153437582,-0.110202092261436));
#53906=CARTESIAN_POINT('Ctrl Pts',(-3.71206997155193,4.97948941119768,0.1682217613857));
#53907=CARTESIAN_POINT('Ctrl Pts',(-6.19588676643994,-0.431005159353265,
0.446645615032825));
#53908=CARTESIAN_POINT('Ctrl Pts',(-2.98687604473746,-5.445488937031,0.725069468679958));
#53909=CARTESIAN_POINT('Ctrl Pts',(2.96649892652511,-5.45661638644921,1.00349332232709));
#53910=CARTESIAN_POINT('Ctrl Pts',(6.19423229821208,-0.454163523115957,
1.28191717597421));
#53911=CARTESIAN_POINT('Ctrl Pts',(3.73065829119942,4.96557821247941,1.56034102962135));
#53912=CARTESIAN_POINT('Ctrl Pts',(-2.16067270617363,5.82290921505217,1.83876488326847));
#53913=CARTESIAN_POINT('Ctrl Pts',(-6.06676131618066,1.33010728982196,2.11718873691561));
#53914=CARTESIAN_POINT('Ctrl Pts',(-4.39866384770363,-4.38480725059255,
2.39561259056273));
#53915=CARTESIAN_POINT('Ctrl Pts',(1.31095915737338,-6.07092780039778,2.67403644420987));
#53916=CARTESIAN_POINT('Ctrl Pts',(5.81606299585617,-2.17903407457897,2.95246029785699));
#53917=CARTESIAN_POINT('Ctrl Pts',(4.97732426439622,3.71497260245568,3.23088415150413));
#53918=CARTESIAN_POINT('Ctrl Pts',(-0.434617561225553,6.1956344183157,3.50930800515125));
#53919=CARTESIAN_POINT('Ctrl Pts',(-5.44722949186912,2.98370057694384,3.78773185879839));
#53920=CARTESIAN_POINT('Ctrl Pts',(-5.45488585933577,-2.96967987021536,
4.06615571244551));
#53921=CARTESIAN_POINT('Ctrl Pts',(-0.450551935420432,-6.19449604273283,
4.34457956609265));
#53922=CARTESIAN_POINT('Ctrl Pts',(4.96775250672782,-3.72776250609439,4.62300341973977));
#53923=CARTESIAN_POINT('Ctrl Pts',(5.82164845789067,2.16406735169747,4.9014272733869));
#53924=CARTESIAN_POINT('Ctrl Pts',(1.32656987444429,6.06753579619937,5.17985112703403));
#53925=CARTESIAN_POINT('Ctrl Pts',(-4.38737112024312,4.39610656413154,5.45827498068116));
#53926=CARTESIAN_POINT('Ctrl Pts',(-6.07016242153879,-1.31449855309236,
5.73669883432829));
#53927=CARTESIAN_POINT('Ctrl Pts',(-2.1756426830818,-5.81733248022635,6.01512268797542));
#53928=CARTESIAN_POINT('Ctrl Pts',(3.71787397049125,-4.97515742559844,6.29354654162255));
#53929=CARTESIAN_POINT('Ctrl Pts',(6.19537996404417,0.438229815352393,6.57197039526968));
#53930=CARTESIAN_POINT('Ctrl Pts',(2.98052409487006,5.44896819497442,6.85039424891681));
#53931=CARTESIAN_POINT('Ctrl Pts',(-2.97285980439152,5.45315347788571,7.12881810256394));
#53932=CARTESIAN_POINT('Ctrl Pts',(-6.19475768149381,0.446940194564266,
7.40724195621107));
#53933=CARTESIAN_POINT('Ctrl Pts',(-3.72486545377224,-4.96992511223639,
7.68566580985821));
#53934=CARTESIAN_POINT('Ctrl Pts',(2.16746126156735,-5.8203857217154,7.96408966350532));
#53935=CARTESIAN_POINT('Ctrl Pts',(6.06830821361728,-1.32303200811196,8.24251351715246));
#53936=CARTESIAN_POINT('Ctrl Pts',(4.3935477861451,4.38993349844886,8.52093737079958));
#53937=CARTESIAN_POINT('Ctrl Pts',(-1.31803750196012,6.06939497918618,8.79936122444673));
#53938=CARTESIAN_POINT('Ctrl Pts',(-5.81859998704997,2.17225055199571,9.07778507809384));
#53939=CARTESIAN_POINT('Ctrl Pts',(-4.97298889554354,-3.72077407467108,
9.35620893174098));
#53940=CARTESIAN_POINT('Ctrl Pts',(0.441841920507206,-6.19512340371251,
9.6346327853881));
#53941=CARTESIAN_POINT('Ctrl Pts',(5.45070504575508,-2.97734659959565,9.91305663903523));
#53942=CARTESIAN_POINT('Ctrl Pts',(5.45141924268827,2.9760387279724,10.1914804926824));
#53943=CARTESIAN_POINT('Ctrl Pts',(0.443328301775111,6.19501721440619,10.4699043463295));
#53944=CARTESIAN_POINT('Ctrl Pts',(-4.97209602826647,3.7219671352177,10.7483281999766));
#53945=CARTESIAN_POINT('Ctrl Pts',(-5.81912100695569,-2.17085443462954,
11.0267520536238));
#53946=CARTESIAN_POINT('Ctrl Pts',(-1.31949369202748,-6.06907856817188,
11.3051759072709));
#53947=CARTESIAN_POINT('Ctrl Pts',(4.39249438433867,-4.3909875146141,11.583599760918));
#53948=CARTESIAN_POINT('Ctrl Pts',(6.06862547360082,1.32157600277364,11.8620236145652));
#53949=CARTESIAN_POINT('Ctrl Pts',(2.1688576824738,5.81986551589623,12.1404474682123));
#53950=CARTESIAN_POINT('Ctrl Pts',(-3.7236729140094,4.97081867496857,12.4188713218594));
#53951=CARTESIAN_POINT('Ctrl Pts',(-6.19486473740788,-0.445453875462067,
12.6972951755065));
#53952=CARTESIAN_POINT('Ctrl Pts',(-2.97416809220076,-5.45244004362073,
12.9757190291537));
#53953=CARTESIAN_POINT('Ctrl Pts',(2.97921663987744,-5.44968315433302,13.2541428828008));
#53954=CARTESIAN_POINT('Ctrl Pts',(6.1952746413817,-0.439716258280684,13.5325667364479));
#53955=CARTESIAN_POINT('Ctrl Pts',(3.71906755141604,4.97426525408005,13.8109905900951));
#53956=CARTESIAN_POINT('Ctrl Pts',(-2.1742468697305,5.81785431404147,14.0894144437422));
#53957=CARTESIAN_POINT('Ctrl Pts',(-6.06984685960131,1.31595492739377,14.3678382973893));
#53958=CARTESIAN_POINT('Ctrl Pts',(-4.38842575040887,-4.39505377704208,
14.6462621510364));
#53959=CARTESIAN_POINT('Ctrl Pts',(1.32511405433002,-6.06785390504426,14.9246860046836));
#53960=CARTESIAN_POINT('Ctrl Pts',(5.82112906633488,-2.1654640756695,15.2031098583307));
#53961=CARTESIAN_POINT('Ctrl Pts',(4.96864676461137,3.72657048752075,15.4815337119778));
#53962=CARTESIAN_POINT('Ctrl Pts',(-0.449065678989183,6.19460396521824,
15.759957565625));
#53963=CARTESIAN_POINT('Ctrl Pts',(-5.45417318798152,2.97098857376587,16.0383814192721));
#53964=CARTESIAN_POINT('Ctrl Pts',(-5.44794521341013,-2.98239353902625,
16.3168052729192));
#53965=CARTESIAN_POINT('Ctrl Pts',(-0.436104065308916,-6.19552996233291,
16.5952291265663));
#53966=CARTESIAN_POINT('Ctrl Pts',(4.97643278893975,-3.71616670335292,16.8736529802135));
#53967=CARTESIAN_POINT('Ctrl Pts',(5.81658564340332,2.17763856571702,17.1520768338606));
#53968=CARTESIAN_POINT('Ctrl Pts',(1.31241571541379,6.07061308764435,17.4305006875077));
#53969=CARTESIAN_POINT('Ctrl Pts',(-4.39761167568901,4.38586249440032,17.7089245411549));
#53970=CARTESIAN_POINT('Ctrl Pts',(-6.06708027377879,-1.3286516554266,17.987348394802));
#53971=CARTESIAN_POINT('Ctrl Pts',(-2.16206973273641,-5.82239063793635,
18.2657722484491));
#53972=CARTESIAN_POINT('Ctrl Pts',(3.72946679422009,-4.96647316521026,18.5441961020963));
#53973=CARTESIAN_POINT('Ctrl Pts',(6.19434108723227,0.452677329860728,18.8226199557434));
#53974=CARTESIAN_POINT('Ctrl Pts',(2.9678080453718,5.45590447824831,19.1010438093905));
#53975=CARTESIAN_POINT('Ctrl Pts',(-2.98556942433889,5.44620542051037,19.3794676630377));
#53976=CARTESIAN_POINT('Ctrl Pts',(-6.19578317717296,0.432491724087773,
19.6578915166847));
#53977=CARTESIAN_POINT('Ctrl Pts',(-3.71326459201449,-4.97859863210875,
19.9363153703319));
#53978=CARTESIAN_POINT('Ctrl Pts',(2.18102952143619,-5.81531499547251,20.214739223979));
#53979=CARTESIAN_POINT('Ctrl Pts',(6.07137725204052,-1.30887605729064,20.4931630776262));
#53980=CARTESIAN_POINT('Ctrl Pts',(4.38329774745979,4.40016807940991,20.7715869312733));
#53981=CARTESIAN_POINT('Ctrl Pts',(-1.33218880486076,6.06630458006745,21.0500107849204));
#53982=CARTESIAN_POINT('Ctrl Pts',(-5.82365023027184,2.15867465482835,21.3284346385676));
#53983=CARTESIAN_POINT('Ctrl Pts',(-4.96429787750409,-3.73236183312285,
21.6068584922147));
#53984=CARTESIAN_POINT('Ctrl Pts',(0.456288826848907,-6.19407610353931,
21.8852823458618));
#53985=CARTESIAN_POINT('Ctrl Pts',(5.4576339138326,-2.96462650809979,22.163706199509));
#53986=CARTESIAN_POINT('Ctrl Pts',(5.44446377622514,2.9887442947358,22.4421300531561));
#53987=CARTESIAN_POINT('Ctrl Pts',(0.428879235845219,6.19603428581577,22.7205539068032));
#53988=CARTESIAN_POINT('Ctrl Pts',(-4.9807627828508,3.7103612183873,22.9989777604504));
#53989=CARTESIAN_POINT('Ctrl Pts',(-5.81404237068101,-2.18441973573531,
23.2774016140974));
#53990=CARTESIAN_POINT('Ctrl Pts',(-1.30533595422747,-6.07213935253009,
23.5558254677446));
#53991=CARTESIAN_POINT('Ctrl Pts',(4.40272298733576,-4.38073151045905,23.8342493213917));
#53992=CARTESIAN_POINT('Ctrl Pts',(6.06552682417391,1.3357255014301,24.1126731750389));
#53993=CARTESIAN_POINT('Ctrl Pts',(2.15527884309945,5.82490784291321,24.391097028686));
#53994=CARTESIAN_POINT('Ctrl Pts',(-3.73525560324502,4.96212090223225,24.6695208823331));
#53995=CARTESIAN_POINT('Ctrl Pts',(-6.19380901422938,-0.459900168726112,
24.9479447359802));
#53996=CARTESIAN_POINT('Ctrl Pts',(-2.96144396303136,-5.45936149414647,
25.2263685896274));
#53997=CARTESIAN_POINT('Ctrl Pts',(2.99191814913776,-5.44272028114656,25.5047924432745));
#53998=CARTESIAN_POINT('Ctrl Pts',(6.196283288176,-0.425266601809134,25.7832162969216));
#53999=CARTESIAN_POINT('Ctrl Pts',(3.70745658345825,4.98292524043012,26.0616401505688));
#54000=CARTESIAN_POINT('Ctrl Pts',(-2.18780920746171,5.81276776946144,26.3400640042159));
#54001=CARTESIAN_POINT('Ctrl Pts',(-6.07289938885401,1.30179540742797,26.618487857863));
#54002=CARTESIAN_POINT('Ctrl Pts',(-4.37816378427055,-4.40527639859808,
26.8969117115101));
#54003=CARTESIAN_POINT('Ctrl Pts',(1.33926174393233,-6.06474700636252,27.1753355651573));
#54004=CARTESIAN_POINT('Ctrl Pts',(5.82616347543284,-2.15188229870415,27.4537594188044));
#54005=CARTESIAN_POINT('Ctrl Pts',(4.95994224013495,3.73814810360272,27.7321832724515));
#54006=CARTESIAN_POINT('Ctrl Pts',(-0.463511354264669,6.19353981939337,
28.0106071260987));
#54007=CARTESIAN_POINT('Ctrl Pts',(-5.46108721860255,2.95826041124837,28.2890309797457));
#54008=CARTESIAN_POINT('Ctrl Pts',(-5.4409749358673,-2.99509098646564,28.567454833393));
#54009=CARTESIAN_POINT('Ctrl Pts',(-0.421653823207863,-6.19653018416905,
28.8458786870401));
#54010=CARTESIAN_POINT('Ctrl Pts',(4.98508600411173,-3.70455068821481,29.1243025406872));
#54011=CARTESIAN_POINT('Ctrl Pts',(5.81149119224705,2.19119793546338,29.4027263943343));
#54012=CARTESIAN_POINT('Ctrl Pts',(1.2982544180955,6.07365736075385,29.6811502479814));
#54013=CARTESIAN_POINT('Ctrl Pts',(-4.40782831232883,4.37559456976717,29.9595741016286));
#54014=CARTESIAN_POINT('Ctrl Pts',(-6.0639651268984,-1.34279753116531,30.2379979552757));
#54015=CARTESIAN_POINT('Ctrl Pts',(-2.14848502279716,-5.82741712740386,
30.5164218089228));
#54016=CARTESIAN_POINT('Ctrl Pts',(3.74103933321266,-4.95776189195283,30.79484566257));
#54017=CARTESIAN_POINT('Ctrl Pts',(6.19326851912278,0.467122382236926,31.0732695162171));
#54018=CARTESIAN_POINT('Ctrl Pts',(2.95507585383304,5.46281108661433,31.3516933698642));
#54019=CARTESIAN_POINT('Ctrl Pts',(-2.99826280564106,5.43922774098064,31.6301172235114));
#54020=CARTESIAN_POINT('Ctrl Pts',(-6.19677497371092,0.418040901269345,
31.9085410771585));
#54021=CARTESIAN_POINT('Ctrl Pts',(-3.7016435336448,-4.98724507316104,32.1869649308056));
#54022=CARTESIAN_POINT('Ctrl Pts',(2.1945859185882,-5.81021263947181,32.4653887844528));
#54023=CARTESIAN_POINT('Ctrl Pts',(6.07441326797193,-1.29471298743398,32.7438126380998));
#54024=CARTESIAN_POINT('Ctrl Pts',(4.37302386782237,4.41037872766044,33.022236491747));
#54025=CARTESIAN_POINT('Ctrl Pts',(-1.3463328619271,6.0631811860474,33.3006603453941));
#54026=CARTESIAN_POINT('Ctrl Pts',(-5.82866879840025,2.14508701653312,33.5790841990412));
#54027=CARTESIAN_POINT('Ctrl Pts',(-4.95557985842688,-3.74392929109215,
33.8575080526884));
#54028=CARTESIAN_POINT('Ctrl Pts',(0.470733251415439,-6.19299511350976,
34.1359319063355));
#54029=CARTESIAN_POINT('Ctrl Pts',(5.46453309759574,-2.95189029186794,34.4143557599827));
#54030=CARTESIAN_POINT('Ctrl Pts',(5.43747869708053,3.00143360558567,34.6927796136298));
#54031=CARTESIAN_POINT('Ctrl Pts',(0.414427837221952,6.19701765671836,34.9712034672769));
#54032=CARTESIAN_POINT('Ctrl Pts',(-4.98940244684405,3.69873512073661,35.249627320924));
#54033=CARTESIAN_POINT('Ctrl Pts',(-5.80893211157042,-2.19797315568457,
35.5280511745712));
#54034=CARTESIAN_POINT('Ctrl Pts',(-1.29117111664705,-6.07516711025136,
35.8064750282183));
#54035=CARTESIAN_POINT('Ctrl Pts',(4.41292764372606,-4.37045167930985,36.0848988818654));
#54036=CARTESIAN_POINT('Ctrl Pts',(6.06239518407591,1.34986773501598,36.3633227355126));
#54037=CARTESIAN_POINT('Ctrl Pts',(2.14168828106728,5.82991848799643,36.6417465891597));
#54038=CARTESIAN_POINT('Ctrl Pts',(-3.74681797625863,4.95339614029897,36.9201704428068));
#54039=CARTESIAN_POINT('Ctrl Pts',(-6.19271960264728,-0.47434396057257,
37.1985942964539));
#54040=CARTESIAN_POINT('Ctrl Pts',(-2.94870372643611,-5.46625325096137,
37.4770181501011));
#54041=CARTESIAN_POINT('Ctrl Pts',(3.00460338522167,-5.43572780476161,37.7554420037482));
#54042=CARTESIAN_POINT('Ctrl Pts',(6.19725823310897,-0.410814632293651,
38.0338658573953));
#54043=CARTESIAN_POINT('Ctrl Pts',(3.69582545047869,4.99155812442748,38.3122897110425));
#54044=CARTESIAN_POINT('Ctrl Pts',(-2.20135964560103,5.80764960897808,38.5907135646896));
#54045=CARTESIAN_POINT('Ctrl Pts',(-6.07591888733587,1.28762880693885,38.8691374183368));
#54046=CARTESIAN_POINT('Ctrl Pts',(-4.36787800510409,-4.4154750596591,39.1475612719838));
#54047=CARTESIAN_POINT('Ctrl Pts',(1.35340214923009,-6.06160712125117,39.425985125631));
#54048=CARTESIAN_POINT('Ctrl Pts',(5.83116619576758,-2.13828881755513,39.7044089792781));
#54049=CARTESIAN_POINT('Ctrl Pts',(4.95121073831148,3.74970538773023,39.9828328329253));
#54050=CARTESIAN_POINT('Ctrl Pts',(-0.477954508481131,6.19244198662903,
40.2612566865723));
#54051=CARTESIAN_POINT('Ctrl Pts',(-5.46797154612653,2.94551615862052,40.5396805402195));
#54052=CARTESIAN_POINT('Ctrl Pts',(-5.43397506461897,-3.00777214347152,
40.8181043938666));
#54053=CARTESIAN_POINT('Ctrl Pts',(-0.407201287712849,-6.19749670280094,
41.0965282475137));
#54054=CARTESIAN_POINT('Ctrl Pts',(4.99371210517841,-3.69291452386027,41.3749521011609));
#54055=CARTESIAN_POINT('Ctrl Pts',(5.80636513213084,2.2047453871862,41.653375954808));
#54056=CARTESIAN_POINT('Ctrl Pts',(1.28408605951368,6.07666859896988,41.9317998084552));
#54057=CARTESIAN_POINT('Ctrl Pts',(-4.41802097459366,4.36530284608003,42.2102236621023));
#54058=CARTESIAN_POINT('Ctrl Pts',(-6.06081699784108,-1.35693610336823,
42.4886475157494));
#54059=CARTESIAN_POINT('Ctrl Pts',(-2.13488862715202,-5.83241192128959,
42.7670713693965));
#54060=CARTESIAN_POINT('Ctrl Pts',(3.75259152452537,-4.9490236532072,43.0454952230437));
#54061=CARTESIAN_POINT('Ctrl Pts',(6.19216226554937,0.481564893913621,43.3239190766908));
#54062=CARTESIAN_POINT('Ctrl Pts',(2.94232758950492,5.46968798250703,43.602342930338));
#54063=CARTESIAN_POINT('Ctrl Pts',(-3.01093987925787,5.43222047724852,43.880766783985));
#54064=CARTESIAN_POINT('Ctrl Pts',(-6.19773306571321,0.403587804708005,
44.1591906376322));
#54065=CARTESIAN_POINT('Ctrl Pts',(-3.69000234187092,-4.99586438836475,
44.4376144912793));
#54066=CARTESIAN_POINT('Ctrl Pts',(2.2081303792894,-5.80507868146529,44.7160383449265));
#54067=CARTESIAN_POINT('Ctrl Pts',(6.07741624489852,-1.28054287557562,44.9944621985735));
#54068=CARTESIAN_POINT('Ctrl Pts',(4.36272620311297,4.42056538766427,45.2728860522208));
#54069=CARTESIAN_POINT('Ctrl Pts',(-1.36046959622891,6.06002481411424,45.5513099058677));
#54070=CARTESIAN_POINT('Ctrl Pts',(-5.83365566413891,2.13148771101397,45.8297337595151));
#54071=CARTESIAN_POINT('Ctrl Pts',(-4.94683488572972,-3.75547638566279,
46.108157613162));
#54072=CARTESIAN_POINT('Ctrl Pts',(0.485175115642611,-6.19188043950342,
46.3865814668093));
#54073=CARTESIAN_POINT('Ctrl Pts',(5.47140255951946,-2.93913802017323,46.6650053204563));
#54074=CARTESIAN_POINT('Ctrl Pts',(5.43046404324665,3.01410659150414,46.9434291741035));
#54075=CARTESIAN_POINT('Ctrl Pts',(0.399974184507209,6.19796732176539,47.2218530277506));
#54076=CARTESIAN_POINT('Ctrl Pts',(-4.99801497325478,3.68708890550052,47.5002768813978));
#54077=CARTESIAN_POINT('Ctrl Pts',(-5.80379025741878,-2.2115146207598,47.7787007350449));
#54078=CARTESIAN_POINT('Ctrl Pts',(-1.2769992563293,-6.07816182486761,48.057124588692));
#54079=CARTESIAN_POINT('Ctrl Pts',(4.42310829800586,-4.36014807707895,48.3355484423391));
#54080=CARTESIAN_POINT('Ctrl Pts',(6.05923057033998,1.36400262661085,48.6139722959862));
#54081=CARTESIAN_POINT('Ctrl Pts',(2.12808607029709,5.83489742389285,48.8923961496335));
#54082=CARTESIAN_POINT('Ctrl Pts',(-3.75835997016207,4.94464443662301,49.1708200032804));
#54083=CARTESIAN_POINT('Ctrl Pts',(-6.19159650858692,-0.488785172441089,
49.4492438569277));
#54084=CARTESIAN_POINT('Ctrl Pts',(-2.93594745170962,-5.47311527658095,
49.7276677105747));
#54085=CARTESIAN_POINT('Ctrl Pts',(3.0172722791337,-5.42870576321049,50.006091564222));
#54086=CARTESIAN_POINT('Ctrl Pts',(6.19819947087785,-0.39636042833906,50.284515417869));
#54087=CARTESIAN_POINT('Ctrl Pts',(3.68417421573959,5.00016385911732,50.5629392715162));
#54088=CARTESIAN_POINT('Ctrl Pts',(-2.21489811044685,5.80249986042937,50.8413631251632));
#54089=CARTESIAN_POINT('Ctrl Pts',(-6.0789053386238,1.2734552029793,51.1197869788105));
#54090=CARTESIAN_POINT('Ctrl Pts',(-4.35756846885422,-4.4256497047542,51.3982108324575));
#54091=CARTESIAN_POINT('Ctrl Pts',(1.36753519331326,-6.05843426678821,51.6766346861046));
#54092=CARTESIAN_POINT('Ctrl Pts',(5.83613720012922,-2.12468370615766,51.9550585397519));
#54093=CARTESIAN_POINT('Ctrl Pts',(4.94245230663171,3.76124227704283,52.2334823933989));
#54094=CARTESIAN_POINT('Ctrl Pts',(-0.492395063081671,6.19131047289637,
52.5119062470461));
#54095=CARTESIAN_POINT('Ctrl Pts',(-5.47482613310915,2.93275588519888,52.7903301006932));
#54096=CARTESIAN_POINT('Ctrl Pts',(-5.42694563773782,-3.02043694107034,
53.0687539543404));
#54097=CARTESIAN_POINT('Ctrl Pts',(-0.392746537431982,-6.19842951297174,
53.3471778079874));
#54098=CARTESIAN_POINT('Ctrl Pts',(5.0023110452221,-3.68125827357881,53.6256016616347));
#54099=CARTESIAN_POINT('Ctrl Pts',(5.80120749093557,2.21828084720058,53.9040255152817));
#54100=CARTESIAN_POINT('Ctrl Pts',(1.26991071673034,6.07964678591425,54.1824493689289));
#54101=CARTESIAN_POINT('Ctrl Pts',(-4.42818960704527,4.35498737931578,54.4608732225759));
#54102=CARTESIAN_POINT('Ctrl Pts',(-6.05763590372964,-1.37106729513512,
54.7392970762232));
#54103=CARTESIAN_POINT('Ctrl Pts',(-2.12128061975243,-5.83737499242651,
55.0177209298702));
#54104=CARTESIAN_POINT('Ctrl Pts',(3.76412330532518,-4.94025849650115,55.2961447835174));
#54105=CARTESIAN_POINT('Ctrl Pts',(6.19102233252913,0.496004786337269,55.5745686371645));
#54106=CARTESIAN_POINT('Ctrl Pts',(2.92956332172572,5.47653512852268,55.8529924908116));
#54107=CARTESIAN_POINT('Ctrl Pts',(-3.02360057623841,5.42518366742681,56.1314163444588));
#54108=CARTESIAN_POINT('Ctrl Pts',(-6.1986574479688,0.389132513014424,56.4098401981059));
#54109=CARTESIAN_POINT('Ctrl Pts',(-3.6783410800095,-5.0044565308391,56.688264051753));
#54110=CARTESIAN_POINT('Ctrl Pts',(2.22166282987091,-5.79991314937677,56.9666879054002));
#54111=CARTESIAN_POINT('Ctrl Pts',(6.08038616648687,-1.2663657987875,57.2451117590473));
#54112=CARTESIAN_POINT('Ctrl Pts',(4.35240480934116,4.43072800401557,57.5235356126944));
#54113=CARTESIAN_POINT('Ctrl Pts',(-1.37459893087578,6.05683548143575,57.8019594663416));
#54114=CARTESIAN_POINT('Ctrl Pts',(-5.83861080036407,2.11787681223804,58.0803833199886));
#54115=CARTESIAN_POINT('Ctrl Pts',(-4.93806300697687,-3.7670030540299,58.3588071736358));
#54116=CARTESIAN_POINT('Ctrl Pts',(0.499614340980781,-6.19073208758301,
58.6372310272829));
#54117=CARTESIAN_POINT('Ctrl Pts',(5.47824226224044,-2.9263697623756,58.9156548809301));
#54118=CARTESIAN_POINT('Ctrl Pts',(5.42341985287656,3.02676318356225,59.1940787345772));
#54119=CARTESIAN_POINT('Ctrl Pts',(0.385518356315185,6.1988832757915,59.4725025882243));
#54120=CARTESIAN_POINT('Ctrl Pts',(-5.00660031523891,3.6754226360235,59.7509264418715));
#54121=CARTESIAN_POINT('Ctrl Pts',(-5.79861683619302,-2.22504405730817,
60.0293502955185));
#54122=CARTESIAN_POINT('Ctrl Pts',(-1.26282045035567,-6.08112348009042,
60.3077741491658));
#54123=CARTESIAN_POINT('Ctrl Pts',(4.43326489480233,-4.34982075980811,60.5861980028128));
#54124=CARTESIAN_POINT('Ctrl Pts',(6.05603300017853,1.37813009933466,60.86462185646));
#54125=CARTESIAN_POINT('Ctrl Pts',(2.11447228477175,5.83984462352173,61.1430457101071));
#54126=CARTESIAN_POINT('Ctrl Pts',(-3.76988152217794,4.93586583880535,61.4214695637542));
#54127=CARTESIAN_POINT('Ctrl Pts',(-6.19043973815677,-0.503223725785225,
61.6998934174013));
#54128=CARTESIAN_POINT('Ctrl Pts',(-2.92317520823401,-5.47994753368219,
61.9783172710485));
#54129=CARTESIAN_POINT('Ctrl Pts',(3.02992476196705,-5.42165419468657,62.2567411246955));
#54130=CARTESIAN_POINT('Ctrl Pts',(6.19910699636319,-0.381904068562471,
62.5351649783428));
#54131=CARTESIAN_POINT('Ctrl Pts',(3.67250294261256,5.0087423976929,62.8135888319898));
#54132=CARTESIAN_POINT('Ctrl Pts',(-2.22842452836309,5.79731855182492,63.0920126856371));
#54133=CARTESIAN_POINT('Ctrl Pts',(-6.08185872647424,1.25927467264003,63.3704365392841));
#54134=CARTESIAN_POINT('Ctrl Pts',(-4.34723523159504,-4.43580027854311,
63.6488603929313));
#54135=CARTESIAN_POINT('Ctrl Pts',(1.38166079931146,-6.05522846023084,63.9272842465784));
#54136=CARTESIAN_POINT('Ctrl Pts',(5.8410764614801,-2.11106703851077,64.2057081002255));
#54137=CARTESIAN_POINT('Ctrl Pts',(4.9336669927334,3.77275870879084,64.4841319538727));
#54138=CARTESIAN_POINT('Ctrl Pts',(-0.506832939523575,6.19014528434975,
64.7625558075197));
#54139=CARTESIAN_POINT('Ctrl Pts',(-5.48165094226821,2.91997966038697,65.040979661167));
#54140=CARTESIAN_POINT('Ctrl Pts',(-5.41988669345709,-3.03308531037791,
65.319403514814));
#54141=CARTESIAN_POINT('Ctrl Pts',(-0.378289650985128,-6.19932860960775,
65.5978273684612));
#54142=CARTESIAN_POINT('Ctrl Pts',(5.01088277747282,-3.66958200076937,65.8762512221083));
#54143=CARTESIAN_POINT('Ctrl Pts',(5.79601829671383,2.2318042418864,66.1546750757555));
#54144=CARTESIAN_POINT('Ctrl Pts',(1.25572846684602,6.08259190538837,66.4330989294025));
#54145=CARTESIAN_POINT('Ctrl Pts',(-4.43833415437589,4.34464822558098,66.7115227830498));
#54146=CARTESIAN_POINT('Ctrl Pts',(-6.0544218618662,-1.38519102960575,66.9899466366968));
#54147=CARTESIAN_POINT('Ctrl Pts',(-2.10766107461286,-5.84230631382042,
67.268370490344));
#54148=CARTESIAN_POINT('Ctrl Pts',(3.7756346128904,-4.93146646950858,67.5467943439911));
#54149=CARTESIAN_POINT('Ctrl Pts',(6.18984872626208,0.510441980968776,67.8252181976383));
#54150=CARTESIAN_POINT('Ctrl Pts',(2.9167831199209,5.48335248741942,68.1036420512853));
#54151=CARTESIAN_POINT('Ctrl Pts',(-3.03624482772044,5.41811734978899,68.3820659049325));
#54152=CARTESIAN_POINT('Ctrl Pts',(-6.19954811544985,0.374675104811834,
68.6604897585795));
#54153=CARTESIAN_POINT('Ctrl Pts',(-3.66665981148688,-5.01302145385108,
68.9389136122268));
#54154=CARTESIAN_POINT('Ctrl Pts',(2.23518319672922,-5.79471607130176,69.2173374658739));
#54155=CARTESIAN_POINT('Ctrl Pts',(6.08332301658356,-1.25218183417913,69.4957613195209));
#54156=CARTESIAN_POINT('Ctrl Pts',(4.34205974264528,4.44086652143958,69.7741851731683));
#54157=CARTESIAN_POINT('Ctrl Pts',(-1.38872078901773,6.05361320535872,70.0526090268151));
#54158=CARTESIAN_POINT('Ctrl Pts',(-5.84353418012459,2.10425439423563,70.3310328804625));
#54159=CARTESIAN_POINT('Ctrl Pts',(-4.9292642698789,-3.77850923349922,70.6094567341095));
#54160=CARTESIAN_POINT('Ctrl Pts',(0.514050848894259,-6.18955006399452,
70.8878805877567));
#54161=CARTESIAN_POINT('Ctrl Pts',(5.4850521685573,-2.91358558792228,71.1663044414038));
#54162=CARTESIAN_POINT('Ctrl Pts',(5.41634616428379,3.03940331292046,71.4447282950509));
#54163=CARTESIAN_POINT('Ctrl Pts',(0.371060431271426,6.19976551381493,71.7231521486979));
#54164=CARTESIAN_POINT('Ctrl Pts',(-5.01515842610055,3.66373637575853,72.0015760023452));
#54165=CARTESIAN_POINT('Ctrl Pts',(-5.79341187603146,-2.23856139174275,
72.2799998559922));
#54166=CARTESIAN_POINT('Ctrl Pts',(-1.24863477584512,-6.08405205981133,
72.5584237096394));
#54167=CARTESIAN_POINT('Ctrl Pts',(4.44339737887316,-4.3394697836679,72.8368475632866));
#54168=CARTESIAN_POINT('Ctrl Pts',(6.05280249098336,1.39225007634737,73.1152714169336));
#54169=CARTESIAN_POINT('Ctrl Pts',(2.10084699853723,5.8447600599752,73.3936952705809));
#54170=CARTESIAN_POINT('Ctrl Pts',(-3.78138256963996,4.92706039459298,73.6721191242278));
#54171=CARTESIAN_POINT('Ctrl Pts',(-6.18924929764864,-0.517659542073067,
73.9505429778751));
#54172=CARTESIAN_POINT('Ctrl Pts',(-2.91038706547802,-5.48674998510428,
74.2289668315222));
#54173=CARTESIAN_POINT('Ctrl Pts',(3.04256076490452,-5.41457313754346,74.5073906851693));
#54174=CARTESIAN_POINT('Ctrl Pts',(6.19998080462899,-0.367445631592474,
74.7858145388165));
#54175=CARTESIAN_POINT('Ctrl Pts',(3.66081169457798,5.017293693495,75.0642383924636));
#54176=CARTESIAN_POINT('Ctrl Pts',(-2.24193882577889,5.79210571134614,75.3426622461107));
#54177=CARTESIAN_POINT('Ctrl Pts',(-6.08477903482368,1.24508729304965,75.6210860997579));
#54178=CARTESIAN_POINT('Ctrl Pts',(-4.33687834952939,-4.44592672581621,
75.8995099534049));
#54179=CARTESIAN_POINT('Ctrl Pts',(1.39577889039483,-6.05198971901576,76.1779338070522));
#54180=CARTESIAN_POINT('Ctrl Pts',(5.84598395295547,-2.09743888867607,76.4563576606991));
#54181=CARTESIAN_POINT('Ctrl Pts',(4.92485484440009,3.78425462033575,76.7347815143464));
#54182=CARTESIAN_POINT('Ctrl Pts',(-0.521268059278363,6.18894642732675,
77.0132053679934));
#54183=CARTESIAN_POINT('Ctrl Pts',(-5.48844593648309,2.90718755367551,77.2916292216407));
#54184=CARTESIAN_POINT('Ctrl Pts',(-5.41279827017078,-3.04571718259916,
77.5700530752877));
#54185=CARTESIAN_POINT('Ctrl Pts',(-0.363830707003893,-6.20019398781887,
77.8484769289348));
#54186=CARTESIAN_POINT('Ctrl Pts',(5.01942725530845,-3.65788576893953,78.126900782582));
#54187=CARTESIAN_POINT('Ctrl Pts',(5.79079757768992,2.24531549768938,78.4053246362291));
#54188=CARTESIAN_POINT('Ctrl Pts',(1.24153938699856,6.08550394137369,78.6837484898763));
#54189=CARTESIAN_POINT('Ctrl Pts',(-4.4484545614091,4.33428544111047,78.9621723435234));
#54190=CARTESIAN_POINT('Ctrl Pts',(-6.05117488973208,-1.39930722996069,
79.2405961971704));
#54191=CARTESIAN_POINT('Ctrl Pts',(-2.09403006581055,-5.8472058586495,79.5190200508177));
#54192=CARTESIAN_POINT('Ctrl Pts',(3.78712538461051,-4.92264762004982,79.7974439044648));
#54193=CARTESIAN_POINT('Ctrl Pts',(6.18864145313159,0.524876399283552,80.0758677581119));
#54194=CARTESIAN_POINT('Ctrl Pts',(2.90398705360255,5.49014002211714,80.354291611759));
#54195=CARTESIAN_POINT('Ctrl Pts',(-3.04887256493131,5.41102156276922,80.6327154654062));
#54196=CARTESIAN_POINT('Ctrl Pts',(-6.20040506331207,0.360215658734639,
80.9111393190533));
#54197=CARTESIAN_POINT('Ctrl Pts',(-3.65495859983791,-5.02155911081553,
81.1895631727004));
#54198=CARTESIAN_POINT('Ctrl Pts',(2.24869140632625,-5.78948747550755,81.4679870263477));
#54199=CARTESIAN_POINT('Ctrl Pts',(6.08622677921486,-1.23799105889803,81.7464108799947));
#54200=CARTESIAN_POINT('Ctrl Pts',(4.33169105929267,4.45098088479241,82.0248347336419));
#54201=CARTESIAN_POINT('Ctrl Pts',(-1.40283509384545,6.05035800340937,82.3032585872889));
#54202=CARTESIAN_POINT('Ctrl Pts',(-5.84842577664184,2.09062053109955,82.5816824409361));
#54203=CARTESIAN_POINT('Ctrl Pts',(-4.92043872229259,-3.78999486148822,
82.8601062945833));
#54204=CARTESIAN_POINT('Ctrl Pts',(0.528484560862153,-6.18833437516702,
83.1385301482302));
#54205=CARTESIAN_POINT('Ctrl Pts',(5.49183224143067,-2.90078556634683,83.4169540018776));
#54206=CARTESIAN_POINT('Ctrl Pts',(5.40924301594254,3.05202691082846,83.6953778555245));
#54207=CARTESIAN_POINT('Ctrl Pts',(0.35660048801342,6.20061403103695,83.9738017091718));
#54208=CARTESIAN_POINT('Ctrl Pts',(-5.02368925929172,3.65203018826795,84.2522255628188));
#54209=CARTESIAN_POINT('Ctrl Pts',(-5.78817540524418,-2.25206655054194,
84.530649416466));
#54210=CARTESIAN_POINT('Ctrl Pts',(-1.23444230995443,-6.08694754810143,
84.8090732701131));
#54211=CARTESIAN_POINT('Ctrl Pts',(4.45350569510733,-4.32909520495806,85.0874971237602));
#54212=CARTESIAN_POINT('Ctrl Pts',(6.04953906032532,1.40636248084973,85.3659209774074));
#54213=CARTESIAN_POINT('Ctrl Pts',(2.08721028570223,5.84964370651772,85.6443448310545));
#54214=CARTESIAN_POINT('Ctrl Pts',(-3.79286304999338,4.91822815187942,85.9227686847017));
#54215=CARTESIAN_POINT('Ctrl Pts',(-6.1880251935374,-0.532092542787492,
86.2011925383488));
#54216=CARTESIAN_POINT('Ctrl Pts',(-2.89758309299682,-5.49352259384837,
86.4796163919959));
#54217=CARTESIAN_POINT('Ctrl Pts',(3.05518021921827,-5.40746263029544,86.758040245643));
#54218=CARTESIAN_POINT('Ctrl Pts',(6.20082089092238,-0.352985196069277,
87.0364640992902));
#54219=CARTESIAN_POINT('Ctrl Pts',(3.6491005352253,5.0258177000128,87.3148879529372));
#54220=CARTESIAN_POINT('Ctrl Pts',(-2.2554409291893,5.78686136734597,87.5933118065845));
#54221=CARTESIAN_POINT('Ctrl Pts',(-6.08766624778842,1.23089314137383,87.8717356602316));
#54222=CARTESIAN_POINT('Ctrl Pts',(-4.32649787898883,-4.45602899149562,
88.1501595138786));
#54223=CARTESIAN_POINT('Ctrl Pts',(1.40988938977465,-6.04871806075837,88.4285833675259));
#54224=CARTESIAN_POINT('Ctrl Pts',(5.85085964786324,-2.08379933077759,88.7070072211729));
#54225=CARTESIAN_POINT('Ctrl Pts',(4.91601590956152,3.79572994915096,88.9854310748201));
#54226=CARTESIAN_POINT('Ctrl Pts',(-0.535700343832902,6.1877139083478,89.2638549284673));
#54227=CARTESIAN_POINT('Ctrl Pts',(-5.49521107879562,2.89437963464127,89.5422787821142));
#54228=CARTESIAN_POINT('Ctrl Pts',(-5.40568040643315,-3.05833248902866,
89.8207026357616));
#54229=CARTESIAN_POINT('Ctrl Pts',(-0.349369784131343,-6.20102564289808,
90.0991264894084));
#54230=CARTESIAN_POINT('Ctrl Pts',(5.02794443225523,-3.64616964170593,90.3775503430558));
#54231=CARTESIAN_POINT('Ctrl Pts',(5.7855453622596,2.25881454112108,90.6559741967028));
#54232=CARTESIAN_POINT('Ctrl Pts',(1.22734355436289,6.08838287803152,90.93439805035));
#54233=CARTESIAN_POINT('Ctrl Pts',(-4.45855077309947,4.32389908226804,91.2128219039971));
#54234=CARTESIAN_POINT('Ctrl Pts',(-6.04789500498758,-1.41341581942115,
91.4912457576442));
#54235=CARTESIAN_POINT('Ctrl Pts',(-2.08038766748531,-5.852073600265,91.7696696112914));
#54236=CARTESIAN_POINT('Ctrl Pts',(3.79859555798657,-4.91380199609103,92.0480934649385));
#54237=CARTESIAN_POINT('Ctrl Pts',(6.18740051970406,0.539307962772255,92.3265173185856));
#54238=CARTESIAN_POINT('Ctrl Pts',(2.89117519236893,5.49689769569843,92.6049411722327));
#54239=CARTESIAN_POINT('Ctrl Pts',(-3.0614837191883,5.40389634496153,92.8833650258799));
#54240=CARTESIAN_POINT('Ctrl Pts',(-6.20122828689443,0.345754253428334,
93.161788879527));
#54241=CARTESIAN_POINT('Ctrl Pts',(-3.64323750870601,-5.03006945529593,
93.4402127331742));
#54242=CARTESIAN_POINT('Ctrl Pts',(2.26218738519033,-5.78422739043248,93.7186365868212));
#54243=CARTESIAN_POINT('Ctrl Pts',(6.08909743858714,-1.22379355012835,93.9970604404684));
#54244=CARTESIAN_POINT('Ctrl Pts',(4.32129881567914,4.46107103906154,94.2754842941155));
#54245=CARTESIAN_POINT('Ctrl Pts',(-1.41694176859032,6.04706989329276,94.5539081477627));
#54246=CARTESIAN_POINT('Ctrl Pts',(-5.85328556331033,2.07697529698528,94.8323320014097));
#54247=CARTESIAN_POINT('Ctrl Pts',(-4.91158641222056,-3.80145987552598,
95.110755855057));
#54248=CARTESIAN_POINT('Ctrl Pts',(0.542915398379021,-6.18708502771268,
95.389179708704));
#54249=CARTESIAN_POINT('Ctrl Pts',(5.49858244398346,-2.88796976726925,95.6676035623512));
#54250=CARTESIAN_POINT('Ctrl Pts',(5.40211044648703,3.06463390862584,95.9460274159983));
#54251=CARTESIAN_POINT('Ctrl Pts',(0.342138605189483,6.20142882284257,96.2244512696454));
#54252=CARTESIAN_POINT('Ctrl Pts',(-5.03219276841277,3.64030413722229,96.5028751232926));
#54253=CARTESIAN_POINT('Ctrl Pts',(-5.78290745231255,-2.26555946025075,
96.7812989769397));
#54254=CARTESIAN_POINT('Ctrl Pts',(-1.2202431298768,-6.0898099292123,97.0597228305868));
#54255=CARTESIAN_POINT('Ctrl Pts',(4.4635897885253,-4.31869708010603,97.3381466842341));
#54256=CARTESIAN_POINT('Ctrl Pts',(6.04624272595434,1.42046723608385,97.6165705378809));
#54257=CARTESIAN_POINT('Ctrl Pts',(2.07356222043732,5.85449553658713,97.8949943915284));
#54258=CARTESIAN_POINT('Ctrl Pts',(-3.80432290079535,4.90936915870336,98.1734182451752));
#54259=CARTESIAN_POINT('Ctrl Pts',(-6.18676743248101,-0.546522649426795,
98.4518420988226));
#54260=CARTESIAN_POINT('Ctrl Pts',(-2.88476336043193,-5.50026532307788,
98.7302659524695));
#54261=CARTESIAN_POINT('Ctrl Pts',(3.06778305627027,-5.40032271161683,99.0086898061168));
#54262=CARTESIAN_POINT('Ctrl Pts',(6.20162725067434,-0.338522840644003,
99.2871136597637));
#54263=CARTESIAN_POINT('Ctrl Pts',(3.637369528252,5.03431437088382,99.5655375134111));
#54264=CARTESIAN_POINT('Ctrl Pts',(-2.2689307651559,5.78158554834853,99.8439613670581));
#54265=CARTESIAN_POINT('Ctrl Pts',(-6.09052034966483,1.21669229481527,100.122385220705));
#54266=CARTESIAN_POINT('Ctrl Pts',(-4.31609387643315,-4.4661070206344,100.400809074352));
#54267=CARTESIAN_POINT('Ctrl Pts',(1.42399222070312,-6.04541350325356,100.679232928));
#54268=CARTESIAN_POINT('Ctrl Pts',(5.85570351968426,-2.07014843900163,100.957656781647));
#54269=CARTESIAN_POINT('Ctrl Pts',(4.90715023629299,3.80718463282164,101.236080635294));
#54270=CARTESIAN_POINT('Ctrl Pts',(-0.550129714689517,6.18644773411688,
101.514504488941));
#54271=CARTESIAN_POINT('Ctrl Pts',(-5.50194633240983,2.88155597294684,101.792928342588));
#54272=CARTESIAN_POINT('Ctrl Pts',(-5.39853314095852,-3.07093116105133,
102.071352196235));
#54273=CARTESIAN_POINT('Ctrl Pts',(-0.334906961020913,-6.20182357032214,
102.349776049882));
#54274=CARTESIAN_POINT('Ctrl Pts',(5.03643426198777,-3.63443368279287,102.628199903529));
#54275=CARTESIAN_POINT('Ctrl Pts',(5.78026167898992,2.27230129875968,102.906623757177));
#54276=CARTESIAN_POINT('Ctrl Pts',(1.21314104615092,6.09122869970316,103.185047610824));
#54277=CARTESIAN_POINT('Ctrl Pts',(-4.46862273453304,4.31348920554555,103.463471464471));
#54278=CARTESIAN_POINT('Ctrl Pts',(-6.04458222547238,-1.42751672124976,
103.741895318118));
#54279=CARTESIAN_POINT('Ctrl Pts',(-2.06673395383878,-5.85690951219101,
104.020319171765));
#54280=CARTESIAN_POINT('Ctrl Pts',(3.81004507063194,-4.90492964574384,104.298743025412));
#54281=CARTESIAN_POINT('Ctrl Pts',(6.18612593272902,0.553736592940906,104.577166879059));
#54282=CARTESIAN_POINT('Ctrl Pts',(2.87834760590436,5.50362547140775,104.855590732706));
#54283=CARTESIAN_POINT('Ctrl Pts',(-3.07407822189872,5.39674173512051,105.134014586354));
#54284=CARTESIAN_POINT('Ctrl Pts',(-6.20201778171941,0.3312909675493,105.412438440001));
#54285=CARTESIAN_POINT('Ctrl Pts',(-3.63149660184265,-5.03855244100415,
105.690862293648));
#54286=CARTESIAN_POINT('Ctrl Pts',(2.27567105991644,-5.77893584468655,105.969286147295));
#54287=CARTESIAN_POINT('Ctrl Pts',(6.09193497908663,-1.20958938509078,106.247710000942));
#54288=CARTESIAN_POINT('Ctrl Pts',(4.31088306832845,4.47113692936624,106.526133854589));
#54289=CARTESIAN_POINT('Ctrl Pts',(-1.43104073652573,6.04374889289317,106.804557708236));
#54290=CARTESIAN_POINT('Ctrl Pts',(-5.85811351369734,2.06331876610964,107.082981561883));
#54291=CARTESIAN_POINT('Ctrl Pts',(-4.90270738781089,-3.81290421325383,
107.361405415531));
#54292=CARTESIAN_POINT('Ctrl Pts',(0.557343282954733,-6.18580202842678,
107.639829269178));
#54293=CARTESIAN_POINT('Ctrl Pts',(5.50530273950077,-2.87513826039528,107.918253122825));
#54294=CARTESIAN_POINT('Ctrl Pts',(5.39494849471189,3.07722423774255,108.196676976472));
#54295=CARTESIAN_POINT('Ctrl Pts',(0.327674861458482,6.20220988480007,108.475100830119));
#54296=CARTESIAN_POINT('Ctrl Pts',(-5.04066890721283,3.6285582863999,108.753524683766));
#54297=CARTESIAN_POINT('Ctrl Pts',(-5.77760804588923,-2.27904004748059,
109.031948537413));
#54298=CARTESIAN_POINT('Ctrl Pts',(-1.20603731284231,-6.0926391875751,109.310372391061));
#54299=CARTESIAN_POINT('Ctrl Pts',(4.47364960427921,-4.3082754656679,109.588796244708));
#54300=CARTESIAN_POINT('Ctrl Pts',(6.04291350579938,1.4345642653332,109.867220098355));
#54301=CARTESIAN_POINT('Ctrl Pts',(2.05990287697488,5.85931552379407,110.145643952002));
#54302=CARTESIAN_POINT('Ctrl Pts',(-3.81576205971545,4.90048346324935,110.424067805649));
#54303=CARTESIAN_POINT('Ctrl Pts',(-6.18547602132036,-0.560949783505152,
110.702491659296));
#54304=CARTESIAN_POINT('Ctrl Pts',(-2.87192793751032,-5.50697813611887,
110.980915512943));
#54305=CARTESIAN_POINT('Ctrl Pts',(3.08036920751339,-5.39315342034202,111.259339366591));
#54306=CARTESIAN_POINT('Ctrl Pts',(6.2023998794988,-0.324058643977884,111.537763220238));
#54307=CARTESIAN_POINT('Ctrl Pts',(3.62561873746359,5.04278365989433,111.816187073885));
#54308=CARTESIAN_POINT('Ctrl Pts',(-2.28240826030677,5.7762782830493,112.094610927532));
#54309=CARTESIAN_POINT('Ctrl Pts',(-6.09334132492911,1.20248483061314,112.373034781179));
#54310=CARTESIAN_POINT('Ctrl Pts',(-4.30566639845044,-4.47616075841778,
112.651458634826));
#54311=CARTESIAN_POINT('Ctrl Pts',(1.43808730647429,-6.04207606447495,112.929882488473));
#54312=CARTESIAN_POINT('Ctrl Pts',(5.86051554207254,-2.05648628759585,113.20830634212));
#54313=CARTESIAN_POINT('Ctrl Pts',(4.89825787281534,3.81861860904526,113.486730195767));
#54314=CARTESIAN_POINT('Ctrl Pts',(-0.564556093366052,6.18514791152054,
113.765154049415));
#54315=CARTESIAN_POINT('Ctrl Pts',(-5.50865166069243,2.86871663834093,114.043577903062));
#54316=CARTESIAN_POINT('Ctrl Pts',(-5.39135651262125,-3.0835131301423,114.322001756709));
#54317=CARTESIAN_POINT('Ctrl Pts',(-0.320442316336498,-6.20258776575104,
114.600425610356));
#54318=CARTESIAN_POINT('Ctrl Pts',(5.04489669832976,-3.62267795603275,114.878849464003));
#54319=CARTESIAN_POINT('Ctrl Pts',(5.77494655661886,2.2857756972502,115.15727331765));
#54320=CARTESIAN_POINT('Ctrl Pts',(1.19893193961059,6.09404139091007,115.435697171297));
#54321=CARTESIAN_POINT('Ctrl Pts',(-4.47867039092821,4.30305586756279,115.714121024945));
#54322=CARTESIAN_POINT('Ctrl Pts',(-6.0412365692046,-1.4416098587512,115.992544878592));
#54323=CARTESIAN_POINT('Ctrl Pts',(-2.05306899913409,-5.86171356812484,
116.270968732239));
#54324=CARTESIAN_POINT('Ctrl Pts',(3.82147386027209,-4.89603061726545,116.549392585886));
#54325=CARTESIAN_POINT('Ctrl Pts',(6.18481769913886,0.568162211311366,116.827816439533));
#54326=CARTESIAN_POINT('Ctrl Pts',(2.8655043639789,5.51032331265255,117.10624029318));
#54327=CARTESIAN_POINT('Ctrl Pts',(-3.08665600456044,5.3895577721604,117.384664146827));
#54328=CARTESIAN_POINT('Ctrl Pts',(-6.20277354349289,0.316825879763828,
117.663088000474));
#54329=CARTESIAN_POINT('Ctrl Pts',(-3.61973594310723,-5.04700802180085,
117.941511854122));
#54330=CARTESIAN_POINT('Ctrl Pts',(2.28914235716608,-5.77361286705054,118.219935707769));
#54331=CARTESIAN_POINT('Ctrl Pts',(6.0947393852799,-1.19537864104265,118.498359561416));
#54332=CARTESIAN_POINT('Ctrl Pts',(4.30044387389252,4.48117850095767,118.776783415063));
#54333=CARTESIAN_POINT('Ctrl Pts',(-1.44513192096696,6.0403950202735,119.05520726871));
#54334=CARTESIAN_POINT('Ctrl Pts',(-5.86290960154331,2.04965101275129,119.333631122357));
#54335=CARTESIAN_POINT('Ctrl Pts',(-4.89380169735742,-3.824327812426,119.612054976004));
#54336=CARTESIAN_POINT('Ctrl Pts',(0.571768136116752,-6.18448538428672,
119.890478829651));
#54337=CARTESIAN_POINT('Ctrl Pts',(5.51199309142856,-2.8622911155176,120.168902683299));
#54338=CARTESIAN_POINT('Ctrl Pts',(5.38775719957539,3.08979782970226,120.447326536946));
#54339=CARTESIAN_POINT('Ctrl Pts',(0.31320933548108,6.20295721265561,120.725750390593));
#54340=CARTESIAN_POINT('Ctrl Pts',(-5.04911762957415,3.61679269969782,121.00417424424));
#54341=CARTESIAN_POINT('Ctrl Pts',(-5.77227721482724,-2.29250823892995,
121.282598097887));
#54342=CARTESIAN_POINT('Ctrl Pts',(-1.19182493606175,-6.09543530776335,
121.561021951534));
#54343=CARTESIAN_POINT('Ctrl Pts',(4.48368508754851,-4.29783041839939,121.839445805182));
#54344=CARTESIAN_POINT('Ctrl Pts',(6.03955141816593,1.44865349205967,122.117869658828));
#54345=CARTESIAN_POINT('Ctrl Pts',(2.04623232923532,5.86410364166548,122.396293512476));
#54346=CARTESIAN_POINT('Ctrl Pts',(-3.82718046383023,4.89157111433223,122.674717366123));
#54347=CARTESIAN_POINT('Ctrl Pts',(-6.18415096841107,-0.575373867468753,
122.95314121977));
#54348=CARTESIAN_POINT('Ctrl Pts',(-2.85907689153052,-5.51366099473004,
123.231565073417));
#54349=CARTESIAN_POINT('Ctrl Pts',(3.09293859974396,-5.38595479873152,123.509988927064));
#54350=CARTESIAN_POINT('Ctrl Pts',(6.203138782157,-0.309592678574449,123.788412780711));
#54351=CARTESIAN_POINT('Ctrl Pts',(3.61384820984823,5.0512255093335,124.066836634358));
#54352=CARTESIAN_POINT('Ctrl Pts',(-2.29587330938013,5.77093962230462,124.345260488006));
#54353=CARTESIAN_POINT('Ctrl Pts',(-6.09612921857968,1.18827078452085,124.623684341653));
#54354=CARTESIAN_POINT('Ctrl Pts',(-4.29521538781869,-4.48619007176196,
124.9021081953));
#54355=CARTESIAN_POINT('Ctrl Pts',(1.45217435528767,-6.03870591061202,125.180532048947));
#54356=CARTESIAN_POINT('Ctrl Pts',(5.86529609507713,-2.04281267134551,125.458955902594));
#54357=CARTESIAN_POINT('Ctrl Pts',(4.88933810046496,3.83003128783364,125.737379756241));
#54358=CARTESIAN_POINT('Ctrl Pts',(-0.578977953088837,6.18381544421881,
126.015803609888));
#54359=CARTESIAN_POINT('Ctrl Pts',(-5.51532976187251,2.85585981889264,126.294227463536));
#54360=CARTESIAN_POINT('Ctrl Pts',(-5.384145396786,-3.09607477471346,126.572651317182));
#54361=CARTESIAN_POINT('Ctrl Pts',(-0.305985678809838,-6.20332493410653,
126.85107517083));
#54362=CARTESIAN_POINT('Ctrl Pts',(5.05335010534642,-3.6108898572602,127.129499024477));
#54363=CARTESIAN_POINT('Ctrl Pts',(5.76956526204834,2.29921374333548,127.407922878124));
#54364=CARTESIAN_POINT('Ctrl Pts',(1.18478194982891,6.09686610220261,127.686346731771));
#54365=CARTESIAN_POINT('Ctrl Pts',(-4.4888176256727,4.29251384208693,127.964770585418));
#54366=CARTESIAN_POINT('Ctrl Pts',(-6.03762402993717,-1.45553411816505,
128.243194439065));
#54367=CARTESIAN_POINT('Ctrl Pts',(-2.03983479797794,-5.86678985768713,
128.521618292712));
#54368=CARTESIAN_POINT('Ctrl Pts',(3.8337165824916,-4.88653035923571,128.80004214636));
#54369=CARTESIAN_POINT('Ctrl Pts',(6.1818974004875,0.58149677391166,129.078466000007));
#54370=CARTESIAN_POINT('Ctrl Pts',(2.85564479853464,5.51907004802257,129.356889853654));
#54371=CARTESIAN_POINT('Ctrl Pts',(-3.1050343009106,5.37821806774232,129.635313707301));
#54372=CARTESIAN_POINT('Ctrl Pts',(-5.67690060144359,1.15622068272167,129.86733358534));
#54373=CARTESIAN_POINT('Ctrl Pts',(-4.91510296356909,-2.38887809660516,
130.052949487772));
#54374=CARTESIAN_POINT('Ctrl Pts',(-3.76253054062033,-3.76598540426341,
130.145757438987));
#54375=CARTESIAN_POINT('Ctrl Pts',(-3.05041111877786,-4.27420965560272,
130.192161414595));
#54376=CARTESIAN_POINT('Ctrl Pts',(-3.96383248548561,-3.93295783950028,
-9.66287555531569));
#54377=CARTESIAN_POINT('Ctrl Pts',(-3.30856849787929,-4.59336580384622,
-9.61647157970784));
#54378=CARTESIAN_POINT('Ctrl Pts',(-1.66601391597817,-5.567339035329,-9.52366362849213));
#54379=CARTESIAN_POINT('Ctrl Pts',(2.18501855494821,-5.7601574796524,-9.3380477260607));
#54380=CARTESIAN_POINT('Ctrl Pts',(6.17595083223459,-2.33837851004803,-9.10602784802143));
#54381=CARTESIAN_POINT('Ctrl Pts',(5.30367297041469,3.9415905605293,-8.82760399437431));
#54382=CARTESIAN_POINT('Ctrl Pts',(-0.447670556531286,6.58755408496995,
-8.54918014072716));
#54383=CARTESIAN_POINT('Ctrl Pts',(-5.7846197819851,3.18729356865408,-8.27075628708006));
#54384=CARTESIAN_POINT('Ctrl Pts',(-5.80822952673516,-3.14488847180297,
-7.9923324334329));
#54385=CARTESIAN_POINT('Ctrl Pts',(-0.494341668036604,-6.58571795329654,
-7.71390857978579));
#54386=CARTESIAN_POINT('Ctrl Pts',(5.27329977167003,-3.97649595721956,-7.43548472613864));
#54387=CARTESIAN_POINT('Ctrl Pts',(6.19603255906839,2.28686674054138,-7.15706087249153));
#54388=CARTESIAN_POINT('Ctrl Pts',(1.42567731735158,6.44877093303202,-6.87863701884439));
#54389=CARTESIAN_POINT('Ctrl Pts',(-4.65453397724029,4.68563770779713,-6.60021316519726));
#54390=CARTESIAN_POINT('Ctrl Pts',(-6.45815982591155,-1.38276999509599,
-6.32178931155014));
#54391=CARTESIAN_POINT('Ctrl Pts',(-2.32796089266521,-6.18063836937714,
-6.043365457903));
#54392=CARTESIAN_POINT('Ctrl Pts',(3.94117612000835,-5.29971065946422,-5.76494160425588));
#54393=CARTESIAN_POINT('Ctrl Pts',(6.58913604537669,0.450642366606509,-5.48651775060875));
#54394=CARTESIAN_POINT('Ctrl Pts',(3.18294525663012,5.78693587022664,-5.20809389696161));
#54395=CARTESIAN_POINT('Ctrl Pts',(-3.14775817423433,5.80615215953137,-4.92967004331449));
#54396=CARTESIAN_POINT('Ctrl Pts',(-6.58627842414191,0.490630370955284,
-4.65124618966736));
#54397=CARTESIAN_POINT('Ctrl Pts',(-3.9732759415693,-5.27568542617564,-4.37282233602023));
#54398=CARTESIAN_POINT('Ctrl Pts',(2.29040223968931,-6.19466210755678,-4.0943984823731));
#54399=CARTESIAN_POINT('Ctrl Pts',(6.4496416755637,-1.42193625171373,-3.81597462872597));
#54400=CARTESIAN_POINT('Ctrl Pts',(4.68290160783284,4.65727523193867,-3.53755077507883));
#54401=CARTESIAN_POINT('Ctrl Pts',(-1.38652376279582,6.45734715674067,-3.25912692143171));
#54402=CARTESIAN_POINT('Ctrl Pts',(-6.1820006544225,2.32435974869207,-2.98070306778457));
#54403=CARTESIAN_POINT('Ctrl Pts',(-5.29740868481312,-3.94426691722004,
-2.70227921413745));
#54404=CARTESIAN_POINT('Ctrl Pts',(0.454482355020498,-6.58887138551255,
-2.42385536049032));
#54405=CARTESIAN_POINT('Ctrl Pts',(5.78879157999998,-3.17957109821796,-2.14543150684319));
#54406=CARTESIAN_POINT('Ctrl Pts',(5.80431541636219,3.15114310501463,-1.86700765319606));
#54407=CARTESIAN_POINT('Ctrl Pts',(0.486790448190714,6.58656324563387,-1.58858379954893));
#54408=CARTESIAN_POINT('Ctrl Pts',(-5.27800125759252,3.97019937163456,-1.3101599459018));
#54409=CARTESIAN_POINT('Ctrl Pts',(-6.19332557868541,-2.29401364463305,
-1.03173609225467));
#54410=CARTESIAN_POINT('Ctrl Pts',(-1.41817562192872,-6.45046961328342,
-0.753312238607539));
#54411=CARTESIAN_POINT('Ctrl Pts',(4.66000479819239,-4.68018542440052,-0.474888384960414));
#54412=CARTESIAN_POINT('Ctrl Pts',(6.4565376442355,1.39028845011451,-0.196464531313281));
#54413=CARTESIAN_POINT('Ctrl Pts',(2.32075498025171,6.18335480526133,0.0819593223338455));
#54414=CARTESIAN_POINT('Ctrl Pts',(-3.94735487254703,5.29510810429758,0.360383175980979));
#54415=CARTESIAN_POINT('Ctrl Pts',(-6.58860528079665,-0.458323880989896,
0.638807029628107));
#54416=CARTESIAN_POINT('Ctrl Pts',(-3.17619543792065,-5.79064442581137,
0.917230883275238));
#54417=CARTESIAN_POINT('Ctrl Pts',(3.15452674161993,-5.80247717465899,1.19565473692237));
#54418=CARTESIAN_POINT('Ctrl Pts',(6.58684594617458,-0.482950108602965,
1.4740785905695));
#54419=CARTESIAN_POINT('Ctrl Pts',(3.96712138952872,5.28031516169088,1.75250244421663));
#54420=CARTESIAN_POINT('Ctrl Pts',(-2.29762423662747,6.19198701494913,2.03092629786376));
#54421=CARTESIAN_POINT('Ctrl Pts',(-6.45129537576889,1.41441447271307,2.30935015151089));
#54422=CARTESIAN_POINT('Ctrl Pts',(-4.67746764069405,-4.66273276054907,
2.58777400515801));
#54423=CARTESIAN_POINT('Ctrl Pts',(1.39405265989795,-6.45572594736398,2.86619785880515));
#54424=CARTESIAN_POINT('Ctrl Pts',(6.18470685673347,-2.31714941734695,3.14462171245227));
#54425=CARTESIAN_POINT('Ctrl Pts',(5.29280572238075,3.95044148307134,3.42304556609941));
#54426=CARTESIAN_POINT('Ctrl Pts',(-0.462165250425673,6.58833693790293,
3.70146941974653));
#54427=CARTESIAN_POINT('Ctrl Pts',(-5.79249530353563,3.17281869708231,3.97989327339367));
#54428=CARTESIAN_POINT('Ctrl Pts',(-5.80063696025417,-3.15790930543777,
4.25831712704079));
#54429=CARTESIAN_POINT('Ctrl Pts',(-0.479109604949533,-6.5871264078111,
4.53674098068793));
#54430=CARTESIAN_POINT('Ctrl Pts',(5.28262727085413,-3.96404205871552,4.81516483433505));
#54431=CARTESIAN_POINT('Ctrl Pts',(6.19064634627567,2.30123404750168,5.09358868798219));
#54432=CARTESIAN_POINT('Ctrl Pts',(1.41065284269685,6.45211894523253,5.3720125416293));
#54433=CARTESIAN_POINT('Ctrl Pts',(-4.66545913786288,4.67474826690904,5.65043639527645));
#54434=CARTESIAN_POINT('Ctrl Pts',(-6.45491205592566,-1.39781639577693,
5.92886024892357));
#54435=CARTESIAN_POINT('Ctrl Pts',(-2.31354306675181,-6.18605680577878,
6.20728410257071));
#54436=CARTESIAN_POINT('Ctrl Pts',(3.95352675068213,-5.29050154122254,6.48570795621782));
#54437=CARTESIAN_POINT('Ctrl Pts',(6.58806635536644,0.466006462751344,6.76413180986496));
#54438=CARTESIAN_POINT('Ctrl Pts',(3.16944087767492,5.79434421215727,7.04255566351209));
#54439=CARTESIAN_POINT('Ctrl Pts',(-3.1612907957547,5.79879477397794,7.32097951715922));
#54440=CARTESIAN_POINT('Ctrl Pts',(-6.58740463021691,0.47526893842755,7.59940337080635));
#54441=CARTESIAN_POINT('Ctrl Pts',(-3.96096138036421,-5.28493758423886,
7.87782722445348));
#54442=CARTESIAN_POINT('Ctrl Pts',(2.30484307609341,-6.18930357315113,8.1562510781006));
#54443=CARTESIAN_POINT('Ctrl Pts',(6.45294032136004,-1.40689073314278,8.43467493174774));
#54444=CARTESIAN_POINT('Ctrl Pts',(4.6720273039881,4.66818392919851,8.71309878539486));
#54445=CARTESIAN_POINT('Ctrl Pts',(-1.40157965648158,6.45409597020173,8.991522639042));
#54446=CARTESIAN_POINT('Ctrl Pts',(-6.18740465193323,2.30993592968984,9.26994649268913));
#54447=CARTESIAN_POINT('Ctrl Pts',(-5.28819556160898,-3.95661067432928,
9.54837034633626));
#54448=CARTESIAN_POINT('Ctrl Pts',(0.469847516662575,-6.58779353327983,
9.82679419998338));
#54449=CARTESIAN_POINT('Ctrl Pts',(5.79619115104702,-3.16606198084645,10.1052180536305));
#54450=CARTESIAN_POINT('Ctrl Pts',(5.79695061645688,3.16467121142106,10.3836419072777));
#54451=CARTESIAN_POINT('Ctrl Pts',(0.471428110342511,6.58768061329754,10.6620657609248));
#54452=CARTESIAN_POINT('Ctrl Pts',(-5.28724610105964,3.95787935552199,10.9404896145719));
#54453=CARTESIAN_POINT('Ctrl Pts',(-6.18795869603207,-2.30845132117582,
11.218913468219));
#54454=CARTESIAN_POINT('Ctrl Pts',(-1.4031281453296,-6.45375950387221,11.4973373218662));
#54455=CARTESIAN_POINT('Ctrl Pts',(4.67090713362965,-4.66930475285615,11.7757611755133));
#54456=CARTESIAN_POINT('Ctrl Pts',(6.45327769046963,1.40534244073263,12.0541850291604));
#54457=CARTESIAN_POINT('Ctrl Pts',(2.30632800738723,6.1887503947387,12.3326088828076));
#54458=CARTESIAN_POINT('Ctrl Pts',(-3.95969325296453,5.28588778432387,12.6110327364547));
#54459=CARTESIAN_POINT('Ctrl Pts',(-6.58751847173579,-0.473688410853622,
12.8894565901018));
#54460=CARTESIAN_POINT('Ctrl Pts',(-3.16268200774551,-5.79803611957706,
13.1678804437489));
#54461=CARTESIAN_POINT('Ctrl Pts',(3.16805055128777,-5.79510448831792,13.4463042973961));
#54462=CARTESIAN_POINT('Ctrl Pts',(6.58795435695914,-0.467587121999925,
13.7247281510432));
#54463=CARTESIAN_POINT('Ctrl Pts',(3.95479598523653,5.28955282053166,14.0031520046903));
#54464=CARTESIAN_POINT('Ctrl Pts',(-2.31205878152226,6.18661171537565,14.2815758583375));
#54465=CARTESIAN_POINT('Ctrl Pts',(-6.45457649249062,1.39936508053644,14.5599997119846));
#54466=CARTESIAN_POINT('Ctrl Pts',(-4.66658061443868,-4.67362875023062,
14.8384235656317));
#54467=CARTESIAN_POINT('Ctrl Pts',(1.40910474725094,-6.45245721700749,15.1168474192789));
#54468=CARTESIAN_POINT('Ctrl Pts',(6.19009403373768,-2.30271930107051,15.3952712729259));
#54469=CARTESIAN_POINT('Ctrl Pts',(5.28357821015179,3.96277448553996,15.6736951265731));
#54470=CARTESIAN_POINT('Ctrl Pts',(-0.477529144018868,6.58724117082786,
15.9521189802202));
#54471=CARTESIAN_POINT('Ctrl Pts',(-5.79987911712016,3.15930095952108,16.2305428338674));
#54472=CARTESIAN_POINT('Ctrl Pts',(-5.79325639018865,-3.17142881420597,
16.5089666875145));
#54473=CARTESIAN_POINT('Ctrl Pts',(-0.463745974705563,-6.58822586110871,
16.7873905411617));
#54474=CARTESIAN_POINT('Ctrl Pts',(5.2918577418708,-3.95171127055596,17.0658143948087));
#54475=CARTESIAN_POINT('Ctrl Pts',(6.18526263163975,2.31566545590642,17.3442382484559));
#54476=CARTESIAN_POINT('Ctrl Pts',(1.39560154004253,6.45539128693748,17.622662102103));
#54477=CARTESIAN_POINT('Ctrl Pts',(-4.67634877807622,4.6638548896618,17.9010859557501));
#54478=CARTESIAN_POINT('Ctrl Pts',(-6.45163455009424,-1.41286657475762,
18.1795098093973));
#54479=CARTESIAN_POINT('Ctrl Pts',(-2.29910981196639,-6.19143556847337,
18.4579336630444));
#54480=CARTESIAN_POINT('Ctrl Pts',(3.96585437100808,-5.28126683987788,18.7363575166915));
#54481=CARTESIAN_POINT('Ctrl Pts',(6.58696163065034,0.481369714852657,19.0147813703387));
#54482=CARTESIAN_POINT('Ctrl Pts',(3.15591883732246,5.80172014304984,19.2932052239858));
#54483=CARTESIAN_POINT('Ctrl Pts',(-3.17480599902726,5.79140632269727,19.5716290776329));
#54484=CARTESIAN_POINT('Ctrl Pts',(-6.58849512565393,0.459904669765239,
19.85005293128));
#54485=CARTESIAN_POINT('Ctrl Pts',(-3.94862521252898,-5.29416086429357,
20.1284767849272));
#54486=CARTESIAN_POINT('Ctrl Pts',(2.3192713431023,-6.18391144528296,20.4069006385743));
#54487=CARTESIAN_POINT('Ctrl Pts',(6.45620388693581,-1.39183752512723,20.6853244922214));
#54488=CARTESIAN_POINT('Ctrl Pts',(4.6611275794521,4.67906721624177,20.9637483458686));
#54489=CARTESIAN_POINT('Ctrl Pts',(-1.41662792197383,6.45080969000957,21.2421721995157));
#54490=CARTESIAN_POINT('Ctrl Pts',(-6.19277499848978,2.29549954130184,21.5205960531628));
#54491=CARTESIAN_POINT('Ctrl Pts',(-5.27895367428779,-3.96893290832191,
21.79901990681));
#54492=CARTESIAN_POINT('Ctrl Pts',(0.48521012204937,-6.58667985129825,22.0774437604571));
#54493=CARTESIAN_POINT('Ctrl Pts',(5.80355919674031,-3.15253564229943,22.3558676141042));
#54494=CARTESIAN_POINT('Ctrl Pts',(5.78955428647267,3.17818210460365,22.6342914677513));
#54495=CARTESIAN_POINT('Ctrl Pts',(0.456063208484729,6.58876215050323,22.9127153213985));
#54496=CARTESIAN_POINT('Ctrl Pts',(-5.29646218701701,3.94553781220464,23.1911391750456));
#54497=CARTESIAN_POINT('Ctrl Pts',(-6.18255815676466,-2.32287644188415,
23.4695630286927));
#54498=CARTESIAN_POINT('Ctrl Pts',(-1.38807303706995,-6.4570142922094,23.7479868823399));
#54499=CARTESIAN_POINT('Ctrl Pts',(4.68178406380318,-4.65839868473658,24.026410735987));
#54500=CARTESIAN_POINT('Ctrl Pts',(6.44998263703386,1.42038878762094,24.3048345896342));
#54501=CARTESIAN_POINT('Ctrl Pts',(2.29188849030413,6.19411232333165,24.5832584432812));
#54502=CARTESIAN_POINT('Ctrl Pts',(-3.9720100964351,5.27663871416782,24.8616822969284));
#54503=CARTESIAN_POINT('Ctrl Pts',(-6.58639583286728,-0.489050364303604,
25.1401061505755));
#54504=CARTESIAN_POINT('Ctrl Pts',(-3.14915137560207,-5.80539627756634,
25.4185300042227));
#54505=CARTESIAN_POINT('Ctrl Pts',(3.18155712978754,-5.78770028214451,25.6969538578698));
#54506=CARTESIAN_POINT('Ctrl Pts',(6.58902693556586,-0.452221592169745,
25.9753777115169));
#54507=CARTESIAN_POINT('Ctrl Pts',(3.94244907063243,5.29876170925873,26.2538015651641));
#54508=CARTESIAN_POINT('Ctrl Pts',(-2.32648075102626,6.18120276654486,26.5322254188111));
#54509=CARTESIAN_POINT('Ctrl Pts',(-6.45782250248278,1.38430807715065,26.8106492724583));
#54510=CARTESIAN_POINT('Ctrl Pts',(-4.65566820644302,-4.68449931983693,
27.0890731261054));
#54511=CARTESIAN_POINT('Ctrl Pts',(1.42414917042049,-6.44915339144822,27.3674969797525));
#54512=CARTESIAN_POINT('Ctrl Pts',(6.19544754254423,-2.28827666020089,27.6459208333997));
#54513=CARTESIAN_POINT('Ctrl Pts',(5.27432196030506,3.97508593430139,27.9243446870468));
#54514=CARTESIAN_POINT('Ctrl Pts',(-0.49289044030986,6.5861095754541,28.202768540694));
#54515=CARTESIAN_POINT('Ctrl Pts',(-5.80723138490337,3.14576603838083,28.481192394341));
#54516=CARTESIAN_POINT('Ctrl Pts',(-5.78584431034302,-3.18493107343138,
28.7596162479882));
#54517=CARTESIAN_POINT('Ctrl Pts',(-0.448379822126494,-6.58928948075187,
29.0380401016353));
#54518=CARTESIAN_POINT('Ctrl Pts',(5.30105943023716,-3.93935898886236,29.3164639552825));
#54519=CARTESIAN_POINT('Ctrl Pts',(6.17984527508429,2.33008426930356,29.5948878089296));
#54520=CARTESIAN_POINT('Ctrl Pts',(1.380542646649,6.45862851748116,29.8733116625768));
#54521=CARTESIAN_POINT('Ctrl Pts',(-4.68721298341994,4.65293614549958,30.1517355162238));
#54522=CARTESIAN_POINT('Ctrl Pts',(-6.44832195353458,-1.42790906909408,
30.430159369871));
#54523=CARTESIAN_POINT('Ctrl Pts',(-2.28466405221999,-6.19678065567362,
30.7085832235181));
#54524=CARTESIAN_POINT('Ctrl Pts',(3.97816042087516,-5.27200341348711,30.9870070771652));
#54525=CARTESIAN_POINT('Ctrl Pts',(6.58582107915601,0.496730348762664,31.2654309308124));
#54526=CARTESIAN_POINT('Ctrl Pts',(3.14237963178648,5.80906451812772,31.5438547844595));
#54527=CARTESIAN_POINT('Ctrl Pts',(-3.18830393438844,5.78398637169907,31.8222786381066));
#54528=CARTESIAN_POINT('Ctrl Pts',(-6.58954978597194,0.44453789966075,32.1007024917539));
#54529=CARTESIAN_POINT('Ctrl Pts',(-3.93626756794489,-5.30335534917115,
32.3791263454008));
#54530=CARTESIAN_POINT('Ctrl Pts',(2.33368699549094,-6.17848568284443,32.6575501990481));
#54531=CARTESIAN_POINT('Ctrl Pts',(6.4594323369305,-1.3767767468452,32.9359740526951));
#54532=CARTESIAN_POINT('Ctrl Pts',(4.65020250283515,4.68992505362966,33.2143979063423));
#54533=CARTESIAN_POINT('Ctrl Pts',(-1.43166848236366,6.44748832357563,33.4928217599894));
#54534=CARTESIAN_POINT('Ctrl Pts',(-6.19811166226677,2.28105066758929,33.7712456136365));
#54535=CARTESIAN_POINT('Ctrl Pts',(-5.26968307450193,-3.98123355511144,
34.0496694672837));
#54536=CARTESIAN_POINT('Ctrl Pts',(0.500570088356797,-6.58553034407101,
34.3280933209308));
#54537=CARTESIAN_POINT('Ctrl Pts',(5.81089567661615,-3.13899215697025,34.6065171745779));
#54538=CARTESIAN_POINT('Ctrl Pts',(5.78212646684429,3.19167571151203,34.8849410282251));
#54539=CARTESIAN_POINT('Ctrl Pts',(0.440695826078731,6.58980785113753,35.1633648818722));
#54540=CARTESIAN_POINT('Ctrl Pts',(-5.30564946528016,3.93317480893105,35.4417887355193));
#54541=CARTESIAN_POINT('Ctrl Pts',(-6.17712399028752,-2.33728892836378,
35.7202125891665));
#54542=CARTESIAN_POINT('Ctrl Pts',(-1.3730103790192,-6.46023396055767,35.9986364428136));
#54543=CARTESIAN_POINT('Ctrl Pts',(4.6926355295443,-4.64746727937873,36.2770602964607));
#54544=CARTESIAN_POINT('Ctrl Pts',(6.44665250185466,1.43542740895129,36.5554841501079));
#54545=CARTESIAN_POINT('Ctrl Pts',(2.27743650753725,6.19944056187117,36.833908003755));
#54546=CARTESIAN_POINT('Ctrl Pts',(-3.9843053359654,5.26736094413842,37.1123318574021));
#54547=CARTESIAN_POINT('Ctrl Pts',(-6.58523737029794,-0.504409657786784,
37.3907557110492));
#54548=CARTESIAN_POINT('Ctrl Pts',(-3.1356036150838,-5.81272485974614,37.6691795646963));
#54549=CARTESIAN_POINT('Ctrl Pts',(3.19504640365602,-5.78026459641099,37.9476034183435));
#54550=CARTESIAN_POINT('Ctrl Pts',(6.59006367616103,-0.436853602686241,
38.2260272719906));
#54551=CARTESIAN_POINT('Ctrl Pts',(3.93008071287194,5.30794177778444,38.5044511256378));
#54552=CARTESIAN_POINT('Ctrl Pts',(-2.34089006669765,6.17576019787637,38.7828749792849));
#54553=CARTESIAN_POINT('Ctrl Pts',(-6.4610333880901,1.36924354445145,39.061298832932));
#54554=CARTESIAN_POINT('Ctrl Pts',(-4.64473047606029,-4.69534441024232,
39.3397226865791));
#54555=CARTESIAN_POINT('Ctrl Pts',(1.43918584757895,-6.44581448865584,39.6181465402263));
#54556=CARTESIAN_POINT('Ctrl Pts',(6.20076735403504,-2.27382157329258,39.8965703938733));
#54557=CARTESIAN_POINT('Ctrl Pts',(5.26503702318596,3.98737576239292,40.1749942475206));
#54558=CARTESIAN_POINT('Ctrl Pts',(-0.508249055747655,6.58494215793644,
40.4534181011676));
#54559=CARTESIAN_POINT('Ctrl Pts',(-5.81455206689598,3.13221400727876,40.7318419548148));
#54560=CARTESIAN_POINT('Ctrl Pts',(-5.77840076103197,-3.19841600967458,
41.0102658084619));
#54561=CARTESIAN_POINT('Ctrl Pts',(-0.433011230789567,-6.59031726095543,
41.2886896621091));
#54562=CARTESIAN_POINT('Ctrl Pts',(5.31023228590465,-3.9269852808195,41.5671135157562));
#54563=CARTESIAN_POINT('Ctrl Pts',(6.17439430607461,2.34449040926819,41.8455373694033));
#54564=CARTESIAN_POINT('Ctrl Pts',(1.36547624442261,6.46183061925605,42.1239612230505));
#54565=CARTESIAN_POINT('Ctrl Pts',(-4.69805169480298,4.6419920938102,42.4023850766975));
#54566=CARTESIAN_POINT('Ctrl Pts',(-6.44497428426404,-1.4429437969693,42.6808089303448));
#54567=CARTESIAN_POINT('Ctrl Pts',(-2.2702058660839,-6.20209203830737,42.9592327839917));
#54568=CARTESIAN_POINT('Ctrl Pts',(3.99044483335022,-5.2627113124345,43.237656637639));
#54569=CARTESIAN_POINT('Ctrl Pts',(6.58464470708685,0.512088280934132,43.516080491286));
#54570=CARTESIAN_POINT('Ctrl Pts',(3.12882333470756,5.8163772974444,43.7945043449333));
#54571=CARTESIAN_POINT('Ctrl Pts',(-3.20178452842208,5.77653496134093,44.0729281985803));
#54572=CARTESIAN_POINT('Ctrl Pts',(-6.59056860543455,0.429168711694992,
44.3513520522275));
#54573=CARTESIAN_POINT('Ctrl Pts',(-3.92388851382601,-5.31252098886223,
44.6297759058746));
#54574=CARTESIAN_POINT('Ctrl Pts',(2.34808995485178,-6.17302631534656,44.9081997595216));
#54575=CARTESIAN_POINT('Ctrl Pts',(6.46262565378449,-1.36170848021304,45.1866236131689));
#54576=CARTESIAN_POINT('Ctrl Pts',(4.63925213355924,4.70075738230592,45.465047466816));
#54577=CARTESIAN_POINT('Ctrl Pts',(-1.4467012558447,6.4441318889649,45.7434713204631));
#54578=CARTESIAN_POINT('Ctrl Pts',(-6.20341461423781,2.26658938714048,46.0218951741103));
#54579=CARTESIAN_POINT('Ctrl Pts',(-5.26038381267472,-3.99351254779384,
46.3003190277573));
#54580=CARTESIAN_POINT('Ctrl Pts',(0.51592733204096,-6.58434501785033,46.5787428814046));
#54581=CARTESIAN_POINT('Ctrl Pts',(5.81820055077105,-3.12543159852284,46.8571667350516));
#54582=CARTESIAN_POINT('Ctrl Pts',(5.77466719797205,3.2051519587537,47.1355905886988));
#54583=CARTESIAN_POINT('Ctrl Pts',(0.425326046708484,6.59081770951289,47.4140144423458));
#54584=CARTESIAN_POINT('Ctrl Pts',(-5.31480788587913,3.92079041294412,47.6924382959931));
#54585=CARTESIAN_POINT('Ctrl Pts',(-6.17165622615728,-2.35168870222466,
47.9708621496401));
#54586=CARTESIAN_POINT('Ctrl Pts',(-1.35794025310373,-6.46341849140512,
48.2492860032874));
#54587=CARTESIAN_POINT('Ctrl Pts',(4.70346147183124,-4.63651059623897,48.5277098569344));
#54588=CARTESIAN_POINT('Ctrl Pts',(6.44328730304483,1.45045822292773,48.8061337105815));
#54589=CARTESIAN_POINT('Ctrl Pts',(2.26297213769171,6.20473508137685,49.0845575642287));
#54590=CARTESIAN_POINT('Ctrl Pts',(-3.9965789046812,5.25805452469773,49.3629814178758));
#54591=CARTESIAN_POINT('Ctrl Pts',(-6.58404309032867,-0.519766207763357,
49.641405271523));
#54592=CARTESIAN_POINT('Ctrl Pts',(-3.12203879987747,-5.82002182625609,
49.91982912517));
#54593=CARTESIAN_POINT('Ctrl Pts',(3.20851829952456,-5.7727974715603,50.1982529788172));
#54594=CARTESIAN_POINT('Ctrl Pts',(6.59106457310578,-0.421483237136511,
50.4766768324643));
#54595=CARTESIAN_POINT('Ctrl Pts',(3.91769097922709,5.31709297617784,50.7551006861114));
#54596=CARTESIAN_POINT('Ctrl Pts',(-2.35528665016334,6.17028403897258,51.0335245397587));
#54597=CARTESIAN_POINT('Ctrl Pts',(-6.46420913184854,1.35417156437564,51.3119483934057));
#54598=CARTESIAN_POINT('Ctrl Pts',(-4.6337674827812,-4.70616396245993,51.5903722470528));
#54599=CARTESIAN_POINT('Ctrl Pts',(1.45421469694148,-6.44244052679083,51.8687961006999));
#54600=CARTESIAN_POINT('Ctrl Pts',(6.20605343927554,-2.25935411896713,52.1472199543472));
#54601=CARTESIAN_POINT('Ctrl Pts',(5.25572344929541,3.99964390296978,52.4256438079942));
#54602=CARTESIAN_POINT('Ctrl Pts',(-0.523604906796155,6.58373892462452,
52.7040676616414));
#54603=CARTESIAN_POINT('Ctrl Pts',(-5.82184112328028,3.11864493992497,52.9824915152884));
#54604=CARTESIAN_POINT('Ctrl Pts',(-5.77092578274138,-3.21188354959022,
53.2609153689357));
#54605=CARTESIAN_POINT('Ctrl Pts',(-0.417640284285345,-6.59130919612937,
53.5393392225827));
#54606=CARTESIAN_POINT('Ctrl Pts',(5.31937625898175,-3.91459021372843,53.8177630762299));
#54607=CARTESIAN_POINT('Ctrl Pts',(6.16890975425877,2.35888379744498,54.096186929877));
#54608=CARTESIAN_POINT('Ctrl Pts',(1.35040241530983,6.46499757484586,54.3746107835242));
#54609=CARTESIAN_POINT('Ctrl Pts',(-4.70886485327322,4.63102279411851,54.6530346371712));
#54610=CARTESIAN_POINT('Ctrl Pts',(-6.44159156049077,-1.45797067660881,
54.9314584908185));
#54611=CARTESIAN_POINT('Ctrl Pts',(-2.25573533219686,-6.20736968748566,
55.2098823444655));
#54612=CARTESIAN_POINT('Ctrl Pts',(4.0027075416176,-5.25339058726029,55.4883061981127));
#54613=CARTESIAN_POINT('Ctrl Pts',(6.58343252084137,0.527443427834472,55.7667300517598));
#54614=CARTESIAN_POINT('Ctrl Pts',(3.11525001981887,5.82365844122538,56.0451539054069));
#54615=CARTESIAN_POINT('Ctrl Pts',(-3.2152477078069,5.76905213215134,56.323577759054));
#54616=CARTESIAN_POINT('Ctrl Pts',(-6.59155157850042,0.413797189461302,
56.6020016127012));
#54617=CARTESIAN_POINT('Ctrl Pts',(-3.91148811750227,-5.32165773351459,
56.8804254663483));
#54618=CARTESIAN_POINT('Ctrl Pts',(2.36248014284657,-6.1675333724831,57.1588493199955));
#54619=CARTESIAN_POINT('Ctrl Pts',(6.46578382012906,-1.34663280718776,57.4372731736426));
#54620=CARTESIAN_POINT('Ctrl Pts',(4.62827653118404,4.71156414335287,57.7156970272897));
#54621=CARTESIAN_POINT('Ctrl Pts',(-1.46172616065295,6.44074040443335,57.9941208809369));
#54622=CARTESIAN_POINT('Ctrl Pts',(-6.20868382555991,2.25211577861082,58.2725447345839));
#54623=CARTESIAN_POINT('Ctrl Pts',(-5.25105593938519,-4.00576981958337,
58.5509685882311));
#54624=CARTESIAN_POINT('Ctrl Pts',(0.531281769573442,-6.58312387908324,
58.8293924418782));
#54625=CARTESIAN_POINT('Ctrl Pts',(5.82547377947346,-3.11185404071339,59.1078162955253));
#54626=CARTESIAN_POINT('Ctrl Pts',(5.76717652042727,3.21861077303071,59.3862401491726));
#54627=CARTESIAN_POINT('Ctrl Pts',(0.409953953971075,6.59179172013654,59.6646640028195));
#54628=CARTESIAN_POINT('Ctrl Pts',(-5.32393739900074,3.90838469160332,59.9430878564668));
#54629=CARTESIAN_POINT('Ctrl Pts',(-6.1661548941135,-2.36607568514559,60.2215117101138));
#54630=CARTESIAN_POINT('Ctrl Pts',(-1.34286274129069,-6.46656786743093,
60.499935563761));
#54631=CARTESIAN_POINT('Ctrl Pts',(4.71426183178142,-4.62552869491119,60.7783594174081));
#54632=CARTESIAN_POINT('Ctrl Pts',(6.43988705890778,1.46548114779727,61.0567832710552));
#54633=CARTESIAN_POINT('Ctrl Pts',(2.24849545943964,6.20999585305146,61.3352071247024));
#54634=CARTESIAN_POINT('Ctrl Pts',(-4.00883073582598,5.24871950646391,61.6136309783494));
#54635=CARTESIAN_POINT('Ctrl Pts',(-6.58281299945516,-0.535119930708313,
61.8920548319967));
#54636=CARTESIAN_POINT('Ctrl Pts',(-3.10845700376283,-5.82728713740749,
62.1704786856437));
#54637=CARTESIAN_POINT('Ctrl Pts',(3.22197274411874,-5.76529894820667,62.448902539291));
#54638=CARTESIAN_POINT('Ctrl Pts',(6.59202962095616,-0.406110579120708,
62.7273263929379));
#54639=CARTESIAN_POINT('Ctrl Pts',(3.90527993708621,5.32621525466534,63.0057502465852));
#54640=CARTESIAN_POINT('Ctrl Pts',(-2.36967042311993,6.1647743196185,63.2841741002322));
#54641=CARTESIAN_POINT('Ctrl Pts',(-6.46734971648495,1.33909221890021,63.5625979538794));
#54642=CARTESIAN_POINT('Ctrl Pts',(-4.62277928623404,-4.71695791764177,
63.8410218075266));
#54643=CARTESIAN_POINT('Ctrl Pts',(1.46923563676534,-6.43903152420423,64.1194456611737));
#54644=CARTESIAN_POINT('Ctrl Pts',(6.21130576951436,-2.24487437591387,64.3978695148208));
#54645=CARTESIAN_POINT('Ctrl Pts',(5.24638128929058,4.01189028930497,64.6762933684679));
#54646=CARTESIAN_POINT('Ctrl Pts',(-0.538957909934277,6.58249988206277,
64.9547172221151));
#54647=CARTESIAN_POINT('Ctrl Pts',(-5.82909851441101,3.10505891012206,65.2331410757622));
#54648=CARTESIAN_POINT('Ctrl Pts',(-5.76341941612784,-3.22533361992796,
65.5115649294094));
#54649=CARTESIAN_POINT('Ctrl Pts',(-0.402267066216936,-6.59226528087837,
65.7899887830564));
#54650=CARTESIAN_POINT('Ctrl Pts',(5.32849129973403,-3.90217385500653,66.0684126367037));
#54651=CARTESIAN_POINT('Ctrl Pts',(6.16339164946744,2.37326435554747,66.3468364903507));
#54652=CARTESIAN_POINT('Ctrl Pts',(1.33532124129813,6.46812936702529,66.6252603439979));
#54653=CARTESIAN_POINT('Ctrl Pts',(-4.71965240001728,4.62002830608733,66.9036841976449));
#54654=CARTESIAN_POINT('Ctrl Pts',(-6.43817380061354,-1.47298962628067,
67.1821080512921));
#54655=CARTESIAN_POINT('Ctrl Pts',(-2.24125252926465,-6.2126135745033,67.4605319049392));
#54656=CARTESIAN_POINT('Ctrl Pts',(4.0149484789801,-5.24404128866014,67.7389557585864));
#54657=CARTESIAN_POINT('Ctrl Pts',(6.58218452701253,0.542795705946505,68.0173796122336));
#54658=CARTESIAN_POINT('Ctrl Pts',(3.10165976094634,5.83090790986826,68.2958034658805));
#54659=CARTESIAN_POINT('Ctrl Pts',(-3.22869339931589,5.76153792482971,68.5742273195278));
#54660=CARTESIAN_POINT('Ctrl Pts',(-6.59249869982305,0.398423416566328,
68.8526511731748));
#54661=CARTESIAN_POINT('Ctrl Pts',(-3.89906644642019,-5.33076553343308,
69.1310750268221));
#54662=CARTESIAN_POINT('Ctrl Pts',(2.3768574812065,-6.16200688413035,69.409498880469));
#54663=CARTESIAN_POINT('Ctrl Pts',(6.46890681878693,-1.33154980976638,69.6879227341164));
#54664=CARTESIAN_POINT('Ctrl Pts',(4.61727575540617,4.72234527799222,69.9663465877634));
#54665=CARTESIAN_POINT('Ctrl Pts',(-1.47674311506742,6.43731388842723,70.2447704414106));
#54666=CARTESIAN_POINT('Ctrl Pts',(-6.21391926757366,2.23762992072296,70.5231942950576));
#54667=CARTESIAN_POINT('Ctrl Pts',(-5.24169950536803,-4.01800530381204,
70.8016181487048));
#54668=CARTESIAN_POINT('Ctrl Pts',(0.546633317440691,-6.5818669344116,71.0800420023519));
#54669=CARTESIAN_POINT('Ctrl Pts',(5.83271532316402,-3.098259557391,71.358465855999));
#54670=CARTESIAN_POINT('Ctrl Pts',(5.75965447495197,3.23205208114023,71.6368897096462));
#54671=CARTESIAN_POINT('Ctrl Pts',(0.394579631475598,6.59272987771093,71.9153135632933));
#54672=CARTESIAN_POINT('Ctrl Pts',(-5.33303795498926,3.89595771238356,72.1937374169405));
#54673=CARTESIAN_POINT('Ctrl Pts',(-6.16062002407802,-2.38044979887542,
72.4721612705875));
#54674=CARTESIAN_POINT('Ctrl Pts',(-1.32777792558714,-6.46968207150563,
72.7505851242348));
#54675=CARTESIAN_POINT('Ctrl Pts',(4.72503655065108,-4.61452163512627,73.0290089778817));
#54676=CARTESIAN_POINT('Ctrl Pts',(6.43645178793764,1.48049610184946,73.3074328315291));
#54677=CARTESIAN_POINT('Ctrl Pts',(2.23400655152038,6.21522284828162,73.585856685176));
#54678=CARTESIAN_POINT('Ctrl Pts',(-4.0210607627615,5.2393559402103,73.8642805388233));
#54679=CARTESIAN_POINT('Ctrl Pts',(-6.58154710436798,-0.550470743112097,
74.1427043924703));
#54680=CARTESIAN_POINT('Ctrl Pts',(-3.09485830061189,-5.83452075368412,
74.4211282461175));
#54681=CARTESIAN_POINT('Ctrl Pts',(3.23540966425953,-5.7577690671347,74.6995520997645));
#54682=CARTESIAN_POINT('Ctrl Pts',(6.59295881446331,-0.390735712251194,
74.9779759534118));
#54683=CARTESIAN_POINT('Ctrl Pts',(3.89284765395332,5.33530856363034,75.2563998070588));
#54684=CARTESIAN_POINT('Ctrl Pts',(-2.38404130733335,6.15923106978178,75.534823660706));
#54685=CARTESIAN_POINT('Ctrl Pts',(-6.47045512491767,1.32400559004247,75.8132475143532));
#54686=CARTESIAN_POINT('Ctrl Pts',(-4.61176594618401,-4.72772621707885,
76.0916713680002));
#54687=CARTESIAN_POINT('Ctrl Pts',(1.48424858535093,-6.43558749943792,76.3700952216474));
#54688=CARTESIAN_POINT('Ctrl Pts',(6.21652431618393,-2.23038242288872,76.6485190752944));
#54689=CARTESIAN_POINT('Ctrl Pts',(5.23701059398374,4.0241148547897,76.9269429289418));
#54690=CARTESIAN_POINT('Ctrl Pts',(-0.554307981656129,6.58122503699047,
77.2053667825887));
#54691=CARTESIAN_POINT('Ctrl Pts',(-5.83632420081472,3.09145599176529,77.483790636236));
#54692=CARTESIAN_POINT('Ctrl Pts',(-5.75588170201891,-3.23876614753225,
77.762214489883));
#54693=CARTESIAN_POINT('Ctrl Pts',(-0.386891660199915,-6.5931855100024,
78.0406383435301));
#54694=CARTESIAN_POINT('Ctrl Pts',(5.33757735858429,-3.88973627218676,78.3190621971773));
#54695=CARTESIAN_POINT('Ctrl Pts',(6.15784002171388,2.38763200535924,78.5974860508244));
#54696=CARTESIAN_POINT('Ctrl Pts',(1.32023280441466,6.47122597876048,78.8759099044716));
#54697=CARTESIAN_POINT('Ctrl Pts',(-4.73041427636142,4.60900868951591,79.1543337581187));
#54698=CARTESIAN_POINT('Ctrl Pts',(-6.43472102322171,-1.48800056429638,
79.4327576117657));
#54699=CARTESIAN_POINT('Ctrl Pts',(-2.22675753605982,-6.21782367083837,
79.711181465413));
#54700=CARTESIAN_POINT('Ctrl Pts',(4.02716757885868,-5.23466346748542,79.98960531906));
#54701=CARTESIAN_POINT('Ctrl Pts',(6.58090073238833,0.558145031768453,80.2680291727073));
#54702=CARTESIAN_POINT('Ctrl Pts',(3.08805263200795,5.83812566394266,80.5464530263542));
#54703=CARTESIAN_POINT('Ctrl Pts',(-3.24212152981735,5.75399238024632,80.8248768800015));
#54704=CARTESIAN_POINT('Ctrl Pts',(-6.59340996425109,0.383047476628627,
81.1033007336486));
#54705=CARTESIAN_POINT('Ctrl Pts',(-3.88662356814169,-5.3398443390798,81.3817245872957));
#54706=CARTESIAN_POINT('Ctrl Pts',(2.39122189173239,-6.15644688034727,81.6601484409429));
#54707=CARTESIAN_POINT('Ctrl Pts',(6.47199463277192,-1.31645956998633,81.93857229459));
#54708=CARTESIAN_POINT('Ctrl Pts',(4.6062498660594,4.73310072758491,82.2169961482372));
#54709=CARTESIAN_POINT('Ctrl Pts',(-1.49175203741027,6.43385235958365,82.4954200018842));
#54710=CARTESIAN_POINT('Ctrl Pts',(-6.21912091180313,2.22313189226599,82.7738438555314));
#54711=CARTESIAN_POINT('Ctrl Pts',(-5.23231456151334,-4.03021893393057,
83.0522677091786));
#54712=CARTESIAN_POINT('Ctrl Pts',(0.561981892144835,-6.58057419067199,
83.3306915628256));
#54713=CARTESIAN_POINT('Ctrl Pts',(5.83992514245569,-3.08464822249653,83.6091154164727));
#54714=CARTESIAN_POINT('Ctrl Pts',(5.75210110245894,3.24547580997431,83.8875392701199));
#54715=CARTESIAN_POINT('Ctrl Pts',(0.379203162843909,6.59363217713319,84.165963123767));
#54716=CARTESIAN_POINT('Ctrl Pts',(-5.3421095043464,3.883509542876,84.4443869774141));
#54717=CARTESIAN_POINT('Ctrl Pts',(-6.15505164615532,-2.39481096523249,
84.7228108310613));
#54718=CARTESIAN_POINT('Ctrl Pts',(-1.31268588804032,-6.47276108669066,
85.0012346847084));
#54719=CARTESIAN_POINT('Ctrl Pts',(4.73578556983606,-4.60348947675244,85.2796585383555));
#54720=CARTESIAN_POINT('Ctrl Pts',(6.43298150881899,1.49550300341722,85.5580823920027));
#54721=CARTESIAN_POINT('Ctrl Pts',(2.21950549273989,6.22041603863717,85.8365062456497));
#54722=CARTESIAN_POINT('Ctrl Pts',(-4.03326891896803,5.22996387686611,86.114930099297));
#54723=CARTESIAN_POINT('Ctrl Pts',(-6.58024541195241,-0.565818561480864,
86.393353952944));
#54724=CARTESIAN_POINT('Ctrl Pts',(-3.08124276438845,-5.84172263574204,
86.6717778065911));
#54725=CARTESIAN_POINT('Ctrl Pts',(3.24882898686282,-5.75020786929984,86.9502016602383));
#54726=CARTESIAN_POINT('Ctrl Pts',(6.59385214857313,-0.375358720152691,
87.2286255138854));
#54727=CARTESIAN_POINT('Ctrl Pts',(3.88039419744838,5.34437285361397,87.5070493675325));
#54728=CARTESIAN_POINT('Ctrl Pts',(-2.39839922463963,6.15365431961246,87.7854732211798));
#54729=CARTESIAN_POINT('Ctrl Pts',(-6.47352534025624,1.30891175985915,88.0638970748268));
#54730=CARTESIAN_POINT('Ctrl Pts',(-4.60072752253314,-4.73846880220224,
88.342320928474));
#54731=CARTESIAN_POINT('Ctrl Pts',(1.49925346104233,-6.43210847122385,88.6207447821212));
#54732=CARTESIAN_POINT('Ctrl Pts',(6.22170905090035,-2.21587833871397,88.8991686357682));
#54733=CARTESIAN_POINT('Ctrl Pts',(5.22761141434257,4.03631753293422,89.1775924894154));
#54734=CARTESIAN_POINT('Ctrl Pts',(-0.569655038472113,6.57991439634137,
89.4560163430625));
#54735=CARTESIAN_POINT('Ctrl Pts',(-5.84351814319067,3.07783625884149,89.7344401967096));
#54736=CARTESIAN_POINT('Ctrl Pts',(-5.74831268141256,-3.25218105934286,
90.0128640503567));
#54737=CARTESIAN_POINT('Ctrl Pts',(-0.371514149862039,-6.59406987849609,
90.2912879040039));
#54738=CARTESIAN_POINT('Ctrl Pts',(5.34663438611311,-3.87727753291801,90.5697117576509));
#54739=CARTESIAN_POINT('Ctrl Pts',(6.15225490119367,2.40198666873391,90.8481356112982));
#54740=CARTESIAN_POINT('Ctrl Pts',(1.30513718672595,6.47428739320878,91.1265594649451));
#54741=CARTESIAN_POINT('Ctrl Pts',(-4.74115042377128,4.59796400434054,91.4049833185925));
#54742=CARTESIAN_POINT('Ctrl Pts',(-6.43123324709496,-1.50300340901059,
91.6834071722394));
#54743=CARTESIAN_POINT('Ctrl Pts',(-2.21225043142142,-6.22299994815304,
91.9618310258866));
#54744=CARTESIAN_POINT('Ctrl Pts',(4.03936477479301,-5.22525717474255,92.2402548795338));
#54745=CARTESIAN_POINT('Ctrl Pts',(6.57958114395136,0.573491321814751,92.5186787331809));
#54746=CARTESIAN_POINT('Ctrl Pts',(3.07442870701341,5.8453116641912,92.797102586828));
#54747=CARTESIAN_POINT('Ctrl Pts',(-3.2555320262752,5.74641553944141,93.0755264404753));
#54748=CARTESIAN_POINT('Ctrl Pts',(-6.59428536682807,0.367669453278525,
93.3539502941222));
#54749=CARTESIAN_POINT('Ctrl Pts',(-3.87415955034417,-5.34889410107492,
93.6323741477694));
#54750=CARTESIAN_POINT('Ctrl Pts',(2.40557329629567,-6.15085339137476,93.9107980014166));
#54751=CARTESIAN_POINT('Ctrl Pts',(6.4750472452893,-1.30136216992396,94.1892218550636));
#54752=CARTESIAN_POINT('Ctrl Pts',(4.5951989231141,4.74383043363146,94.4676457087109));
#54753=CARTESIAN_POINT('Ctrl Pts',(-1.50675284604706,6.43035583672989,94.7460695623579));
#54754=CARTESIAN_POINT('Ctrl Pts',(-6.22428872995647,2.20862177209563,95.0244934160051));
#54755=CARTESIAN_POINT('Ctrl Pts',(-5.22290115886631,-4.04241064350841,
95.3029172696522));
#54756=CARTESIAN_POINT('Ctrl Pts',(0.577327410204486,-6.57924565489567,
95.5813411232994));
#54757=CARTESIAN_POINT('Ctrl Pts',(5.84710319813395,-3.07102011006271,95.8597649769464));
#54758=CARTESIAN_POINT('Ctrl Pts',(5.74451644403124,3.25888188652056,96.1381888305936));
#54759=CARTESIAN_POINT('Ctrl Pts',(0.363824631709314,6.59449861349584,96.4166126842407));
#54760=CARTESIAN_POINT('Ctrl Pts',(-5.35115199773147,3.87104025078679,96.6950365378879));
#54761=CARTESIAN_POINT('Ctrl Pts',(-6.14944979063202,-2.40915910610592,
96.973460391535));
#54762=CARTESIAN_POINT('Ctrl Pts',(-1.29758671073624,-6.47580489623943,
97.2518842451821));
#54763=CARTESIAN_POINT('Ctrl Pts',(4.74650883087199,-4.59243227979371,97.5303080988292));
#54764=CARTESIAN_POINT('Ctrl Pts',(6.42947624042683,1.51050177087747,97.8087319524763));
#54765=CARTESIAN_POINT('Ctrl Pts',(2.20499236196995,6.22557539587235,98.0871558061237));
#54766=CARTESIAN_POINT('Ctrl Pts',(-4.04545513804484,5.2205433675149,98.3655796597704));
#54767=CARTESIAN_POINT('Ctrl Pts',(-6.57890792928845,-0.581163302337195,
98.6440035134179));
#54768=CARTESIAN_POINT('Ctrl Pts',(-3.06761046914817,-5.8488927444098,98.9224273670648));
#54769=CARTESIAN_POINT('Ctrl Pts',(3.26223063894007,-5.74261539582774,99.2008512207121));
#54770=CARTESIAN_POINT('Ctrl Pts',(6.59470961842695,-0.359979686461526,
99.4792750743591));
#54771=CARTESIAN_POINT('Ctrl Pts',(3.8679196353063,5.35340807531511,99.7576989280063));
#54772=CARTESIAN_POINT('Ctrl Pts',(-2.41274409694558,6.14804409944263,100.036122781653));
#54773=CARTESIAN_POINT('Ctrl Pts',(-6.47656034580163,1.29381081044633,100.314546635301));
#54774=CARTESIAN_POINT('Ctrl Pts',(-4.58966407531989,-4.74918561458226,
100.592970488948));
#54775=CARTESIAN_POINT('Ctrl Pts',(1.51425018222724,-6.42859445848481,100.871394342595));
#54776=CARTESIAN_POINT('Ctrl Pts',(6.22685994546354,-2.20136220227813,101.149818196242));
#54777=CARTESIAN_POINT('Ctrl Pts',(5.2181838014896,4.04849825736762,101.428242049889));
#54778=CARTESIAN_POINT('Ctrl Pts',(-0.584998996909095,6.57856796724433,
101.706665903536));
#54779=CARTESIAN_POINT('Ctrl Pts',(-5.85068030241062,3.06419978542872,101.985089757183));
#54780=CARTESIAN_POINT('Ctrl Pts',(-5.74071239547699,-3.26557828239561,
102.26351361083));
#54781=CARTESIAN_POINT('Ctrl Pts',(-0.356134618842078,-6.59491838154948,
102.541937464478));
#54782=CARTESIAN_POINT('Ctrl Pts',(5.35566233305879,-3.86479770496367,102.820361318125));
#54783=CARTESIAN_POINT('Ctrl Pts',(6.14663631828457,2.4163282675959,103.098785171772));
#54784=CARTESIAN_POINT('Ctrl Pts',(1.29003447033791,6.47731359371901,103.377209025419));
#54785=CARTESIAN_POINT('Ctrl Pts',(-4.7518607838522,4.58689431063379,103.655632879066));
#54786=CARTESIAN_POINT('Ctrl Pts',(-6.42771049120372,-1.51799807882206,
103.934056732713));
#54787=CARTESIAN_POINT('Ctrl Pts',(-2.19773129425428,-6.22814237829327,
104.21248058636));
#54788=CARTESIAN_POINT('Ctrl Pts',(4.05154000044214,-5.21582246159265,104.490904440007));
#54789=CARTESIAN_POINT('Ctrl Pts',(6.57822576887897,0.588834492616189,104.769328293655));
#54790=CARTESIAN_POINT('Ctrl Pts',(3.06078806006388,5.85246587152864,105.047752147302));
#54791=CARTESIAN_POINT('Ctrl Pts',(-3.26892481574906,5.73880744362598,105.326176000949));
#54792=CARTESIAN_POINT('Ctrl Pts',(-6.59512490279267,0.352289430157958,
105.604599854596));
#54793=CARTESIAN_POINT('Ctrl Pts',(-3.86167446081989,-5.35791477019638,
105.883023708243));
#54794=CARTESIAN_POINT('Ctrl Pts',(2.4199116168386,-6.1452264476362,106.16144756189));
#54795=CARTESIAN_POINT('Ctrl Pts',(6.47806463973569,-1.28625769169451,106.439871415537));
#54796=CARTESIAN_POINT('Ctrl Pts',(4.58412298667673,4.75453433777263,106.718295269185));
#54797=CARTESIAN_POINT('Ctrl Pts',(-1.52174545938792,6.42682433888381,106.996719122832));
#54798=CARTESIAN_POINT('Ctrl Pts',(-6.22942269392552,2.19409963913285,107.275142976479));
#54799=CARTESIAN_POINT('Ctrl Pts',(-5.21345934862686,-4.05458036623436,
107.553566830126));
#54800=CARTESIAN_POINT('Ctrl Pts',(0.59266978815451,-6.57788133430863,107.831990683773));
#54801=CARTESIAN_POINT('Ctrl Pts',(5.8542494511568,-3.05737529421354,108.11041453742));
#54802=CARTESIAN_POINT('Ctrl Pts',(5.7369005409224,3.27227023786272,108.388838391067));
#54803=CARTESIAN_POINT('Ctrl Pts',(0.348444121716408,6.59532918208624,108.667262244714));
#54804=CARTESIAN_POINT('Ctrl Pts',(-5.36016538596209,3.85854990393683,108.945686098361));
#54805=CARTESIAN_POINT('Ctrl Pts',(-6.14381448797689,-2.42349414345551,
109.224109952009));
#54806=CARTESIAN_POINT('Ctrl Pts',(-1.28248047580012,-6.47881348359625,
109.502533805656));
#54807=CARTESIAN_POINT('Ctrl Pts',(4.7572062754346,-4.58135010439092,109.780957659303));
#54808=CARTESIAN_POINT('Ctrl Pts',(6.42593600182647,1.52549232265109,110.05938151295));
#54809=CARTESIAN_POINT('Ctrl Pts',(2.19046723814809,6.23070089192516,110.337805366597));
#54810=CARTESIAN_POINT('Ctrl Pts',(-4.05761935371081,5.21109446339532,110.616229220244));
#54811=CARTESIAN_POINT('Ctrl Pts',(-6.57753466365052,-0.596504882220527,
110.894653073892));
#54812=CARTESIAN_POINT('Ctrl Pts',(-3.05396148903758,-5.85603104068893,
111.173076927538));
#54813=CARTESIAN_POINT('Ctrl Pts',(3.27561454759935,-5.73499168801425,111.451500781186));
#54814=CARTESIAN_POINT('Ctrl Pts',(6.59553121936074,-0.344598694824773,
111.729924634833));
#54815=CARTESIAN_POINT('Ctrl Pts',(3.85542403537677,5.36241417959085,112.00834848848));
#54816=CARTESIAN_POINT('Ctrl Pts',(-2.42707584622865,6.14240043978659,112.286772342127));
#54817=CARTESIAN_POINT('Ctrl Pts',(-6.47956012504612,1.2787028239389,112.565196195774));
#54818=CARTESIAN_POINT('Ctrl Pts',(-4.57857566471911,-4.75987659592976,
112.843620049421));
#54819=CARTESIAN_POINT('Ctrl Pts',(1.52923866733776,-6.42504548033368,113.122043903069));
#54820=CARTESIAN_POINT('Ctrl Pts',(6.23197697185764,-2.18683409253494,113.400467756716));
#54821=CARTESIAN_POINT('Ctrl Pts',(5.20872780670208,4.06065696183837,113.678891610363));
#54822=CARTESIAN_POINT('Ctrl Pts',(-0.600339773510414,6.57718575702242,
113.95731546401));
#54823=CARTESIAN_POINT('Ctrl Pts',(-5.85781063951934,3.05054664569663,114.235739317657));
#54824=CARTESIAN_POINT('Ctrl Pts',(-5.73308088555054,-3.27895774382228,
114.514163171304));
#54825=CARTESIAN_POINT('Ctrl Pts',(-0.340753150789953,-6.5957310145475,
114.792587024951));
#54826=CARTESIAN_POINT('Ctrl Pts',(5.36466115031821,-3.85229685620206,115.071010878598));
#54827=CARTESIAN_POINT('Ctrl Pts',(6.14098430354606,2.43065672394069,115.349434732246));
#54828=CARTESIAN_POINT('Ctrl Pts',(1.27492473739474,6.48030456383154,115.627858585892));
#54829=CARTESIAN_POINT('Ctrl Pts',(-4.76254529835031,4.5757996686042,115.90628243954));
#54830=CARTESIAN_POINT('Ctrl Pts',(-6.42415277470816,-1.53298449217421,
116.184706293187));
#54831=CARTESIAN_POINT('Ctrl Pts',(-2.18320020352859,-6.2332509332892,116.463130146834));
#54832=CARTESIAN_POINT('Ctrl Pts',(4.06369318958433,-5.20635937935165,116.741554000481));
#54833=CARTESIAN_POINT('Ctrl Pts',(6.57683461454295,0.604174460720374,117.019977854128));
#54834=CARTESIAN_POINT('Ctrl Pts',(3.04713076535168,5.85958824704307,117.298401707775));
#54835=CARTESIAN_POINT('Ctrl Pts',(-3.28229982539491,5.73116813418082,117.576825561423));
#54836=CARTESIAN_POINT('Ctrl Pts',(-6.59592856757859,0.336907490919371,
117.85524941507));
#54837=CARTESIAN_POINT('Ctrl Pts',(-3.84916836747591,-5.36690629738036,
118.133673268717));
#54838=CARTESIAN_POINT('Ctrl Pts',(2.43423677537425,-6.13956607973662,118.412097122364));
#54839=CARTESIAN_POINT('Ctrl Pts',(6.48104679969937,-1.27114621745216,118.690520976011));
#54840=CARTESIAN_POINT('Ctrl Pts',(4.57302211699003,4.76521238178937,118.968944829658));
#54841=CARTESIAN_POINT('Ctrl Pts',(-1.53672979588759,6.42325788525319,119.247368683305));
#54842=CARTESIAN_POINT('Ctrl Pts',(-6.23452277578633,2.17956557236435,119.525792536953));
#54843=CARTESIAN_POINT('Ctrl Pts',(-5.20398918214985,-4.06672803591727,
119.8042163906));
#54844=CARTESIAN_POINT('Ctrl Pts',(0.608008942548482,-6.57648123633055,
120.082640244247));
#54845=CARTESIAN_POINT('Ctrl Pts',(5.86136386265324,-3.04371384916539,120.361064097894));
#54846=CARTESIAN_POINT('Ctrl Pts',(5.72925343456004,3.28564079118416,120.639487951541));
#54847=CARTESIAN_POINT('Ctrl Pts',(0.333061716511642,6.59612387838091,120.917911805188));
#54848=CARTESIAN_POINT('Ctrl Pts',(-5.36914961999736,3.84603857027319,121.196335658835));
#54849=CARTESIAN_POINT('Ctrl Pts',(-6.13814576887177,-2.43781599933361,
121.474759512482));
#54850=CARTESIAN_POINT('Ctrl Pts',(-1.26736726533664,-6.4817868323569,121.753183366129));
#54851=CARTESIAN_POINT('Ctrl Pts',(4.76787784522852,-4.57024301089718,122.031607219777));
#54852=CARTESIAN_POINT('Ctrl Pts',(6.42236081248373,1.5404745773487,122.310031073424));
#54853=CARTESIAN_POINT('Ctrl Pts',(2.17593019988002,6.23579249864457,122.588454927071));
#54854=CARTESIAN_POINT('Ctrl Pts',(-4.06976149905412,5.20161721641628,122.866878780718));
#54855=CARTESIAN_POINT('Ctrl Pts',(-6.57612562392392,-0.611843218661398,
123.145302634365));
#54856=CARTESIAN_POINT('Ctrl Pts',(-3.04029589562085,-5.86313748391429,
123.423726488012));
#54857=CARTESIAN_POINT('Ctrl Pts',(3.28898063499709,-5.72733679079851,123.702150341659));
#54858=CARTESIAN_POINT('Ctrl Pts',(6.5963169564375,-0.329215822341513,123.980574195307));
#54859=CARTESIAN_POINT('Ctrl Pts',(3.84290744762627,5.37139110507242,124.258998048954));
#54860=CARTESIAN_POINT('Ctrl Pts',(-2.4413943605552,6.13672339472416,124.537421902601));
#54861=CARTESIAN_POINT('Ctrl Pts',(-6.48252472584031,1.26358783835648,124.815845756248));
#54862=CARTESIAN_POINT('Ctrl Pts',(-4.56746222988183,-4.77054160472563,
125.094269609895));
#54863=CARTESIAN_POINT('Ctrl Pts',(1.54421860607799,-6.42146171349359,125.372693463542));
#54864=CARTESIAN_POINT('Ctrl Pts',(6.23706053422062,-2.17229379126241,125.651117317189));
#54865=CARTESIAN_POINT('Ctrl Pts',(5.19924266576478,4.07279301896267,125.929541170837));
#54866=CARTESIAN_POINT('Ctrl Pts',(-0.615675744729761,6.57576883295141,
126.207965024483));
#54867=CARTESIAN_POINT('Ctrl Pts',(-5.86491202376979,3.03687491286735,126.486388878131));
#54868=CARTESIAN_POINT('Ctrl Pts',(-5.72541270217929,-3.29231559248493,
126.764812731778));
#54869=CARTESIAN_POINT('Ctrl Pts',(-0.325380197419233,-6.59651490739494,
127.043236585425));
#54870=CARTESIAN_POINT('Ctrl Pts',(5.37365036593983,-3.83976158356861,127.321660439072));
#54871=CARTESIAN_POINT('Ctrl Pts',(6.1352619223662,2.44494652372861,127.600084292719));
#54872=CARTESIAN_POINT('Ctrl Pts',(1.25987786825185,6.48330831590777,127.878508146366));
#54873=CARTESIAN_POINT('Ctrl Pts',(-4.77333570284661,4.56458945006103,128.156932000013));
#54874=CARTESIAN_POINT('Ctrl Pts',(-6.42031125916862,-1.54779132331292,
128.435355853661));
#54875=CARTESIAN_POINT('Ctrl Pts',(-2.16912716912506,-6.23864897710079,
128.713779707308));
#54876=CARTESIAN_POINT('Ctrl Pts',(4.07671190140194,-5.19625695937802,128.992203560955));
#54877=CARTESIAN_POINT('Ctrl Pts',(6.57372921642299,0.618354217852361,129.270627414602));
#54878=CARTESIAN_POINT('Ctrl Pts',(3.03664626371355,5.86888938326796,129.549051268249));
#54879=CARTESIAN_POINT('Ctrl Pts',(-3.30184300701674,5.71910967681579,129.827475121896));
#54880=CARTESIAN_POINT('Ctrl Pts',(-6.03672382843121,1.22950628103885,130.059494999936));
#54881=CARTESIAN_POINT('Ctrl Pts',(-5.22664060241318,-2.54029413961005,
130.245110902367));
#54882=CARTESIAN_POINT('Ctrl Pts',(-4.00101382151821,-4.00468766736226,
130.337918853583));
#54883=CARTESIAN_POINT('Ctrl Pts',(-3.24375760296964,-4.54512507566672,
130.384322829191));
#54884=CARTESIAN_POINT('Ctrl Pts',(-4.20009954634508,-4.16738459507781,
-9.47071414072041));
#54885=CARTESIAN_POINT('Ctrl Pts',(-3.50577808166169,-4.8671566469011,-9.42431016511256));
#54886=CARTESIAN_POINT('Ctrl Pts',(-1.76531786303429,-5.89918424712944,
-9.33150221389684));
#54887=CARTESIAN_POINT('Ctrl Pts',(2.31525814347615,-6.10349577227439,-9.14588631146544));
#54888=CARTESIAN_POINT('Ctrl Pts',(6.54407278403002,-2.4777592280193,-8.91386643342614));
#54889=CARTESIAN_POINT('Ctrl Pts',(5.61980217846484,4.17653187559757,-8.63544257977903));
#54890=CARTESIAN_POINT('Ctrl Pts',(-0.47435427916949,6.98020994205008,-8.35701872613188));
#54891=CARTESIAN_POINT('Ctrl Pts',(-6.12941616757563,3.37727447383079,-8.07859487248477));
#54892=CARTESIAN_POINT('Ctrl Pts',(-6.15443318799092,-3.33234179095485,
-7.80017101883763));
#54893=CARTESIAN_POINT('Ctrl Pts',(-0.523807255543973,-6.97826436643947,
-7.5217471651905));
#54894=CARTESIAN_POINT('Ctrl Pts',(5.58761856355849,-4.21351783333861,-7.24332331154338));
#54895=CARTESIAN_POINT('Ctrl Pts',(6.56535149650638,2.42317706277268,-6.96489945789624));
#54896=CARTESIAN_POINT('Ctrl Pts',(1.51065583012593,6.8331545214114,-6.68647560424912));
#54897=CARTESIAN_POINT('Ctrl Pts',(-4.9319707928733,4.96492848346115,-6.40805175060197));
#54898=CARTESIAN_POINT('Ctrl Pts',(-6.84310304594355,-1.46519098634236,
-6.12962789695486));
#54899=CARTESIAN_POINT('Ctrl Pts',(-2.46672066112633,-6.5490397251654,-5.85120404330772));
#54900=CARTESIAN_POINT('Ctrl Pts',(4.17609273205395,-5.61560369114569,-5.5727801896606));
#54901=CARTESIAN_POINT('Ctrl Pts',(6.98188619633454,0.477503226102664,-5.29435633601347));
#54902=CARTESIAN_POINT('Ctrl Pts',(3.37266697756901,6.13187030790779,-5.01593248236633));
#54903=CARTESIAN_POINT('Ctrl Pts',(-3.33538254404525,6.15223199783412,-4.73750862871921));
#54904=CARTESIAN_POINT('Ctrl Pts',(-6.97885824454911,0.519874743954567,
-4.45908477507207));
#54905=CARTESIAN_POINT('Ctrl Pts',(-4.21010588636016,-5.59014641670148,
-4.18066092142495));
#54906=CARTESIAN_POINT('Ctrl Pts',(2.42692329786755,-6.56389935825552,-3.90223706777781));
#54907=CARTESIAN_POINT('Ctrl Pts',(6.83407716517237,-1.50669177560396,-3.62381321413069));
#54908=CARTESIAN_POINT('Ctrl Pts',(4.9620292963081,4.93487544201203,-3.34538936048356));
#54909=CARTESIAN_POINT('Ctrl Pts',(-1.46916850004176,6.84224193704743,-3.06696550683643));
#54910=CARTESIAN_POINT('Ctrl Pts',(-6.55048321018197,2.46290486839966,-2.7885416531893));
#54911=CARTESIAN_POINT('Ctrl Pts',(-5.61316450565459,-4.17936775843667,
-2.51011779954216));
#54912=CARTESIAN_POINT('Ctrl Pts',(0.48157209976335,-6.98160576123052,-2.23169394589504));
#54913=CARTESIAN_POINT('Ctrl Pts',(6.13383662858499,-3.36909170003948,-1.95327009224791));
#54914=CARTESIAN_POINT('Ctrl Pts',(6.15028577427905,3.33896923603762,-1.67484623860078));
#54915=CARTESIAN_POINT('Ctrl Pts',(0.515805939856379,6.97916004302912,-1.39642238495365));
#54916=CARTESIAN_POINT('Ctrl Pts',(-5.59260028490076,4.20684593528139,-1.11799853130652));
#54917=CARTESIAN_POINT('Ctrl Pts',(-6.56248316462805,-2.43074996317731,
-0.839574677659391));
#54918=CARTESIAN_POINT('Ctrl Pts',(-1.50270699079991,-6.83495445271005,
-0.56115082401226));
#54919=CARTESIAN_POINT('Ctrl Pts',(4.93776770600804,-4.95915121282611,-0.282726970365132));
#54920=CARTESIAN_POINT('Ctrl Pts',(6.84138417297234,1.47315758423168,-0.004303116718001));
#54921=CARTESIAN_POINT('Ctrl Pts',(2.4590852351668,6.55191807614683,0.274120736929126));
#54922=CARTESIAN_POINT('Ctrl Pts',(-4.18263977354214,5.61072679739748,0.55254459057626));
#54923=CARTESIAN_POINT('Ctrl Pts',(-6.98132379515334,-0.485642602626536,
0.830968444223388));
#54924=CARTESIAN_POINT('Ctrl Pts',(-3.36551483110386,-6.13579991459174,
1.10939229787052));
#54925=CARTESIAN_POINT('Ctrl Pts',(3.34255455671475,-6.14833796286877,1.38781615151765));
#54926=CARTESIAN_POINT('Ctrl Pts',(6.97945959413709,-0.511736694089966,
1.66624000516478));
#54927=CARTESIAN_POINT('Ctrl Pts',(4.20358448785803,5.59505211090234,1.94466385881191));
#54928=CARTESIAN_POINT('Ctrl Pts',(-2.43457576708131,6.5610648148461,2.22308771245903));
#54929=CARTESIAN_POINT('Ctrl Pts',(-6.8358294353571,1.49872165560417,2.50151156610617));
#54930=CARTESIAN_POINT('Ctrl Pts',(-4.95627143368447,-4.94065827050558,
2.77993541975329));
#54931=CARTESIAN_POINT('Ctrl Pts',(1.47714616242253,-6.84052409433019,3.05835927340044));
#54932=CARTESIAN_POINT('Ctrl Pts',(6.55335071761077,-2.45526476011491,3.33678312704754));
#54933=CARTESIAN_POINT('Ctrl Pts',(5.60828718036528,4.18591036368699,3.61520698069469));
#54934=CARTESIAN_POINT('Ctrl Pts',(-0.489712939625793,6.98103945749017,
3.89363083434181));
#54935=CARTESIAN_POINT('Ctrl Pts',(-6.13776111520212,3.36193681722077,4.17205468798895));
#54936=CARTESIAN_POINT('Ctrl Pts',(-6.14638806117258,-3.34613874066016,
4.45047854163607));
#54937=CARTESIAN_POINT('Ctrl Pts',(-0.507667274478622,-6.97975677288937,
4.72890239528321));
#54938=CARTESIAN_POINT('Ctrl Pts',(5.59750203498042,-4.20032161133665,5.00732624893033));
#54939=CARTESIAN_POINT('Ctrl Pts',(6.55964423466067,2.43840074330588,5.28575010257747));
#54940=CARTESIAN_POINT('Ctrl Pts',(1.49473581094941,6.83670209426571,5.56417395622459));
#54941=CARTESIAN_POINT('Ctrl Pts',(-4.94354715548264,4.95338996968654,5.84259780987173));
#54942=CARTESIAN_POINT('Ctrl Pts',(-6.83966169031252,-1.4811342384615,6.12102166351884));
#54943=CARTESIAN_POINT('Ctrl Pts',(-2.45144345042182,-6.55478113133121,
6.399445517166));
#54944=CARTESIAN_POINT('Ctrl Pts',(4.18917953087302,-5.60584565684663,6.67786937081309));
#54945=CARTESIAN_POINT('Ctrl Pts',(6.98075274668871,0.493783110150294,6.95629322446026));
#54946=CARTESIAN_POINT('Ctrl Pts',(3.35835766047978,6.13972022934013,7.23471707810736));
#54947=CARTESIAN_POINT('Ctrl Pts',(-3.34972178711789,6.14443607007018,7.5131409317545));
#54948=CARTESIAN_POINT('Ctrl Pts',(-6.98005157894001,0.503597682290836,
7.79156478540162));
#54949=CARTESIAN_POINT('Ctrl Pts',(-4.1970573069562,-5.59995005624133,8.06998863904877));
#54950=CARTESIAN_POINT('Ctrl Pts',(2.44222489061947,-6.55822142458687,8.34841249269588));
#54951=CARTESIAN_POINT('Ctrl Pts',(6.83757242910279,-1.49074945817361,8.62683634634303));
#54952=CARTESIAN_POINT('Ctrl Pts',(4.9505068218311,4.94643435994816,8.90526019999013));
#54953=CARTESIAN_POINT('Ctrl Pts',(-1.48512181100304,6.83879696121727,9.18368405363728));
#54954=CARTESIAN_POINT('Ctrl Pts',(-6.55620931681649,2.44762130738398,9.46210790728441));
#54955=CARTESIAN_POINT('Ctrl Pts',(-5.60340222767442,-4.19244727398749,
9.74053176093154));
#54956=CARTESIAN_POINT('Ctrl Pts',(0.497853112817942,-6.98046366284714,
10.0189556145787));
#54957=CARTESIAN_POINT('Ctrl Pts',(6.14167725633898,-3.35477736209725,10.2973794682258));
#54958=CARTESIAN_POINT('Ctrl Pts',(6.14248199022549,3.35330369486973,10.5758033218729));
#54959=CARTESIAN_POINT('Ctrl Pts',(0.499527918909906,6.98034401218888,10.8542271755201));
#54960=CARTESIAN_POINT('Ctrl Pts',(-5.6023961738528,4.19379157582627,11.1326510291672));
#54961=CARTESIAN_POINT('Ctrl Pts',(-6.55679638510844,-2.4460482077221,11.4110748828143));
#54962=CARTESIAN_POINT('Ctrl Pts',(-1.48676259863171,-6.83844043957255,
11.6894987364615));
#54963=CARTESIAN_POINT('Ctrl Pts',(4.94931988292061,-4.94762199109819,11.9679225901086));
#54964=CARTESIAN_POINT('Ctrl Pts',(6.83792990733845,1.48910887869161,12.2463464437557));
#54965=CARTESIAN_POINT('Ctrl Pts',(2.44379833230066,6.55763527358118,12.5247702974028));
#54966=CARTESIAN_POINT('Ctrl Pts',(-4.19571359191966,5.60095689367916,12.80319415105));
#54967=CARTESIAN_POINT('Ctrl Pts',(-6.98017220606371,-0.501922946245178,
13.0816180046971));
#54968=CARTESIAN_POINT('Ctrl Pts',(-3.35119592329026,-6.1436321955334,13.3600418583442));
#54969=CARTESIAN_POINT('Ctrl Pts',(3.3568844626981,-6.14052582230283,13.6384657119914));
#54970=CARTESIAN_POINT('Ctrl Pts',(6.98063407253657,-0.495457985719165,
13.9168895656385));
#54971=CARTESIAN_POINT('Ctrl Pts',(4.190524419057,5.60484038698326,14.1953134192856));
#54972=CARTESIAN_POINT('Ctrl Pts',(-2.44987069331402,6.55536911670982,14.4737372729327));
#54973=CARTESIAN_POINT('Ctrl Pts',(-6.83930612537993,1.4827752336791,14.7521611265799));
#54974=CARTESIAN_POINT('Ctrl Pts',(-4.94473547846849,-4.95220372341915,
15.030584980227));
#54975=CARTESIAN_POINT('Ctrl Pts',(1.49309544017187,-6.83706052897074,15.3090088338741));
#54976=CARTESIAN_POINT('Ctrl Pts',(6.55905900114047,-2.43997452647152,15.5874326875213));
#54977=CARTESIAN_POINT('Ctrl Pts',(5.59850965569222,4.19897848355916,15.8658565411684));
#54978=CARTESIAN_POINT('Ctrl Pts',(-0.505992609048554,6.97987837643749,
16.1442803948155));
#54979=CARTESIAN_POINT('Ctrl Pts',(-6.1455850462588,3.34761334527627,16.4227042484627));
#54980=CARTESIAN_POINT('Ctrl Pts',(-6.13856756696716,-3.36046408938568,
16.7011281021098));
#54981=CARTESIAN_POINT('Ctrl Pts',(-0.491387884102221,-6.98092175988452,
16.9795519557569));
#54982=CARTESIAN_POINT('Ctrl Pts',(5.60728269480187,-4.18725583775901,17.257975809404));
#54983=CARTESIAN_POINT('Ctrl Pts',(6.55393961987617,2.45369234609581,17.5363996630512));
#54984=CARTESIAN_POINT('Ctrl Pts',(1.47878736467127,6.84016948623062,17.8148235166983));
#54985=CARTESIAN_POINT('Ctrl Pts',(-4.95508588046342,4.94184728492329,18.0932473703454));
#54986=CARTESIAN_POINT('Ctrl Pts',(-6.8361888264097,-1.49708149408864,18.3716712239925));
#54987=CARTESIAN_POINT('Ctrl Pts',(-2.43614989119636,-6.56048049901039,
18.6500950776397));
#54988=CARTESIAN_POINT('Ctrl Pts',(4.20224194779605,-5.59606051454548,18.9285189312868));
#54989=CARTESIAN_POINT('Ctrl Pts',(6.97958217406843,0.510062099844575,19.2069427849339));
#54990=CARTESIAN_POINT('Ctrl Pts',(3.34402962927311,6.14753580785139,19.4853666385811));
#54991=CARTESIAN_POINT('Ctrl Pts',(-3.36404257371562,6.13660722488416,19.7637904922282));
#54992=CARTESIAN_POINT('Ctrl Pts',(-6.9812070741349,0.487317615442708,20.0422143458754));
#54993=CARTESIAN_POINT('Ctrl Pts',(-4.18398583304347,-5.60972309647839,
20.3206381995225));
#54994=CARTESIAN_POINT('Ctrl Pts',(2.45751316476841,-6.55250789509341,20.5990620531696));
#54995=CARTESIAN_POINT('Ctrl Pts',(6.84103052183109,-1.47479899296382,20.8774859068167));
#54996=CARTESIAN_POINT('Ctrl Pts',(4.9389574114444,4.95796635307363,21.1559097604638));
#54997=CARTESIAN_POINT('Ctrl Pts',(-1.50106703908689,6.83531479995168,21.434333614111));
#54998=CARTESIAN_POINT('Ctrl Pts',(-6.56189976670772,2.43232442777533,21.7127574677581));
#54999=CARTESIAN_POINT('Ctrl Pts',(-5.5936094710715,-4.20550398352098,21.9911813214053));
#55000=CARTESIAN_POINT('Ctrl Pts',(0.514131417249838,-6.97928359905718,
22.2696051750524));
#55001=CARTESIAN_POINT('Ctrl Pts',(6.149484479648,-3.34044477649908,22.5480290286995));
#55002=CARTESIAN_POINT('Ctrl Pts',(6.13464479672021,3.36761991447152,22.8264528823466));
#55003=CARTESIAN_POINT('Ctrl Pts',(0.483247181124235,6.98149001519067,23.1048767359938));
#55004=CARTESIAN_POINT('Ctrl Pts',(-5.61216159118322,4.180714406022,23.3833005896409));
#55005=CARTESIAN_POINT('Ctrl Pts',(-6.5510739428483,-2.46133314803299,23.661724443288));
#55006=CARTESIAN_POINT('Ctrl Pts',(-1.47081011991242,-6.84188923188871,
23.9401482969351));
#55007=CARTESIAN_POINT('Ctrl Pts',(4.96084514027061,-4.93606585901412,24.2185721505823));
#55008=CARTESIAN_POINT('Ctrl Pts',(6.8344384498938,1.50505207381178,24.4969960042294));
#55009=CARTESIAN_POINT('Ctrl Pts',(2.42849813750882,6.56331680375008,24.7754198578766));
#55010=CARTESIAN_POINT('Ctrl Pts',(-4.20876458962517,5.5911565261034,25.0538437115237));
#55011=CARTESIAN_POINT('Ctrl Pts',(-6.97898265150518,-0.5182005598811,25.3322675651708));
#55012=CARTESIAN_POINT('Ctrl Pts',(-3.33685878817279,-6.15143106098621,
25.6106914188179));
#55013=CARTESIAN_POINT('Ctrl Pts',(3.37119611043732,-6.13268028314246,25.889115272465));
#55014=CARTESIAN_POINT('Ctrl Pts',(6.98177058295572,-0.479176582530357,
26.1675391261122));
#55015=CARTESIAN_POINT('Ctrl Pts',(4.1774415578066,5.61459817808735,26.4459629797593));
#55016=CARTESIAN_POINT('Ctrl Pts',(-2.4651522945908,6.54963776362828,26.7243868334065));
#55017=CARTESIAN_POINT('Ctrl Pts',(-6.84274561611155,1.46682074687334,27.0028106870536));
#55018=CARTESIAN_POINT('Ctrl Pts',(-4.93317262861548,-4.96372224107578,
27.2812345407007));
#55019=CARTESIAN_POINT('Ctrl Pts',(1.50903659690863,-6.83355977653392,27.5596583943478));
#55020=CARTESIAN_POINT('Ctrl Pts',(6.56473160965562,-2.42467102169763,27.838082247995));
#55021=CARTESIAN_POINT('Ctrl Pts',(5.58870168047518,4.21202376500006,28.1165061016421));
#55022=CARTESIAN_POINT('Ctrl Pts',(-0.52226952635505,6.97867933151483,28.3949299552892));
#55023=CARTESIAN_POINT('Ctrl Pts',(-6.1533755512042,3.33327166551328,28.6733538089363));
#55024=CARTESIAN_POINT('Ctrl Pts',(-6.13071368481874,-3.37477116039712,
28.9517776625835));
#55025=CARTESIAN_POINT('Ctrl Pts',(-0.475105821045126,-6.9820487773347,
29.2302015162306));
#55026=CARTESIAN_POINT('Ctrl Pts',(5.61703285636259,-4.17416728950991,29.5086253698778));
#55027=CARTESIAN_POINT('Ctrl Pts',(6.54819935792153,2.46897060314373,29.7870492235249));
#55028=CARTESIAN_POINT('Ctrl Pts',(1.4628308752025,6.84359967420847,30.065473077172));
#55029=CARTESIAN_POINT('Ctrl Pts',(-4.96659765451106,4.93027772123201,30.3438969308191));
#55030=CARTESIAN_POINT('Ctrl Pts',(-6.83267878017075,-1.51302060702285,
30.6223207844663));
#55031=CARTESIAN_POINT('Ctrl Pts',(-2.42084308164284,-6.56614418394338,
30.9007446381133));
#55032=CARTESIAN_POINT('Ctrl Pts',(4.21528150853767,-5.5862449350214,31.1791684917606));
#55033=CARTESIAN_POINT('Ctrl Pts',(6.97837363918924,0.526338315288408,31.4575923454076));
#55034=CARTESIAN_POINT('Ctrl Pts',(3.32968340973994,6.15531794964111,31.7360161990548));
#55035=CARTESIAN_POINT('Ctrl Pts',(-3.37834506313583,6.12874500241751,32.0144400527019));
#55036=CARTESIAN_POINT('Ctrl Pts',(-6.98232459823295,0.471034898052151,
32.292863906349));
#55037=CARTESIAN_POINT('Ctrl Pts',(-4.17089160224498,-5.61946562518125,
32.5712877599962));
#55038=CARTESIAN_POINT('Ctrl Pts',(2.47278807239367,-6.54675872621704,32.8497116136433));
#55039=CARTESIAN_POINT('Ctrl Pts',(6.84445140588907,-1.45884050625643,33.1281354672904));
#55040=CARTESIAN_POINT('Ctrl Pts',(4.92738113784791,4.96947137959889,33.4065593209376));
#55041=CARTESIAN_POINT('Ctrl Pts',(-1.51700410280022,6.83179546110386,33.6849831745847));
#55042=CARTESIAN_POINT('Ctrl Pts',(-6.56755452613331,2.41701431864547,33.9634070282318));
#55043=CARTESIAN_POINT('Ctrl Pts',(-5.58378629057699,-4.21853781913074,
34.2418308818789));
#55044=CARTESIAN_POINT('Ctrl Pts',(0.530406925298152,-6.97806557463225,
34.5202547355261));
#55045=CARTESIAN_POINT('Ctrl Pts',(6.15725825563656,-3.32609402207256,34.7986785891732));
#55046=CARTESIAN_POINT('Ctrl Pts',(6.12677423660805,3.38191781743839,35.0771024428204));
#55047=CARTESIAN_POINT('Ctrl Pts',(0.466963814935509,6.98259804555671,35.3555262964674));
#55048=CARTESIAN_POINT('Ctrl Pts',(-5.62189648371627,4.16761449712548,35.6339501501146));
#55049=CARTESIAN_POINT('Ctrl Pts',(-6.54531586900461,-2.47660470104297,
35.9123740037618));
#55050=CARTESIAN_POINT('Ctrl Pts',(-1.45484964139136,-6.84530081086397,
36.1907978574088));
#55051=CARTESIAN_POINT('Ctrl Pts',(4.97234341536255,-4.92448287944761,36.4692217110561));
#55052=CARTESIAN_POINT('Ctrl Pts',(6.8309098196334,1.52098708288659,36.7476455647031));
#55053=CARTESIAN_POINT('Ctrl Pts',(2.41318473400722,6.56896263574592,37.0260694183503));
#55054=CARTESIAN_POINT('Ctrl Pts',(-4.22179269567218,5.58132574797784,37.3044932719974));
#55055=CARTESIAN_POINT('Ctrl Pts',(-6.97775513794859,-0.534475355000993,
37.5829171256445));
#55056=CARTESIAN_POINT('Ctrl Pts',(-3.3225035037315,-6.15919646853093,37.8613409792916));
#55057=CARTESIAN_POINT('Ctrl Pts',(3.38548942209037,-6.12480138806036,38.1397648329388));
#55058=CARTESIAN_POINT('Ctrl Pts',(6.98286911921309,-0.462892573078836,
38.4181886865859));
#55059=CARTESIAN_POINT('Ctrl Pts',(4.16433597526518,5.62432543114141,38.696612540233));
#55060=CARTESIAN_POINT('Ctrl Pts',(-2.48042048779425,6.54387078677464,38.9750363938802));
#55061=CARTESIAN_POINT('Ctrl Pts',(-6.84614788884433,1.45085828196406,39.2534602475273));
#55062=CARTESIAN_POINT('Ctrl Pts',(-4.92158294701648,-4.97521376082556,
39.5318841011744));
#55063=CARTESIAN_POINT('Ctrl Pts',(1.52496954592781,-6.83002185606051,39.8103079548215));
#55064=CARTESIAN_POINT('Ctrl Pts',(6.57036851230249,-2.40935432903004,40.0887318084687));
#55065=CARTESIAN_POINT('Ctrl Pts',(5.57886330806047,4.22504613705561,40.3671556621158));
#55066=CARTESIAN_POINT('Ctrl Pts',(-0.538543603014195,6.97744232924386,
40.6455795157629));
#55067=CARTESIAN_POINT('Ctrl Pts',(-6.16113258766541,3.318911855937,40.9240033694101));
#55068=CARTESIAN_POINT('Ctrl Pts',(-6.12282645744497,-3.38905987587764,
41.2024272230572));
#55069=CARTESIAN_POINT('Ctrl Pts',(-0.458821173866272,-6.98313781910993,
41.4808510767043));
#55070=CARTESIAN_POINT('Ctrl Pts',(5.62675246663088,-4.16105603777872,41.7592749303515));
#55071=CARTESIAN_POINT('Ctrl Pts',(6.54242348001838,2.48423543135017,42.0376987839985));
#55072=CARTESIAN_POINT('Ctrl Pts',(1.44686642933153,6.84699263954222,42.3161226376458));
#55073=CARTESIAN_POINT('Ctrl Pts',(-4.9780824150123,4.91868134154035,42.5945464912928));
#55074=CARTESIAN_POINT('Ctrl Pts',(-6.82913157068701,-1.52895149057037,
42.87297034494));
#55075=CARTESIAN_POINT('Ctrl Pts',(-2.40552310501578,-6.57177215532517,
43.151394198587));
#55076=CARTESIAN_POINT('Ctrl Pts',(4.22829814217506,-5.5763989716618,43.4298180522343));
#55077=CARTESIAN_POINT('Ctrl Pts',(6.97712714862434,0.542611667954641,43.7082419058813));
#55078=CARTESIAN_POINT('Ctrl Pts',(3.3153190799102,6.16306661238177,43.9866657595286));
#55079=CARTESIAN_POINT('Ctrl Pts',(-3.39262917758629,6.12084944543334,44.2650896131756));
#55080=CARTESIAN_POINT('Ctrl Pts',(-6.98340414515589,0.454749618681986,
44.5435134668228));
#55081=CARTESIAN_POINT('Ctrl Pts',(-4.15777468578111,-5.62917758935972,
44.8219373204699));
#55082=CARTESIAN_POINT('Ctrl Pts',(2.48804953041416,-6.54097394922784,45.100361174117));
#55083=CARTESIAN_POINT('Ctrl Pts',(6.84783506267045,-1.44287408485045,45.3787850277641));
#55084=CARTESIAN_POINT('Ctrl Pts',(4.9157780640055,4.98094937694757,45.6572088814113));
#55085=CARTESIAN_POINT('Ctrl Pts',(-1.5329329154605,6.82823896381557,45.9356327350584));
#55086=CARTESIAN_POINT('Ctrl Pts',(-6.57317356433671,2.40169106326698,46.2140565887055));
#55087=CARTESIAN_POINT('Ctrl Pts',(-5.57393273961971,-4.23154870992487,
46.4924804423526));
#55088=CARTESIAN_POINT('Ctrl Pts',(0.546679548439304,-6.97680959619725,
46.7709042959998));
#55089=CARTESIAN_POINT('Ctrl Pts',(6.16499854202264,-3.31172517687243,47.0493281496469));
#55090=CARTESIAN_POINT('Ctrl Pts',(6.11887035269745,3.39619732600324,47.327752003294));
#55091=CARTESIAN_POINT('Ctrl Pts',(0.450677908909769,6.98366809726039,47.6061758569412));
#55092=CARTESIAN_POINT('Ctrl Pts',(-5.6316007985035,4.1544919203877,47.8845997105883));
#55093=CARTESIAN_POINT('Ctrl Pts',(-6.53952219489578,-2.49186278368952,
48.1630235642354));
#55094=CARTESIAN_POINT('Ctrl Pts',(-1.43888124987817,-6.84867515794263,
48.4414474178826));
#55095=CARTESIAN_POINT('Ctrl Pts',(4.98381464565661,-4.91287311539898,48.7198712715296));
#55096=CARTESIAN_POINT('Ctrl Pts',(6.82734403574969,1.53691381924461,48.9982951251769));
#55097=CARTESIAN_POINT('Ctrl Pts',(2.3978582050863,6.57457273886085,49.2767189788239));
#55098=CARTESIAN_POINT('Ctrl Pts',(-4.23479783920031,5.57146461277246,49.5551428324711));
#55099=CARTESIAN_POINT('Ctrl Pts',(-6.97648967207044,-0.550747243085628,
49.8335666861182));
#55100=CARTESIAN_POINT('Ctrl Pts',(-3.30813014804529,-6.16692837593123,
50.1119905397654));
#55101=CARTESIAN_POINT('Ctrl Pts',(3.3997643199154,-6.11688917991012,50.3904143934124));
#55102=CARTESIAN_POINT('Ctrl Pts',(6.9839296753337,-0.446606045933962,50.6688382470596));
#55103=CARTESIAN_POINT('Ctrl Pts',(4.1512077427146,5.63402209323835,50.9472621007067));
#55104=CARTESIAN_POINT('Ctrl Pts',(-2.49567518987983,6.53806821751579,51.2256859543539));
#55105=CARTESIAN_POINT('Ctrl Pts',(-6.84951292507326,1.43488792577199,51.504109808001));
#55106=CARTESIAN_POINT('Ctrl Pts',(-4.90996649670818,-4.98667822016567,
51.7825336616481));
#55107=CARTESIAN_POINT('Ctrl Pts',(1.5408942005697,-6.82644678679344,52.0609575152952));
#55108=CARTESIAN_POINT('Ctrl Pts',(6.57596967842187,-2.3940245317766,52.3393813689425));
#55109=CARTESIAN_POINT('Ctrl Pts',(5.56899459195911,4.23804552889673,52.6178052225894));
#55110=CARTESIAN_POINT('Ctrl Pts',(-0.554814750510634,6.97616737635267,
52.8962290762368));
#55111=CARTESIAN_POINT('Ctrl Pts',(-6.16885611345141,3.30453399465108,53.1746529298836));
#55112=CARTESIAN_POINT('Ctrl Pts',(-6.11490592774493,-3.4033301581101,53.453076783531));
#55113=CARTESIAN_POINT('Ctrl Pts',(-0.442534031138704,-6.98418887928699,
53.7315006371779));
#55114=CARTESIAN_POINT('Ctrl Pts',(5.63644147274139,-4.14792215387804,54.0099244908252));
#55115=CARTESIAN_POINT('Ctrl Pts',(6.53661201758198,2.49948674768936,54.2883483444722));
#55116=CARTESIAN_POINT('Ctrl Pts',(1.43089411388931,6.85034836377748,54.5667721981195));
#55117=CARTESIAN_POINT('Ctrl Pts',(-4.98954009950117,4.90705820892124,54.8451960517665));
#55118=CARTESIAN_POINT('Ctrl Pts',(-6.8255472172519,-1.54487405808249,55.1236199054137));
#55119=CARTESIAN_POINT('Ctrl Pts',(-2.39019004464128,-6.57736438254481,
55.4020437590608));
#55120=CARTESIAN_POINT('Ctrl Pts',(4.24129177791002,-5.56652267801944,55.6804676127079));
#55121=CARTESIAN_POINT('Ctrl Pts',(6.97584270915361,0.558882069331685,55.9588914663551));
#55122=CARTESIAN_POINT('Ctrl Pts',(3.30093671791202,6.17078175392806,56.2373153200021));
#55123=CARTESIAN_POINT('Ctrl Pts',(-3.40689483937537,6.11292059687588,56.5157391736494));
#55124=CARTESIAN_POINT('Ctrl Pts',(-6.98444570903205,0.43846186590818,56.7941630272964));
#55125=CARTESIAN_POINT('Ctrl Pts',(-4.14463515499503,-5.63885893619008,
57.0725868809436));
#55126=CARTESIAN_POINT('Ctrl Pts',(2.50329745582221,-6.53515359558943,57.3510107345907));
#55127=CARTESIAN_POINT('Ctrl Pts',(6.85118147377125,-1.42689981558801,57.6294345882378));
#55128=CARTESIAN_POINT('Ctrl Pts',(4.90414825302692,4.99240028269017,57.907858441885));
#55129=CARTESIAN_POINT('Ctrl Pts',(-1.54885339043013,6.82464532743094,58.1862822955321));
#55130=CARTESIAN_POINT('Ctrl Pts',(-6.57875685075575,2.3863547449836,58.4647061491792));
#55131=CARTESIAN_POINT('Ctrl Pts',(-5.56404887179351,-4.24453658513685,
58.7431300028264));
#55132=CARTESIAN_POINT('Ctrl Pts',(0.562949198166103,-6.97551567058348,
59.0215538564735));
#55133=CARTESIAN_POINT('Ctrl Pts',(6.17270529670647,-3.29733831905118,59.2999777101206));
#55134=CARTESIAN_POINT('Ctrl Pts',(6.11093318797799,3.41045836249916,59.5784015637678));
#55135=CARTESIAN_POINT('Ctrl Pts',(0.434389551626964,6.98470016448157,59.8568254174148));
#55136=CARTESIAN_POINT('Ctrl Pts',(-5.64127448276255,4.14134674718315,60.1352492710621));
#55137=CARTESIAN_POINT('Ctrl Pts',(-6.53369295203398,-2.507107312983,60.4136731247091));
#55138=CARTESIAN_POINT('Ctrl Pts',(-1.42290503222572,-6.85201225477145,
60.6920969783564));
#55139=CARTESIAN_POINT('Ctrl Pts',(4.99525876876051,-4.90123663001426,60.9705208320033));
#55140=CARTESIAN_POINT('Ctrl Pts',(6.82374111763702,1.55283219625988,61.2489446856506));
#55141=CARTESIAN_POINT('Ctrl Pts',(2.38251863410754,6.5801470825812,61.5273685392976));
#55142=CARTESIAN_POINT('Ctrl Pts',(-4.24777994947404,5.56157317412246,61.8057923929448));
#55143=CARTESIAN_POINT('Ctrl Pts',(-6.97518626075355,-0.567016135631398,
62.0842162465919));
#55144=CARTESIAN_POINT('Ctrl Pts',(-3.29373879929166,-6.17462674113279,
62.3626401002391));
#55145=CARTESIAN_POINT('Ctrl Pts',(3.41402072627044,-6.10894370172678,62.6410639538862));
#55146=CARTESIAN_POINT('Ctrl Pts',(6.98495224554912,-0.430317089678943,
62.9194878075333));
#55147=CARTESIAN_POINT('Ctrl Pts',(4.13805693155986,5.64368811163779,63.1979116611804));
#55148=CARTESIAN_POINT('Ctrl Pts',(-2.51091631787676,6.53223008741208,63.4763355148276));
#55149=CARTESIAN_POINT('Ctrl Pts',(-6.85284070649566,1.41890976516039,63.7547593684747));
#55150=CARTESIAN_POINT('Ctrl Pts',(-4.89832334087304,-4.99811555674043,
64.0331832221217));
#55151=CARTESIAN_POINT('Ctrl Pts',(1.55681047421923,-6.82283458817761,64.3116070757691));
#55152=CARTESIAN_POINT('Ctrl Pts',(6.58153507754862,-2.37868171331697,64.5900309294159));
#55153=CARTESIAN_POINT('Ctrl Pts',(5.55909558584776,4.2510218698191,64.8684547830634));
#55154=CARTESIAN_POINT('Ctrl Pts',(-0.571082880344979,6.97485447977578,
65.1468786367103));
#55155=CARTESIAN_POINT('Ctrl Pts',(-6.17654608655382,3.29013815985714,65.4253024903575));
#55156=CARTESIAN_POINT('Ctrl Pts',(-6.10695213879858,-3.41758192947802,
65.7037263440046));
#55157=CARTESIAN_POINT('Ctrl Pts',(-0.426244481448751,-6.98520195214898,
65.9821501976518));
#55158=CARTESIAN_POINT('Ctrl Pts',(5.64609982199524,-4.1347657092437,66.2605740512988));
#55159=CARTESIAN_POINT('Ctrl Pts',(6.53076500222105,2.51472446920854,66.538997904946));
#55160=CARTESIAN_POINT('Ctrl Pts',(1.41491401575025,6.85366682866222,66.8174217585931));
#55161=CARTESIAN_POINT('Ctrl Pts',(-5.00097064565866,4.8954083865937,67.0958456122403));
#55162=CARTESIAN_POINT('Ctrl Pts',(-6.82192573936089,-1.5607882229556,67.3742694658874));
#55163=CARTESIAN_POINT('Ctrl Pts',(-2.37484398391645,-6.58292083518617,
67.6526933195345));
#55164=CARTESIAN_POINT('Ctrl Pts',(4.2542623450698,-5.55661610781171,67.9311171731817));
#55165=CARTESIAN_POINT('Ctrl Pts',(6.97452032776297,0.575149430924237,68.2095410268288));
#55166=CARTESIAN_POINT('Ctrl Pts',(3.28653640197177,6.17846333231709,68.4879648804759));
#55167=CARTESIAN_POINT('Ctrl Pts',(-3.42114197091134,6.10495849987044,68.7663887341231));
#55168=CARTESIAN_POINT('Ctrl Pts',(-6.98544928419626,0.422171728320822,
69.0448125877702));
#55169=CARTESIAN_POINT('Ctrl Pts',(-4.1314730813535,-5.64850961301508,69.3232364414172));
#55170=CARTESIAN_POINT('Ctrl Pts',(2.51853176568377,-6.52929769695893,69.6016602950645));
#55171=CARTESIAN_POINT('Ctrl Pts',(6.85449062099032,-1.41091778535363,69.8800841487114));
#55172=CARTESIAN_POINT('Ctrl Pts',(4.89249176816705,5.00382403454488,70.1585080023588));
#55173=CARTESIAN_POINT('Ctrl Pts',(-1.56476544111709,6.82101457149574,70.4369318560057));
#55174=CARTESIAN_POINT('Ctrl Pts',(-6.58430435502274,2.37100544721029,70.715355709653));
#55175=CARTESIAN_POINT('Ctrl Pts',(-5.55413474085716,-4.25750137412486,
70.9937795633));
#55176=CARTESIAN_POINT('Ctrl Pts',(0.579215785987118,-6.97418380482868,
71.2722034169472));
#55177=CARTESIAN_POINT('Ctrl Pts',(6.18037847777074,-3.28293352685973,71.5506272705943));
#55178=CARTESIAN_POINT('Ctrl Pts',(6.10296278562014,3.42470084936001,71.8290511242415));
#55179=CARTESIAN_POINT('Ctrl Pts',(0.418098831679774,6.98569424160693,72.1074749778885));
#55180=CARTESIAN_POINT('Ctrl Pts',(-5.65091748387798,4.1281790490086,72.3858988315358));
#55181=CARTESIAN_POINT('Ctrl Pts',(-6.52782817212458,-2.52233820600809,
72.6643226851828));
#55182=CARTESIAN_POINT('Ctrl Pts',(-1.40692107532915,-6.85531208319993,
72.9427465388299));
#55183=CARTESIAN_POINT('Ctrl Pts',(5.006675722429,-4.88957348658464,73.2211703924772));
#55184=CARTESIAN_POINT('Ctrl Pts',(6.82010108489192,1.56874212735155,73.4995942461242));
#55185=CARTESIAN_POINT('Ctrl Pts',(2.36716610450353,6.58568563658803,73.7780180997714));
#55186=CARTESIAN_POINT('Ctrl Pts',(-4.26073895588305,5.55165148582763,74.0564419534185));
#55187=CARTESIAN_POINT('Ctrl Pts',(-6.97384491108733,-0.583281944151123,
74.3348658070656));
#55188=CARTESIAN_POINT('Ctrl Pts',(-3.27932953574576,-6.18229152226397,
74.6132896607128));
#55189=CARTESIAN_POINT('Ctrl Pts',(3.42825856361453,-6.10096499672593,74.8917135143599));
#55190=CARTESIAN_POINT('Ctrl Pts',(6.98593682429763,-0.414025792909914,
75.170137368007));
#55191=CARTESIAN_POINT('Ctrl Pts',(4.12488361332866,5.65332343376568,75.4485612216542));
#55192=CARTESIAN_POINT('Ctrl Pts',(-2.52614378888781,6.52635642821742,75.7269850753012));
#55193=CARTESIAN_POINT('Ctrl Pts',(-6.85613121501166,1.40292388703529,76.0054089289485));
#55194=CARTESIAN_POINT('Ctrl Pts',(-4.88665354283862,-5.00952570834149,
76.2838327825954));
#55195=CARTESIAN_POINT('Ctrl Pts',(1.57271828030703,-6.81918527986008,76.5622566362427));
#55196=CARTESIAN_POINT('Ctrl Pts',(6.58706467941239,-2.36332595710137,76.8406804898898));
#55197=CARTESIAN_POINT('Ctrl Pts',(5.54916634356738,4.26397508924365,77.1191043435369));
#55198=CARTESIAN_POINT('Ctrl Pts',(-0.587347904033891,6.9735036466542,77.397528197184));
#55199=CARTESIAN_POINT('Ctrl Pts',(-6.18420246514635,3.27572442985507,77.6759520508313));
#55200=CARTESIAN_POINT('Ctrl Pts',(-6.09896513386704,-3.43181511246536,
77.9543759044783));
#55201=CARTESIAN_POINT('Ctrl Pts',(-0.409952613395948,-6.98617703218592,
78.2327997581254));
#55202=CARTESIAN_POINT('Ctrl Pts',(5.65572746186015,-4.12158677543401,78.5112236117726));
#55203=CARTESIAN_POINT('Ctrl Pts',(6.52488246573783,2.52994851302911,78.7896474654196));
#55204=CARTESIAN_POINT('Ctrl Pts',(1.39892622183076,6.85694801614726,79.0680713190669));
#55205=CARTESIAN_POINT('Ctrl Pts',(-5.01237399131375,4.88373193792135,79.3464951727139));
#55206=CARTESIAN_POINT('Ctrl Pts',(-6.81826715671135,-1.57669389863207,
79.6249190263612));
#55207=CARTESIAN_POINT('Ctrl Pts',(-2.35948500630908,-6.58844148302724,
79.9033428800081));
#55208=CARTESIAN_POINT('Ctrl Pts',(4.26720977310686,-5.54667931492101,80.1817667336555));
#55209=CARTESIAN_POINT('Ctrl Pts',(6.97316001164507,0.591413664253351,80.4601905873024));
#55210=CARTESIAN_POINT('Ctrl Pts',(3.27211821041336,6.18611130576817,80.7386144409497));
#55211=CARTESIAN_POINT('Ctrl Pts',(-3.43537049470339,6.09696319772341,81.0170382945967));
#55212=CARTESIAN_POINT('Ctrl Pts',(-6.9864148651901,0.405879294522616,81.2954621482438));
#55213=CARTESIAN_POINT('Ctrl Pts',(-4.11828853644548,-5.65812956734407,
81.573886001891));
#55214=CARTESIAN_POINT('Ctrl Pts',(2.53375237713854,-6.52340628518699,81.8523098555382));
#55215=CARTESIAN_POINT('Ctrl Pts',(6.85776248632897,-1.39492808107462,82.1307337091853));
#55216=CARTESIAN_POINT('Ctrl Pts',(4.88080867282612,5.01522057037741,82.4091575628324));
#55217=CARTESIAN_POINT('Ctrl Pts',(-1.5806689809751,6.81734671575793,82.6875814164794));
#55218=CARTESIAN_POINT('Ctrl Pts',(-6.58981604696442,2.35564325343243,82.9660052701267));
#55219=CARTESIAN_POINT('Ctrl Pts',(-5.54419040073409,-4.27044300637292,
83.2444291237738));
#55220=CARTESIAN_POINT('Ctrl Pts',(0.595479223427524,-6.97281400617696,
83.522852977421));
#55221=CARTESIAN_POINT('Ctrl Pts',(6.1880180434807,-3.26851087864622,83.801276831068));
#55222=CARTESIAN_POINT('Ctrl Pts',(6.09495918897536,3.43892470912016,84.0797006847152));
#55223=CARTESIAN_POINT('Ctrl Pts',(0.401805837674386,6.98665032322945,84.3581245383623));
#55224=CARTESIAN_POINT('Ctrl Pts',(-5.66052974940107,4.11498889748403,84.6365483920093));
#55225=CARTESIAN_POINT('Ctrl Pts',(-6.52192788706646,-2.53755537992303,
84.9149722456567));
#55226=CARTESIAN_POINT('Ctrl Pts',(-1.39092946612621,-6.8585746252799,85.1933960993035));
#55227=CARTESIAN_POINT('Ctrl Pts',(5.01806544456479,-4.87788374854682,85.4718199529509));
#55228=CARTESIAN_POINT('Ctrl Pts',(6.81642395731267,1.58464352598471,85.7502438065978));
#55229=CARTESIAN_POINT('Ctrl Pts',(2.35180069977754,6.59118837075661,86.0286676602452));
#55230=CARTESIAN_POINT('Ctrl Pts',(-4.27367478794267,5.5416996018528,86.307091513892));
#55231=CARTESIAN_POINT('Ctrl Pts',(-6.97246563036744,-0.59954458017424,
86.5855153675394));
#55232=CARTESIAN_POINT('Ctrl Pts',(-3.26490243578007,-6.1899226776357,86.8639392211865));
#55233=CARTESIAN_POINT('Ctrl Pts',(3.44247775450736,-6.09295310830424,87.1423630748335));
#55234=CARTESIAN_POINT('Ctrl Pts',(6.98688340622387,-0.397732244236107,
87.4207869284808));
#55235=CARTESIAN_POINT('Ctrl Pts',(4.11168785967147,5.66292800721513,87.6992107821278));
#55236=CARTESIAN_POINT('Ctrl Pts',(-2.54135752008998,6.52044727187894,87.977634635775));
#55237=CARTESIAN_POINT('Ctrl Pts',(-6.85938443272403,1.38693037834446,88.2560584894221));
#55238=CARTESIAN_POINT('Ctrl Pts',(-4.87495716607746,-5.02090861290885,
88.5344823430691));
#55239=CARTESIAN_POINT('Ctrl Pts',(1.58861753231004,-6.81549888168934,88.8129061967165));
#55240=CARTESIAN_POINT('Ctrl Pts',(6.59255845393744,-2.34795734665035,89.0913300503635));
#55241=CARTESIAN_POINT('Ctrl Pts',(5.53920691912364,4.27690511671748,89.3697539040107));
#55242=CARTESIAN_POINT('Ctrl Pts',(-0.603609733111337,6.97211488433493,
89.6481777576577));
#55243=CARTESIAN_POINT('Ctrl Pts',(-6.19182520758571,3.26129288304171,89.9266016113048));
#55244=CARTESIAN_POINT('Ctrl Pts',(-6.09094495639199,-3.44602962965707,
90.2050254649521));
#55245=CARTESIAN_POINT('Ctrl Pts',(-0.393658515592726,-6.98711411409408,
90.483449318599));
#55246=CARTESIAN_POINT('Ctrl Pts',(5.66532433997098,-4.10838542413011,90.7618731722463));
#55247=CARTESIAN_POINT('Ctrl Pts',(6.51896444012776,2.54515879634676,91.0402970258934));
#55248=CARTESIAN_POINT('Ctrl Pts',(1.38293081908901,6.86019190838603,91.3187208795406));
#55249=CARTESIAN_POINT('Ctrl Pts',(-5.02375007444307,4.87202892641306,91.5971447331876));
#55250=CARTESIAN_POINT('Ctrl Pts',(-6.81457148920236,-1.59259099860004,
91.8755685868349));
#55251=CARTESIAN_POINT('Ctrl Pts',(-2.34411319535752,-6.59392629604109,
92.1539924404817));
#55252=CARTESIAN_POINT('Ctrl Pts',(4.28013399159945,-5.53671235339405,92.4324162941292));
#55253=CARTESIAN_POINT('Ctrl Pts',(6.97176176819866,0.607674680857242,92.7108401477761));
#55254=CARTESIAN_POINT('Ctrl Pts',(3.25768222165789,6.19372563268397,92.9892640014233));
#55255=CARTESIAN_POINT('Ctrl Pts',(-3.44958033336209,6.08893473392128,93.2676878550705));
#55256=CARTESIAN_POINT('Ctrl Pts',(-6.98734244676171,0.389584653128723,
93.5461117087175));
#55257=CARTESIAN_POINT('Ctrl Pts',(-4.10508159198234,-5.6677187468539,93.8245355623647));
#55258=CARTESIAN_POINT('Ctrl Pts',(2.548959207401,-6.51747939231703,94.1029594160119));
#55259=CARTESIAN_POINT('Ctrl Pts',(6.86099705199147,-1.37893078971957,94.3813832696589));
#55260=CARTESIAN_POINT('Ctrl Pts',(4.86909903054906,5.02658982820138,94.6598071233061));
#55261=CARTESIAN_POINT('Ctrl Pts',(-1.5965639235038,6.81364178016702,94.9382309769533));
#55262=CARTESIAN_POINT('Ctrl Pts',(-6.59529189660259,2.34026824720598,95.2166548306002));
#55263=CARTESIAN_POINT('Ctrl Pts',(-5.53421590551207,-4.28336141149082,
95.4950786842477));
#55264=CARTESIAN_POINT('Ctrl Pts',(0.611739422029957,-6.97140628207867,
95.7735025378944));
#55265=CARTESIAN_POINT('Ctrl Pts',(6.19562395228444,-3.25407045285617,96.051926391542));
#55266=CARTESIAN_POINT('Ctrl Pts',(6.08692244157545,3.45312986441528,96.3303502451886));
#55267=CARTESIAN_POINT('Ctrl Pts',(0.385510658229152,6.98756840414912,96.6087740988361));
#55268=CARTESIAN_POINT('Ctrl Pts',(-5.67011122705018,4.10177636435128,96.8871979524832));
#55269=CARTESIAN_POINT('Ctrl Pts',(-6.51599212895148,-2.55275875196109,
97.1656218061301));
#55270=CARTESIAN_POINT('Ctrl Pts',(-1.37493029159568,-6.86179986326655,
97.4440456597775));
#55271=CARTESIAN_POINT('Ctrl Pts',(5.0294278732187,-4.8661674794814,97.7224695134245));
#55272=CARTESIAN_POINT('Ctrl Pts',(6.8127097548993,1.6005363056711,98.0008933670716));
#55273=CARTESIAN_POINT('Ctrl Pts',(2.33642250350259,6.59665525515757,98.2793172207188));
#55274=CARTESIAN_POINT('Ctrl Pts',(-4.28658737529433,5.53171757632644,98.5577410743658));
#55275=CARTESIAN_POINT('Ctrl Pts',(-6.97104842609587,-0.615803955247596,
98.8361649280132));
#55276=CARTESIAN_POINT('Ctrl Pts',(-3.25045757786441,-6.19752016574172,
99.11458878166));
#55277=CARTESIAN_POINT('Ctrl Pts',(3.45667822160986,-6.08490808003864,99.3930126353075));
#55278=CARTESIAN_POINT('Ctrl Pts',(6.98779198617956,-0.381436532279055,
99.6714364889542));
#55279=CARTESIAN_POINT('Ctrl Pts',(4.09846974236059,5.67250177974641,99.9498603426018));
#55280=CARTESIAN_POINT('Ctrl Pts',(-2.55655742873526,6.51450265053672,100.228284196249));
#55281=CARTESIAN_POINT('Ctrl Pts',(-6.86260034193842,1.3709293260774,100.506708049896));
#55282=CARTESIAN_POINT('Ctrl Pts',(-4.86323427420664,-5.03226420853012,
100.785131903543));
#55283=CARTESIAN_POINT('Ctrl Pts',(1.60450814375138,-6.81177541371608,101.06355575719));
#55284=CARTESIAN_POINT('Ctrl Pts',(6.59801637124282,-2.33257596555462,101.341979610837));
#55285=CARTESIAN_POINT('Ctrl Pts',(5.52921736668622,4.28981188191358,101.620403464484));
#55286=CARTESIAN_POINT('Ctrl Pts',(-0.619868279128679,6.97068820037178,
101.898827318132));
#55287=CARTESIAN_POINT('Ctrl Pts',(-6.19941427241141,3.2468435979106,102.177251171778));
#55288=CARTESIAN_POINT('Ctrl Pts',(-6.08289164999546,-3.46022540373989,
102.455675025426));
#55289=CARTESIAN_POINT('Ctrl Pts',(-0.37736227666324,-6.98801319277683,
102.734098879073));
#55290=CARTESIAN_POINT('Ctrl Pts',(5.6748904041298,-4.09516172713445,103.01252273272));
#55291=CARTESIAN_POINT('Ctrl Pts',(6.51301095757923,2.5603552364321,103.290946586367));
#55292=CARTESIAN_POINT('Ctrl Pts',(1.3669278945249,6.86339848773486,103.569370440014));
#55293=CARTESIAN_POINT('Ctrl Pts',(-5.03509883317134,4.86029941572203,103.847794293661));
#55294=CARTESIAN_POINT('Ctrl Pts',(-6.81083875693507,-1.60847943639435,
104.126218147308));
#55295=CARTESIAN_POINT('Ctrl Pts',(-2.32872863466976,-6.59937524439553,
104.404642000956));
#55296=CARTESIAN_POINT('Ctrl Pts',(4.29303493025233,-5.52671527744145,104.683065854603));
#55297=CARTESIAN_POINT('Ctrl Pts',(6.97032560502893,0.623932392291463,104.96148970825));
#55298=CARTESIAN_POINT('Ctrl Pts',(3.24322851422338,6.20130627164954,105.239913561897));
#55299=CARTESIAN_POINT('Ctrl Pts',(-3.4637714095994,6.08087315213145,105.518337415544));
#55300=CARTESIAN_POINT('Ctrl Pts',(-6.98823202386593,0.37328789276662,105.796761269191));
#55301=CARTESIAN_POINT('Ctrl Pts',(-4.09185231979714,-5.6772770993886,106.075185122838));
#55302=CARTESIAN_POINT('Ctrl Pts',(2.56415217376077,-6.51151705058585,106.353608976486));
#55303=CARTESIAN_POINT('Ctrl Pts',(6.86419430038473,-1.36292599829824,106.632032830133));
#55304=CARTESIAN_POINT('Ctrl Pts',(4.85736290502502,5.03793174617901,106.91045668378));
#55305=CARTESIAN_POINT('Ctrl Pts',(-1.61245018225011,6.80989978487445,107.188880537427));
#55306=CARTESIAN_POINT('Ctrl Pts',(-6.60073187415369,2.32488051215605,107.467304391074));
#55307=CARTESIAN_POINT('Ctrl Pts',(-5.52421130944283,-4.29625651921488,
107.745728244721));
#55308=CARTESIAN_POINT('Ctrl Pts',(0.627996293354289,-6.96996064019049,
108.024152098368));
#55309=CARTESIAN_POINT('Ctrl Pts',(6.20319616281283,-3.2396123280318,108.302575952016));
#55310=CARTESIAN_POINT('Ctrl Pts',(6.07885258713292,3.46731623798289,108.580999805663));
#55311=CARTESIAN_POINT('Ctrl Pts',(0.369213381974334,6.98844847937241,108.85942365931));
#55312=CARTESIAN_POINT('Ctrl Pts',(-5.67966186471135,4.08854152147376,109.137847512957));
#55313=CARTESIAN_POINT('Ctrl Pts',(-6.51002093006455,-2.56794823943043,
109.416271366604));
#55314=CARTESIAN_POINT('Ctrl Pts',(-1.35892363875792,-6.86498777961741,
109.694695220251));
#55315=CARTESIAN_POINT('Ctrl Pts',(5.04076294658997,-4.85442474311395,109.973119073898));
#55316=CARTESIAN_POINT('Ctrl Pts',(6.80895849785357,1.61642037996899,110.251542927545));
#55317=CARTESIAN_POINT('Ctrl Pts',(2.32103159932129,6.60208626005625,110.529966781192));
#55318=CARTESIAN_POINT('Ctrl Pts',(-4.29947664770616,5.52170546354129,110.80839063484));
#55319=CARTESIAN_POINT('Ctrl Pts',(-6.96959330598069,-0.632059980935899,
111.086814488487));
#55320=CARTESIAN_POINT('Ctrl Pts',(-3.23599504056484,-6.20508394525901,
111.365238342134));
#55321=CARTESIAN_POINT('Ctrl Pts',(3.47085988768531,-6.07682995568647,111.643662195781));
#55322=CARTESIAN_POINT('Ctrl Pts',(6.98866255922268,-0.365138745671669,
111.922086049428));
#55323=CARTESIAN_POINT('Ctrl Pts',(4.08522933328995,5.68204469928737,112.200509903075));
#55324=CARTESIAN_POINT('Ctrl Pts',(-2.57174343215052,6.50852259652388,112.478933756722));
#55325=CARTESIAN_POINT('Ctrl Pts',(-6.86577892516314,1.35492081726468,112.75735761037));
#55326=CARTESIAN_POINT('Ctrl Pts',(-4.85148493098777,-5.04359243344176,
113.035781464017));
#55327=CARTESIAN_POINT('Ctrl Pts',(1.62039002820123,-6.80801489619239,113.314205317664));
#55328=CARTESIAN_POINT('Ctrl Pts',(6.60343840164274,-2.31718189747404,113.592629171311));
#55329=CARTESIAN_POINT('Ctrl Pts',(5.5191977405888,4.30269531463148,113.871053024958));
#55330=CARTESIAN_POINT('Ctrl Pts',(-0.636123453654769,6.9692236025243,114.149476878605));
#55331=CARTESIAN_POINT('Ctrl Pts',(-6.20696961834626,3.23237665305234,114.427900732252));
#55332=CARTESIAN_POINT('Ctrl Pts',(-6.07480525847982,-3.47440235750226,
114.706324585899));
#55333=CARTESIAN_POINT('Ctrl Pts',(-0.361063985243409,-6.98887426334396,
114.984748439546));
#55334=CARTESIAN_POINT('Ctrl Pts',(5.68442560230666,-4.08191575637137,115.263172293194));
#55335=CARTESIAN_POINT('Ctrl Pts',(6.50702205047326,2.57553775063117,115.541596146841));
#55336=CARTESIAN_POINT('Ctrl Pts',(1.35091753517889,6.86656773675302,115.820020000488));
#55337=CARTESIAN_POINT('Ctrl Pts',(-5.04642020577243,4.84854346964561,116.098443854135));
#55338=CARTESIAN_POINT('Ctrl Pts',(-6.80706898021171,-1.62435912559722,
116.376867707782));
#55339=CARTESIAN_POINT('Ctrl Pts',(-2.3133314079231,-6.60478829845354,116.655291561429));
#55340=CARTESIAN_POINT('Ctrl Pts',(4.30591251889657,-5.51668814143787,116.933715415077));
#55341=CARTESIAN_POINT('Ctrl Pts',(6.96885152994704,0.640186710129389,117.212139268724));
#55342=CARTESIAN_POINT('Ctrl Pts',(3.22875716672446,6.20885318143358,117.490563122371));
#55343=CARTESIAN_POINT('Ctrl Pts',(-3.47794364622938,6.07277849620123,117.768986976018));
#55344=CARTESIAN_POINT('Ctrl Pts',(-6.9890835916643,0.356989102074914,118.047410829665));
#55345=CARTESIAN_POINT('Ctrl Pts',(-4.07860079184459,-5.68680457295987,
118.325834683312));
#55346=CARTESIAN_POINT('Ctrl Pts',(2.57933119358243,-6.5055192924227,118.604258536959));
#55347=CARTESIAN_POINT('Ctrl Pts',(6.86735421411885,-1.34691379386167,118.882682390606));
#55348=CARTESIAN_POINT('Ctrl Pts',(4.84560036008754,5.04924626262106,119.161106244254));
#55349=CARTESIAN_POINT('Ctrl Pts',(-1.62832767080822,6.80612075023288,119.439530097901));
#55350=CARTESIAN_POINT('Ctrl Pts',(-6.60613595002934,2.30948013197741,119.717953951548));
#55351=CARTESIAN_POINT('Ctrl Pts',(-5.51417666694228,-4.30912825940853,
119.996377805195));
#55352=CARTESIAN_POINT('Ctrl Pts',(0.644249748980212,-6.96847708837439,
120.274801658842));
#55353=CARTESIAN_POINT('Ctrl Pts',(6.21073463387792,-3.22513658281319,120.553225512489));
#55354=CARTESIAN_POINT('Ctrl Pts',(6.0707496695447,3.48148375266606,120.831649366136));
#55355=CARTESIAN_POINT('Ctrl Pts',(0.352914097542206,6.98929054410621,121.110073219783));
#55356=CARTESIAN_POINT('Ctrl Pts',(-5.68918161042058,4.07528444084858,121.38849707343));
#55357=CARTESIAN_POINT('Ctrl Pts',(-6.5040143229163,-2.58312375973728,121.666920927078));
#55358=CARTESIAN_POINT('Ctrl Pts',(-1.34290959461152,-6.86813835695045,
121.945344780725));
#55359=CARTESIAN_POINT('Ctrl Pts',(5.05207060290854,-4.84265560339497,122.223768634372));
#55360=CARTESIAN_POINT('Ctrl Pts',(6.80517020680153,1.63229566263774,122.502192488019));
#55361=CARTESIAN_POINT('Ctrl Pts',(2.30562807052473,6.60748135562364,122.780616341666));
#55362=CARTESIAN_POINT('Ctrl Pts',(-4.31234253427801,5.51166331850034,123.059040195313));
#55363=CARTESIAN_POINT('Ctrl Pts',(-6.96810027943676,-0.648312569854052,
123.337464048961));
#55364=CARTESIAN_POINT('Ctrl Pts',(-3.22151489971119,-6.21261397309853,
123.615887902608));
#55365=CARTESIAN_POINT('Ctrl Pts',(3.48502267025022,-6.0687187828655,123.894311756255));
#55366=CARTESIAN_POINT('Ctrl Pts',(6.98949513071799,-0.348838966108577,
124.172735609902));
#55367=CARTESIAN_POINT('Ctrl Pts',(4.07196668540431,5.69155670081135,124.451159463549));
#55368=CARTESIAN_POINT('Ctrl Pts',(-2.58691541173027,6.5025071671437,124.729583317196));
#55369=CARTESIAN_POINT('Ctrl Pts',(-6.86892023310093,1.33890489219211,125.008007170843));
#55370=CARTESIAN_POINT('Ctrl Pts',(-4.83970907194496,-5.0548931376893,125.28643102449));
#55371=CARTESIAN_POINT('Ctrl Pts',(1.63626285686831,-6.80421751637518,125.564854878138));
#55372=CARTESIAN_POINT('Ctrl Pts',(6.60882497336411,-2.30177491117929,125.843278731785));
#55373=CARTESIAN_POINT('Ctrl Pts',(5.50914723106459,4.31555475009168,126.121702585432));
#55374=CARTESIAN_POINT('Ctrl Pts',(-0.652373536370679,6.96772222168401,
126.400126439079));
#55375=CARTESIAN_POINT('Ctrl Pts',(-6.21449428566708,3.21789000684206,126.678550292726));
#55376=CARTESIAN_POINT('Ctrl Pts',(-6.06668000757257,-3.48855641025641,
126.956974146373));
#55377=CARTESIAN_POINT('Ctrl Pts',(-0.344774716028633,-6.98970488068336,
127.23539800002));
#55378=CARTESIAN_POINT('Ctrl Pts',(5.69395062653325,-4.068633309877,127.513821853667));
#55379=CARTESIAN_POINT('Ctrl Pts',(6.50095858268405,2.59067930412174,127.792245707314));
#55380=CARTESIAN_POINT('Ctrl Pts',(1.3349737866748,6.86975052961293,128.070669560962));
#55381=CARTESIAN_POINT('Ctrl Pts',(-5.05785378002051,4.83666505803512,128.349093414609));
#55382=CARTESIAN_POINT('Ctrl Pts',(-6.80299848840007,-1.64004852846079,
128.627517268256));
#55383=CARTESIAN_POINT('Ctrl Pts',(-2.29841954027217,-6.61050809651445,
128.905941121903));
#55384=CARTESIAN_POINT('Ctrl Pts',(4.31970722031227,-5.50598355952033,129.18436497555));
#55385=CARTESIAN_POINT('Ctrl Pts',(6.96556103235851,0.655211661793067,129.462788829197));
#55386=CARTESIAN_POINT('Ctrl Pts',(3.21764772889245,6.21870871851334,129.741212682844));
#55387=CARTESIAN_POINT('Ctrl Pts',(-3.49865171312285,6.06000128588926,130.019636536492));
#55388=CARTESIAN_POINT('Ctrl Pts',(-6.39654705541885,1.30279187935603,130.251656414531));
#55389=CARTESIAN_POINT('Ctrl Pts',(-5.53817824125726,-2.69171018261493,
130.437272316962));
#55390=CARTESIAN_POINT('Ctrl Pts',(-4.23949710241608,-4.24338993046111,
130.530080268178));
#55391=CARTESIAN_POINT('Ctrl Pts',(-3.43710408716141,-4.81604049573073,
130.576484243786));
#55392=CARTESIAN_POINT('Ctrl Pts',(-2.85711522928025,-4.00149011032068,
-10.));
#55393=CARTESIAN_POINT('Ctrl Pts',(-2.41648365696274,-4.31442211364657,
-9.96932881922757));
#55394=CARTESIAN_POINT('Ctrl Pts',(-1.17990489524751,-4.91804358772338,
-9.89225366284727));
#55395=CARTESIAN_POINT('Ctrl Pts',(1.92453937789233,-5.07348089440844,-9.72237055525127));
#55396=CARTESIAN_POINT('Ctrl Pts',(5.43970692864372,-2.05961707410548,-9.49035067721199));
#55397=CARTESIAN_POINT('Ctrl Pts',(4.67141455431437,3.47170793039274,-9.21192682356487));
#55398=CARTESIAN_POINT('Ctrl Pts',(-0.394303111254869,5.8022423708097,-8.93350296991773));
#55399=CARTESIAN_POINT('Ctrl Pts',(-4.31724444146487,3.30287017342899,-8.70114717405969));
#55400=CARTESIAN_POINT('Ctrl Pts',(-4.90982483510101,0.82872126176219,-8.56159932941736));
#55401=CARTESIAN_POINT('Ctrl Pts',(-4.91001919821333,6.39834157814545E-5,
-8.51485943599074));
#55402=CARTESIAN_POINT('Ctrl Pts',(-5.90701629014678,0.000721185244744792,
126.811624807795));
#55403=CARTESIAN_POINT('Ctrl Pts',(-5.90589710669071,-1.0324812503633,126.860074587321));
#55404=CARTESIAN_POINT('Ctrl Pts',(-5.6483729107334,-2.06620547501384,126.908524366847));
#55405=CARTESIAN_POINT('Ctrl Pts',(-5.1376648386644,-2.95434008581106,126.956974146373));
#55406=CARTESIAN_POINT('Ctrl Pts',(-4.15937824372468,-4.65560590039867,
127.049782097589));
#55407=CARTESIAN_POINT('Ctrl Pts',(-2.25207647987663,-5.82265539054102,
127.142590048805));
#55408=CARTESIAN_POINT('Ctrl Pts',(-0.29197137419231,-5.91933487381112,
127.23539800002));
#55409=CARTESIAN_POINT('Ctrl Pts',(1.66813373149212,-6.01601435708123,127.328205951236));
#55410=CARTESIAN_POINT('Ctrl Pts',(3.68104217901263,-5.04232383347917,127.421013902452));
#55411=CARTESIAN_POINT('Ctrl Pts',(4.82199772879814,-3.44559313601152,127.513821853667));
#55412=CARTESIAN_POINT('Ctrl Pts',(5.96295327858346,-1.84886243854414,127.606629804883));
#55413=CARTESIAN_POINT('Ctrl Pts',(6.23195593063374,0.370908432788888,127.699437756099));
#55414=CARTESIAN_POINT('Ctrl Pts',(5.50545979065741,2.19397240603706,127.792245707315));
#55415=CARTESIAN_POINT('Ctrl Pts',(4.77896365068096,4.01703637928555,127.88505365853));
#55416=CARTESIAN_POINT('Ctrl Pts',(3.05696871867794,5.44339345444921,127.977861609746));
#55417=CARTESIAN_POINT('Ctrl Pts',(1.13049999156036,5.81772441343478,128.070669560962));
#55418=CARTESIAN_POINT('Ctrl Pts',(-0.79596873555699,6.19205537242031,128.163477512177));
#55419=CARTESIAN_POINT('Ctrl Pts',(-2.92691125778872,5.51436021522773,128.256285463393));
#55420=CARTESIAN_POINT('Ctrl Pts',(-4.28323997030115,4.09606037221553,128.349093414609));
#55421=CARTESIAN_POINT('Ctrl Pts',(-5.31857665971544,3.01341878945275,128.419937212337));
#55422=CARTESIAN_POINT('Ctrl Pts',(-5.90255806307964,1.49923850233953,128.490781010066));
#55423=CARTESIAN_POINT('Ctrl Pts',(-5.91642361182645,-0.00541095714722729,
128.561624807795));
#55424=CARTESIAN_POINT('Origin',(0.,0.,-13.2351405640096));
#55425=CARTESIAN_POINT('Ctrl Pts',(2.85706463458369,-4.00329423554042,-10.));
#55426=CARTESIAN_POINT('Ctrl Pts',(3.52391651473643,-3.52737645103792,-9.95360512071162));
#55427=CARTESIAN_POINT('Ctrl Pts',(4.6032797975914,-2.23787345781402,-9.86081536213486));
#55428=CARTESIAN_POINT('Ctrl Pts',(5.31710770646798,1.0817198372055,-9.67523584498136));
#55429=CARTESIAN_POINT('Ctrl Pts',(2.91000325553484,5.03585724930024,-9.44326144853946));
#55430=CARTESIAN_POINT('Ctrl Pts',(-2.67142550958262,5.17047615300083,-9.16489217280919));
#55431=CARTESIAN_POINT('Ctrl Pts',(-4.84847440842237,1.94359242658305,-8.97051854463248));
#55432=CARTESIAN_POINT('Ctrl Pts',(-4.92512433492993,0.157117410974401,
-8.86893467503253));
#55433=CARTESIAN_POINT('Ctrl Pts',(-4.9240923050422,0.00237935796991912,
-8.86014056400933));
#55434=CARTESIAN_POINT('Ctrl Pts',(3.4371040871608,-4.81604049573117,-10.5764842437858));
#55435=CARTESIAN_POINT('Ctrl Pts',(4.23933981366781,-4.24350218404385,-10.5300893644975));
#55436=CARTESIAN_POINT('Ctrl Pts',(5.53783474658711,-2.69220510984897,-10.4372996059207));
#55437=CARTESIAN_POINT('Ctrl Pts',(6.39658354541614,1.30132991344342,-10.2517200887672));
#55438=CARTESIAN_POINT('Ctrl Pts',(3.50079027340594,6.05823379856682,-10.0197456923253));
#55439=CARTESIAN_POINT('Ctrl Pts',(-3.21377662457789,6.22018294683352,-9.74137641659503));
#55440=CARTESIAN_POINT('Ctrl Pts',(-6.96458399641983,0.660629702264095,
-9.46300714086476));
#55441=CARTESIAN_POINT('Ctrl Pts',(-4.3248127554248,-5.50138505625064,-9.18463786513449));
#55442=CARTESIAN_POINT('Ctrl Pts',(2.29049378023627,-6.61276642800579,-8.90626858940423));
#55443=CARTESIAN_POINT('Ctrl Pts',(6.80029139153989,-1.64926970870278,-8.62789931367396));
#55444=CARTESIAN_POINT('Ctrl Pts',(5.06509383187957,4.82841021736868,-8.3495300379437));
#55445=CARTESIAN_POINT('Ctrl Pts',(-1.32276848152976,6.87163827279611,-8.07116076221342));
#55446=CARTESIAN_POINT('Ctrl Pts',(-6.49543867311718,2.60324077919988,-7.79279148648315));
#55447=CARTESIAN_POINT('Ctrl Pts',(-5.70232919786885,-4.05608148955149,
-7.51442221075289));
#55448=CARTESIAN_POINT('Ctrl Pts',(0.328315906814816,-6.99003262884612,
-7.23605293502261));
#55449=CARTESIAN_POINT('Ctrl Pts',(6.05737171330259,-3.50376713762688,-6.95768365929234));
#55450=CARTESIAN_POINT('Ctrl Pts',(6.22288606259671,3.20061689120149,-6.67931438356208));
#55451=CARTESIAN_POINT('Ctrl Pts',(0.672806576516693,6.96531258652612,-6.4009451078318));
#55452=CARTESIAN_POINT('Ctrl Pts',(-5.49522514782519,4.33251896898317,-6.12257583210154));
#55453=CARTESIAN_POINT('Ctrl Pts',(-6.61601726927951,-2.27959531258102,
-5.84420655637128));
#55454=CARTESIAN_POINT('Ctrl Pts',(-1.66014241893913,-6.79795287504758,
-5.565837280641));
#55455=CARTESIAN_POINT('Ctrl Pts',(4.82053563726988,-5.0725406571401,-5.28746800491073));
#55456=CARTESIAN_POINT('Ctrl Pts',(6.87365889457675,1.31188753052232,-5.00909872918046));
#55457=CARTESIAN_POINT('Ctrl Pts',(2.61347841437683,6.49137623247661,-4.73072945345019));
#55458=CARTESIAN_POINT('Ctrl Pts',(-4.047123996549,5.70867950871538,-4.45236017771992));
#55459=CARTESIAN_POINT('Ctrl Pts',(-6.99053269373454,-0.3173128977453,-4.17399090198966));
#55460=CARTESIAN_POINT('Ctrl Pts',(-3.51329185906621,-6.05186045779054,
-3.89562162625939));
#55461=CARTESIAN_POINT('Ctrl Pts',(3.19082973901377,-6.22790817328656,-3.61725235052912));
#55462=CARTESIAN_POINT('Ctrl Pts',(6.96424488227746,-0.683760135240154,
-3.33888307479885));
#55463=CARTESIAN_POINT('Ctrl Pts',(4.34115529651584,5.48840645098574,-3.06051379906858));
#55464=CARTESIAN_POINT('Ctrl Pts',(-2.26918930552874,6.61959323301065,-2.78214452333831));
#55465=CARTESIAN_POINT('Ctrl Pts',(-6.79533377574579,1.67083020092733,-2.50377524760804));
#55466=CARTESIAN_POINT('Ctrl Pts',(-5.08011463276461,-4.81255337613399,
-2.22540597187778));
#55467=CARTESIAN_POINT('Ctrl Pts',(1.30107731735387,-6.87571323530137,-1.9470366961475));
#55468=CARTESIAN_POINT('Ctrl Pts',(6.48725855983418,-2.62368272834031,-1.66866742041724));
#55469=CARTESIAN_POINT('Ctrl Pts',(5.715036454269,4.03814227174553,-1.39029814468696));
#55470=CARTESIAN_POINT('Ctrl Pts',(-0.306320093554309,6.99102300674048,
-1.1119288689567));
#55471=CARTESIAN_POINT('Ctrl Pts',(-6.04632841794436,3.5228039035726,-0.833559593226426));
#55472=CARTESIAN_POINT('Ctrl Pts',(-6.23291796674688,-3.18103258398395,
-0.555190317496161));
#55473=CARTESIAN_POINT('Ctrl Pts',(-0.694710370832787,-6.96316107678336,
-0.276821041765888));
#55474=CARTESIAN_POINT('Ctrl Pts',(5.48157331859047,-4.34978029715457,0.0015482339643776));
#55475=CARTESIAN_POINT('Ctrl Pts',(6.62315328652935,2.25877737365066,0.27991750969465));
#55476=CARTESIAN_POINT('Ctrl Pts',(1.68151360901781,6.79269804004795,0.558286785424916));
#55477=CARTESIAN_POINT('Ctrl Pts',(-4.80455908671799,5.08767595890522,0.836656061155189));
#55478=CARTESIAN_POINT('Ctrl Pts',(-6.87775064266443,-1.29026384042682,
1.11502533688545));
#55479=CARTESIAN_POINT('Ctrl Pts',(-2.63388051878106,-6.48312487103019,
1.39339461261573));
#55480=CARTESIAN_POINT('Ctrl Pts',(4.02915054287043,-5.72137925534322,1.67176388834599));
#55481=CARTESIAN_POINT('Ctrl Pts',(6.99149604335227,0.295326525009105,1.95013316407626));
#55482=CARTESIAN_POINT('Ctrl Pts',(3.53230723199496,6.04078143118759,2.22850243980653));
#55483=CARTESIAN_POINT('Ctrl Pts',(-3.17122756047482,6.23791234631183,2.5068717155368));
#55484=CARTESIAN_POINT('Ctrl Pts',(-6.96206005518643,0.705658889664277,
2.78524099126707));
#55485=CARTESIAN_POINT('Ctrl Pts',(-4.35839454142477,-5.47472663261496,
3.06361026699734));
#55486=CARTESIAN_POINT('Ctrl Pts',(2.24835985613929,-6.62669696288323,3.34197954272761));
#55487=CARTESIAN_POINT('Ctrl Pts',(6.79004550846843,-1.69219285943192,3.62034881845788));
#55488=CARTESIAN_POINT('Ctrl Pts',(5.09522470478115,4.79655291729097,3.89871809418815));
#55489=CARTESIAN_POINT('Ctrl Pts',(-1.27944717303976,6.87977104357299,4.17708736991841));
#55490=CARTESIAN_POINT('Ctrl Pts',(-6.47897515162715,2.64407179652568,4.45545664564868));
#55491=CARTESIAN_POINT('Ctrl Pts',(-5.72770790931377,-4.02014885124534,
4.73382592137895));
#55492=CARTESIAN_POINT('Ctrl Pts',(0.284332226209421,-6.99195179229115,
5.01219519710922));
#55493=CARTESIAN_POINT('Ctrl Pts',(6.03521950757322,-3.54180182618849,5.29056447283949));
#55494=CARTESIAN_POINT('Ctrl Pts',(6.24289130157187,3.16141469556638,5.56893374856976));
#55495=CARTESIAN_POINT('Ctrl Pts',(0.716605663635154,6.96094181870749,5.84730302430003));
#55496=CARTESIAN_POINT('Ctrl Pts',(-5.46786640944469,4.36699800882151,6.12567230003029));
#55497=CARTESIAN_POINT('Ctrl Pts',(-6.63022425359814,-2.23793677917492,
6.40404157576057));
#55498=CARTESIAN_POINT('Ctrl Pts',(-1.70286792561071,-6.78737618734301,
6.68241085149083));
#55499=CARTESIAN_POINT('Ctrl Pts',(4.78853488756881,-5.10276085184492,6.96078012722111));
#55500=CARTESIAN_POINT('Ctrl Pts',(6.88177443307402,1.26862734200135,7.23914940295137));
#55501=CARTESIAN_POINT('Ctrl Pts',(2.6542565363518,6.47480941185285,7.51751867868164));
#55502=CARTESIAN_POINT('Ctrl Pts',(-4.01113721911641,5.73402240054953,7.79588795441191));
#55503=CARTESIAN_POINT('Ctrl Pts',(-6.99239025243653,-0.273337224349726,
8.07425723014218));
#55504=CARTESIAN_POINT('Ctrl Pts',(-3.5512876626729,-6.02964266084915,8.35262650587245));
#55505=CARTESIAN_POINT('Ctrl Pts',(3.15159401352083,-6.24785482021824,8.63099578160272));
#55506=CARTESIAN_POINT('Ctrl Pts',(6.95980637011251,-0.727550665676303,
8.90936505733298));
#55507=CARTESIAN_POINT('Ctrl Pts',(4.37559067807077,5.46099266604204,9.18773433306327));
#55508=CARTESIAN_POINT('Ctrl Pts',(-2.22750816853013,6.63373514995257,9.4661036087935));
#55509=CARTESIAN_POINT('Ctrl Pts',(-6.78469008327218,1.71353878115812,9.74447288452382));
#55510=CARTESIAN_POINT('Ctrl Pts',(-5.11028438146206,-4.78050501737731,
10.022842160254));
#55511=CARTESIAN_POINT('Ctrl Pts',(1.25780437406543,-6.88376080621389,10.3012114359844));
#55512=CARTESIAN_POINT('Ctrl Pts',(6.47062766200786,-2.66443471307583,10.5795807117146));
#55513=CARTESIAN_POINT('Ctrl Pts',(5.74032271343675,4.00211566876656,10.8579499874449));
#55514=CARTESIAN_POINT('Ctrl Pts',(-0.262341546617244,6.99281142270426,
11.1363192631751));
#55515=CARTESIAN_POINT('Ctrl Pts',(-6.02405090480507,3.56076471799275,11.4146885389054));
#55516=CARTESIAN_POINT('Ctrl Pts',(-6.25280288997779,-3.14176553862156,
11.6930578146357));
#55517=CARTESIAN_POINT('Ctrl Pts',(-0.738493868724291,-6.95865371220909,
11.9714270903659));
#55518=CARTESIAN_POINT('Ctrl Pts',(5.45410541940353,-4.38417252792563,12.2497963660962));
#55519=CARTESIAN_POINT('Ctrl Pts',(6.63722964326527,2.21707404999144,12.5281656418265));
#55520=CARTESIAN_POINT('Ctrl Pts',(1.72420539968851,6.78198720289781,12.8065349175568));
#55521=CARTESIAN_POINT('Ctrl Pts',(-4.77246332657172,5.11779527502935,13.084904193287));
#55522=CARTESIAN_POINT('Ctrl Pts',(-6.88573015808093,-1.24697829599372,
13.3632734690173));
#55523=CARTESIAN_POINT('Ctrl Pts',(-2.67460630153053,-6.4664299124322,13.6416427447476));
#55524=CARTESIAN_POINT('Ctrl Pts',(3.99308422250307,-5.74660883239687,13.9200120204778));
#55525=CARTESIAN_POINT('Ctrl Pts',(6.99321530205292,0.251345220200505,14.1983812962081));
#55526=CARTESIAN_POINT('Ctrl Pts',(3.57023296871443,6.01844425326751,14.4767505719383));
#55527=CARTESIAN_POINT('Ctrl Pts',(-3.13192929517096,6.25773549861567,14.7551198476687));
#55528=CARTESIAN_POINT('Ctrl Pts',(-6.95748384784736,0.749435245720291,
15.0334891233989));
#55529=CARTESIAN_POINT('Ctrl Pts',(-4.39274353716615,-5.44720468655893,
15.3118583991292));
#55530=CARTESIAN_POINT('Ctrl Pts',(2.2066344493589,-6.64070772489554,15.5902276748594));
#55531=CARTESIAN_POINT('Ctrl Pts',(6.77926755290319,-1.73486775482704,15.8685969505897));
#55532=CARTESIAN_POINT('Ctrl Pts',(5.12529351397489,4.7644098350364,16.14696622632));
#55533=CARTESIAN_POINT('Ctrl Pts',(-1.23614913455534,6.88768248380563,16.4253355020503));
#55534=CARTESIAN_POINT('Ctrl Pts',(-6.46221617350552,2.68477127656499,16.7037047777805));
#55535=CARTESIAN_POINT('Ctrl Pts',(-5.75288074188647,-3.9840429026576,16.9820740535108));
#55536=CARTESIAN_POINT('Ctrl Pts',(0.240348272289746,-6.99360188948385,
17.2604433292411));
#55537=CARTESIAN_POINT('Ctrl Pts',(6.01282272009998,-3.57969239142614,17.5388126049713));
#55538=CARTESIAN_POINT('Ctrl Pts',(6.26265263393503,3.12208530749102,17.8171818807016));
#55539=CARTESIAN_POINT('Ctrl Pts',(0.760374769609702,6.95629677992002,18.0955511564318));
#55540=CARTESIAN_POINT('Ctrl Pts',(-5.44029048457163,4.40130368459892,18.3739204321622));
#55541=CARTESIAN_POINT('Ctrl Pts',(-6.64416938624315,-2.1961893924464,18.6522897078924));
#55542=CARTESIAN_POINT('Ctrl Pts',(-1.74552582020905,-6.77653114001317,
18.9306589836227));
#55543=CARTESIAN_POINT('Ctrl Pts',(4.75634456268516,-5.13277907975786,19.2090282593529));
#55544=CARTESIAN_POINT('Ctrl Pts',(6.88961777856047,1.22531691652745,19.4873975350832));
#55545=CARTESIAN_POINT('Ctrl Pts',(2.69492961304441,6.45798645564707,19.7657668108135));
#55546=CARTESIAN_POINT('Ctrl Pts',(-3.97499173158654,5.75913842639707,20.0441360865438));
#55547=CARTESIAN_POINT('Ctrl Pts',(-6.99397118404114,-0.22935073007701,
20.322505362274));
#55548=CARTESIAN_POINT('Ctrl Pts',(-3.58914296273775,-6.00718631920259,
20.6008746380043));
#55549=CARTESIAN_POINT('Ctrl Pts',(3.11223359992263,-6.26755428377747,20.8792439137345));
#55550=CARTESIAN_POINT('Ctrl Pts',(6.9550925113623,-0.771312413342824,21.1576131894649));
#55551=CARTESIAN_POINT('Ctrl Pts',(4.40985294905754,5.43336283053807,21.4359824651951));
#55552=CARTESIAN_POINT('Ctrl Pts',(-2.18573890508088,6.64761461874863,21.7143517409254));
#55553=CARTESIAN_POINT('Ctrl Pts',(-6.77377797099395,1.75617956948081,21.9927210166556));
#55554=CARTESIAN_POINT('Ctrl Pts',(-5.1402519538691,-4.74826752946058,22.2710902923859));
#55555=CARTESIAN_POINT('Ctrl Pts',(1.21448166869439,-6.89153603756012,22.5494595681161));
#55556=CARTESIAN_POINT('Ctrl Pts',(6.45374076931547,-2.70508128585077,22.8278288438465));
#55557=CARTESIAN_POINT('Ctrl Pts',(5.76538187045557,3.96593073167031,23.1061981195766));
#55558=CARTESIAN_POINT('Ctrl Pts',(-0.218352620755356,6.99432318481166,
23.384567395307));
#55559=CARTESIAN_POINT('Ctrl Pts',(-6.00153506451229,3.59858465928122,23.6629366710372));
#55560=CARTESIAN_POINT('Ctrl Pts',(-6.27244043602289,-3.10237419682568,
23.9413059467676));
#55561=CARTESIAN_POINT('Ctrl Pts',(-0.782248149874517,-6.95387104515194,
24.2196752224977));
#55562=CARTESIAN_POINT('Ctrl Pts',(5.42642174158814,-4.41839130940257,24.4980444982281));
#55563=CARTESIAN_POINT('Ctrl Pts',(6.651043413893,2.17528301310316,24.7764137739583));
#55564=CARTESIAN_POINT('Ctrl Pts',(1.76682897629888,6.77100805265326,25.0547830496886));
#55565=CARTESIAN_POINT('Ctrl Pts',(-4.74017875533462,5.14771211783052,25.3331523254189));
#55566=CARTESIAN_POINT('Ctrl Pts',(-6.89343725606137,-1.20364341784837,
25.6115216011491));
#55567=CARTESIAN_POINT('Ctrl Pts',(-2.71522626988215,-6.44947912500898,
25.8898908768794));
#55568=CARTESIAN_POINT('Ctrl Pts',(3.95685992531394,-5.77161105862387,26.1682601526097));
#55569=CARTESIAN_POINT('Ctrl Pts',(6.99465789092502,0.207353971519667,26.4466294283399));
#55570=CARTESIAN_POINT('Ctrl Pts',(3.60801745771017,5.99586897000287,26.7249987040702));
#55571=CARTESIAN_POINT('Ctrl Pts',(-3.09250712257939,6.27731107858934,27.0033679798005));
#55572=CARTESIAN_POINT('Ctrl Pts',(-6.95263238430926,0.79318195216411,27.2817372555308));
#55573=CARTESIAN_POINT('Ctrl Pts',(-4.42691874452137,-5.41946723488482,
27.560106531261));
#55574=CARTESIAN_POINT('Ctrl Pts',(2.16482174236717,-6.65445576319799,27.8384758069913));
#55575=CARTESIAN_POINT('Ctrl Pts',(6.76822139184016,-1.77747401433098,28.1168450827215));
#55576=CARTESIAN_POINT('Ctrl Pts',(5.15515955319559,4.73207826030814,28.3952143584518));
#55577=CARTESIAN_POINT('Ctrl Pts',(-1.19280219078862,6.89532142936314,28.6735836341821));
#55578=CARTESIAN_POINT('Ctrl Pts',(-6.44520153326523,2.72536454005337,28.9519529099124));
#55579=CARTESIAN_POINT('Ctrl Pts',(-5.77782597549934,-3.9477793349464,29.2303221856426));
#55580=CARTESIAN_POINT('Ctrl Pts',(0.19635480956596,-6.99497530155361,29.5086914613729));
#55581=CARTESIAN_POINT('Ctrl Pts',(5.99018804968463,-3.61744133470055,29.7870607371032));
#55582=CARTESIAN_POINT('Ctrl Pts',(6.28216619943336,3.08263240158176,30.0654300128334));
#55583=CARTESIAN_POINT('Ctrl Pts',(0.804113793176059,6.95137653189703,30.3437992885637));
#55584=CARTESIAN_POINT('Ctrl Pts',(-5.41249932762432,4.43543523332839,30.622168564294));
#55585=CARTESIAN_POINT('Ctrl Pts',(-6.65785165822602,-2.15435511874011,
30.9005378400242));
#55586=CARTESIAN_POINT('Ctrl Pts',(-1.78811465725532,-6.76541799544518,
31.1789071157545));
#55587=CARTESIAN_POINT('Ctrl Pts',(4.72396606441094,-5.16259424154934,31.4572763914848));
#55588=CARTESIAN_POINT('Ctrl Pts',(6.89718855280647,1.18195801432204,31.735645667215));
#55589=CARTESIAN_POINT('Ctrl Pts',(2.73549607129591,6.44090800466125,32.0140149429453));
#55590=CARTESIAN_POINT('Ctrl Pts',(-3.93868898302102,5.78402660571449,32.2923842186756));
#55591=CARTESIAN_POINT('Ctrl Pts',(-6.99527541591257,-0.185355162091369,
32.5707534944059));
#55592=CARTESIAN_POINT('Ctrl Pts',(-3.62685626695024,-5.98449231760461,
32.8491227701361));
#55593=CARTESIAN_POINT('Ctrl Pts',(3.07275005824958,-6.28700578654989,33.1274920458664));
#55594=CARTESIAN_POINT('Ctrl Pts',(6.95010349102055,-0.815043645879572,
33.4058613215966));
#55595=CARTESIAN_POINT('Ctrl Pts',(4.44394075476531,5.40551803703592,33.6842305973269));
#55596=CARTESIAN_POINT('Ctrl Pts',(-2.14388316810245,6.66123109058015,33.9625998730572));
#55597=CARTESIAN_POINT('Ctrl Pts',(-6.76259787040012,1.79875087876129,34.2409691487875));
#55598=CARTESIAN_POINT('Ctrl Pts',(-5.17001616450826,-4.71584218770179,
34.5193384245177));
#55599=CARTESIAN_POINT('Ctrl Pts',(1.17111091526254,-6.8990386217746,34.797707700248));
#55600=CARTESIAN_POINT('Ctrl Pts',(6.43659854981351,-2.74562083855788,35.0760769759783));
#55601=CARTESIAN_POINT('Ctrl Pts',(5.79021293393728,3.92958889201531,35.3544462517086));
#55602=CARTESIAN_POINT('Ctrl Pts',(-0.17435505629461,6.99555823325981,35.6328155274388));
#55603=CARTESIAN_POINT('Ctrl Pts',(-5.97878178784655,3.63626223117903,35.9111848031691));
#55604=CARTESIAN_POINT('Ctrl Pts',(-6.29182982797216,-3.06286011701881,
36.1895540788993));
#55605=CARTESIAN_POINT('Ctrl Pts',(-0.82597148324852,-6.94881326482767,
36.4679233546296));
#55606=CARTESIAN_POINT('Ctrl Pts',(5.39852338038214,-4.45243528780061,36.7462926303599));
#55607=CARTESIAN_POINT('Ctrl Pts',(6.66459405190411,2.13340591634808,37.0246619060902));
#55608=CARTESIAN_POINT('Ctrl Pts',(1.8093826525488,6.75976102367829,37.3030311818204));
#55609=CARTESIAN_POINT('Ctrl Pts',(-4.70770665026849,5.17742530372023,37.5814004575507));
#55610=CARTESIAN_POINT('Ctrl Pts',(-6.90087163169291,-1.16026092043159,
37.8597697332809));
#55611=CARTESIAN_POINT('Ctrl Pts',(-2.75573881680387,-6.43227317937797,
38.1381390090112));
#55612=CARTESIAN_POINT('Ctrl Pts',(3.92047908443075,-5.79638494487086,38.4165082847415));
#55613=CARTESIAN_POINT('Ctrl Pts',(6.99582375289604,0.163354519375268,38.6948775604718));
#55614=CARTESIAN_POINT('Ctrl Pts',(3.64565920412922,5.97305647453065,38.973246836202));
#55615=CARTESIAN_POINT('Ctrl Pts',(-3.0529626023439,6.29663831177191,39.2516161119323));
#55616=CARTESIAN_POINT('Ctrl Pts',(-6.94750585650865,0.836897278262201,
39.5299853876626));
#55617=CARTESIAN_POINT('Ctrl Pts',(-4.46091881143022,-5.39151537495839,
39.8083546633928));
#55618=CARTESIAN_POINT('Ctrl Pts',(2.12292338938355,-6.66794053388248,40.0867239391231));
#55619=CARTESIAN_POINT('Ctrl Pts',(6.75690746229423,-1.82000995232913,40.3650932148533));
#55620=CARTESIAN_POINT('Ctrl Pts',(5.18482164086506,4.69955947222737,40.6434624905837));
#55621=CARTESIAN_POINT('Ctrl Pts',(-1.14940805665755,6.90268757802897,40.9218317663139));
#55622=CARTESIAN_POINT('Ctrl Pts',(-6.42793190404972,2.76584998101567,41.2002010420442));
#55623=CARTESIAN_POINT('Ctrl Pts',(-5.80254262325399,-3.91135958279285,
41.4785703177744));
#55624=CARTESIAN_POINT('Ctrl Pts',(0.1523535785339,-6.99607197416468,41.7569395935047));
#55625=CARTESIAN_POINT('Ctrl Pts',(5.9673163918137,-3.65504716256524,42.0353088692351));
#55626=CARTESIAN_POINT('Ctrl Pts',(6.30143122605941,3.04305753869823,42.3136781449652));
#55627=CARTESIAN_POINT('Ctrl Pts',(0.847821003904525,6.94618126929632,42.5920474206956));
#55628=CARTESIAN_POINT('Ctrl Pts',(-5.38449403809326,4.46939130467704,42.8704166964258));
#55629=CARTESIAN_POINT('Ctrl Pts',(-6.67127052824044,-2.11243561312889,
43.1487859721561));
#55630=CARTESIAN_POINT('Ctrl Pts',(-1.83063275182428,-6.75403719330394,
43.4271552478863));
#55631=CARTESIAN_POINT('Ctrl Pts',(4.69140067372388,-5.19220515765391,43.7055245236166));
#55632=CARTESIAN_POINT('Ctrl Pts',(6.90448645629252,1.13855235077613,43.9838937993469));
#55633=CARTESIAN_POINT('Ctrl Pts',(2.77595430619153,6.42357473456341,44.2622630750771));
#55634=CARTESIAN_POINT('Ctrl Pts',(-3.90223040965128,5.8086859538606,44.5406323508074));
#55635=CARTESIAN_POINT('Ctrl Pts',(-6.99630289645201,-0.141352260972383,
44.8190016265377));
#55636=CARTESIAN_POINT('Ctrl Pts',(-3.66442608327355,-5.96156155388915,
45.0973709022679));
#55637=CARTESIAN_POINT('Ctrl Pts',(3.0331449505737,-6.30620855898327,45.3757401779983));
#55638=CARTESIAN_POINT('Ctrl Pts',(6.94483950646594,-0.858742633164764,
45.6541094537285));
#55639=CARTESIAN_POINT('Ctrl Pts',(4.47785274659151,5.37745938714813,45.9324787294588));
#55640=CARTESIAN_POINT('Ctrl Pts',(-2.1019426135168,6.67458402674401,46.210848005189));
#55641=CARTESIAN_POINT('Ctrl Pts',(-6.75115022380455,1.84125102476782,46.4892172809194));
#55642=CARTESIAN_POINT('Ctrl Pts',(-5.19957583582988,-4.68323027493191,
46.7675865566495));
#55643=CARTESIAN_POINT('Ctrl Pts',(1.12769382962969,-6.90626826203556,47.0459558323799));
#55644=CARTESIAN_POINT('Ctrl Pts',(6.41920168169281,-2.78605176734692,47.32432510811));
#55645=CARTESIAN_POINT('Ctrl Pts',(5.81481492150043,3.89309158757929,47.6026943838405));
#55646=CARTESIAN_POINT('Ctrl Pts',(-0.130350593893225,6.99651651918698,
47.8810636595706));
#55647=CARTESIAN_POINT('Ctrl Pts',(-5.95579197498666,3.67379594306342,48.159432935301));
#55648=CARTESIAN_POINT('Ctrl Pts',(-6.31097029873081,-3.02322486248083,
48.4378022110312));
#55649=CARTESIAN_POINT('Ctrl Pts',(-0.869662139037468,-6.94348057133521,
48.7161714867615));
#55650=CARTESIAN_POINT('Ctrl Pts',(5.37041143951732,-4.4863031162513,48.9945407624917));
#55651=CARTESIAN_POINT('Ctrl Pts',(6.6778810212001,2.09144441649309,49.2729100382221));
#55652=CARTESIAN_POINT('Ctrl Pts',(1.85186474490403,6.74824656093464,49.5512793139522));
#55653=CARTESIAN_POINT('Ctrl Pts',(-4.6750482960543,5.20693365716757,49.8296485896825));
#55654=CARTESIAN_POINT('Ctrl Pts',(-6.90803299085227,-1.11683252006797,
50.1080178654128));
#55655=CARTESIAN_POINT('Ctrl Pts',(-2.79614233951396,-6.41481275625112,
50.3863871411431));
#55656=CARTESIAN_POINT('Ctrl Pts',(3.88394313917433,-5.82092951101844,50.6647564168733));
#55657=CARTESIAN_POINT('Ctrl Pts',(6.99671284184141,0.119348604500108,50.9431256926036));
#55658=CARTESIAN_POINT('Ctrl Pts',(3.68315671876607,5.95000766937262,51.2214949683339));
#55659=CARTESIAN_POINT('Ctrl Pts',(-3.01329729894889,6.31571643352771,51.4998642440641));
#55660=CARTESIAN_POINT('Ctrl Pts',(-6.94210446726436,0.880579494522117,
51.7782335197944));
#55661=CARTESIAN_POINT('Ctrl Pts',(-4.49474239276128,-5.36335021262824,
52.0566027955247));
#55662=CARTESIAN_POINT('Ctrl Pts',(2.0809410480163,-6.68116150345623,52.334972071255));
#55663=CARTESIAN_POINT('Ctrl Pts',(6.74532621187403,-1.86247388598872,52.6133413469853));
#55664=CARTESIAN_POINT('Ctrl Pts',(5.21427860347363,4.66685475732229,52.8917106227154));
#55665=CARTESIAN_POINT('Ctrl Pts',(-1.10596844894738,6.90978063837902,53.1700798984458));
#55666=CARTESIAN_POINT('Ctrl Pts',(-6.41040796909065,2.80622599774214,53.448449174176));
#55667=CARTESIAN_POINT('Ctrl Pts',(-5.82702970729528,-3.87478508705741,
53.7268184499063));
#55668=CARTESIAN_POINT('Ctrl Pts',(0.108346319997076,-6.99689186392985,
54.0051877256365));
#55669=CARTESIAN_POINT('Ctrl Pts',(5.94420865134965,-3.69250838723553,54.2835570013669));
#55670=CARTESIAN_POINT('Ctrl Pts',(6.32044695163845,3.00336228452527,54.5619262770971));
#55671=CARTESIAN_POINT('Ctrl Pts',(0.891494672623838,6.94071119765604,54.8402955528274));
#55672=CARTESIAN_POINT('Ctrl Pts',(-5.3562757239408,4.50317055525407,55.1186648285575));
#55673=CARTESIAN_POINT('Ctrl Pts',(-6.68442546540088,-2.07043253405773,
55.397034104288));
#55674=CARTESIAN_POINT('Ctrl Pts',(-1.87307842178917,-6.7423891838437,55.6754033800181));
#55675=CARTESIAN_POINT('Ctrl Pts',(4.65864967899578,-5.22161065658646,55.9537726557485));
#55676=CARTESIAN_POINT('Ctrl Pts',(6.9115112002945,1.09510164313103,56.2321419314787));
#55677=CARTESIAN_POINT('Ctrl Pts',(2.81630271709793,6.40598733110295,56.510511207209));
#55678=CARTESIAN_POINT('Ctrl Pts',(-3.86561745387344,5.83311549524726,56.7888804829392));
#55679=CARTESIAN_POINT('Ctrl Pts',(-6.99705358500964,-0.0973437675893806,
57.0672497586697));
#55680=CARTESIAN_POINT('Ctrl Pts',(-3.70185092534808,-5.93839493525681,
57.3456190343996));
#55681=CARTESIAN_POINT('Ctrl Pts',(2.99341984377602,-6.32516184136598,57.6239883101302));
#55682=CARTESIAN_POINT('Ctrl Pts',(6.93930076595538,-0.902407646352917,
57.9023575858602));
#55683=CARTESIAN_POINT('Ctrl Pts',(4.51158758288953,5.34918799094799,58.1807268615907));
#55684=CARTESIAN_POINT('Ctrl Pts',(-2.05991890060161,6.68767289896333,58.4590961373207));
#55685=CARTESIAN_POINT('Ctrl Pts',(-6.73943548410595,1.88367832608374,58.7374654130512));
#55686=CARTESIAN_POINT('Ctrl Pts',(-5.22892979837629,-4.65043308136325,
59.0158346887813));
#55687=CARTESIAN_POINT('Ctrl Pts',(1.0842321294891,-6.91322467231963,59.2942039645118));
#55688=CARTESIAN_POINT('Ctrl Pts',(6.40155085321885,-2.82637247266478,59.5725732402418));
#55689=CARTESIAN_POINT('Ctrl Pts',(5.8391868598262,3.85644026229077,59.8509425159723));
#55690=CARTESIAN_POINT('Ctrl Pts',(-0.0863409744825115,6.99719800468092,
60.1293117917024));
#55691=CARTESIAN_POINT('Ctrl Pts',(-5.93256653546964,3.71118431000278,60.4076810674328));
#55692=CARTESIAN_POINT('Ctrl Pts',(-6.32986109105182,-2.98347000128584,
60.686050343163));
#55693=CARTESIAN_POINT('Ctrl Pts',(-0.913318388725055,-6.93787317564979,
60.9644196188933));
#55694=CARTESIAN_POINT('Ctrl Pts',(5.34208703117528,-4.5199934548551,61.2427888946235));
#55695=CARTESIAN_POINT('Ctrl Pts',(6.69090379611385,2.04940017364437,61.5211581703538));
#55696=CARTESIAN_POINT('Ctrl Pts',(1.89427357266239,6.73646511996448,61.7995274460842));
#55697=CARTESIAN_POINT('Ctrl Pts',(-4.64220498474165,5.23623601074521,62.0778967218143));
#55698=CARTESIAN_POINT('Ctrl Pts',(-6.91492105021739,-1.07335993489815,
62.3562659975447));
#55699=CARTESIAN_POINT('Ctrl Pts',(-2.83643523954384,-6.39709854640821,
62.6346352732749));
#55700=CARTESIAN_POINT('Ctrl Pts',(3.84725353500179,-5.84524378601966,62.9130045490052));
#55701=CARTESIAN_POINT('Ctrl Pts',(6.99732512258652,0.0753379678828323,
63.1913738247354));
#55702=CARTESIAN_POINT('Ctrl Pts',(3.7205085181213,5.92672346639955,63.4697431004658));
#55703=CARTESIAN_POINT('Ctrl Pts',(-2.97351278165681,6.33454468907653,63.7481123761959));
#55704=CARTESIAN_POINT('Ctrl Pts',(-6.93642843026943,0.924226872761883,
64.0264816519263));
#55705=CARTESIAN_POINT('Ctrl Pts',(-4.52838815036582,-5.33497286218137,
64.3048509276565));
#55706=CARTESIAN_POINT('Ctrl Pts',(2.03887637919601,-6.69411814886327,64.5832202033868));
#55707=CARTESIAN_POINT('Ctrl Pts',(6.7334780987638,-1.90486413532633,64.861589479117));
#55708=CARTESIAN_POINT('Ctrl Pts',(5.24352927562737,4.63396540947642,65.1399587548474));
#55709=CARTESIAN_POINT('Ctrl Pts',(-1.06248508624185,6.91660032979344,65.4183280305775));
#55710=CARTESIAN_POINT('Ctrl Pts',(-6.39263042168039,2.84649099285255,65.6966973063079));
#55711=CARTESIAN_POINT('Ctrl Pts',(-5.85128625885058,-3.83805729472223,
65.975066582038));
#55712=CARTESIAN_POINT('Ctrl Pts',(0.0643347749972447,-6.99743493841216,
66.2534358577685));
#55713=CARTESIAN_POINT('Ctrl Pts',(5.92086574249491,-3.72982352664781,66.5318051334986));
#55714=CARTESIAN_POINT('Ctrl Pts',(6.33921262385881,2.96354820951057,66.810174409229));
#55715=CARTESIAN_POINT('Ctrl Pts',(0.935133071489911,6.93496653338645,67.0885436849591));
#55716=CARTESIAN_POINT('Ctrl Pts',(-5.32784550155691,4.53677164866438,67.3669129606895));
#55717=CARTESIAN_POINT('Ctrl Pts',(-6.69731594926383,-2.02834754327791,
67.6452822364197));
#55718=CARTESIAN_POINT('Ctrl Pts',(-1.91544998788864,-6.73047442789003,
67.92365151215));
#55719=CARTESIAN_POINT('Ctrl Pts',(4.62571437594122,-5.25080957498887,68.2020207878803));
#55720=CARTESIAN_POINT('Ctrl Pts',(6.91826250689525,1.05160761040976,68.4803900636105));
#55721=CARTESIAN_POINT('Ctrl Pts',(2.85653970772702,6.38814649008333,68.7587593393409));
#55722=CARTESIAN_POINT('Ctrl Pts',(-3.8288515641914,5.85731426337825,69.0371286150711));
#55723=CARTESIAN_POINT('Ctrl Pts',(-6.99752745188624,-0.053331423033017,
69.3154978908014));
#55724=CARTESIAN_POINT('Ctrl Pts',(-3.73912931254947,-5.91499337823953,
69.5938671665316));
#55725=CARTESIAN_POINT('Ctrl Pts',(2.95357630948563,-6.34386488385672,69.8722364422619));
#55726=CARTESIAN_POINT('Ctrl Pts',(6.9334874886159,-0.946036957941923,70.1506057179922));
#55727=CARTESIAN_POINT('Ctrl Pts',(4.54514392902107,5.32070496692563,70.4289749937224));
#55728=CARTESIAN_POINT('Ctrl Pts',(-2.01781369192432,6.70049718940818,70.7073442694526));
#55729=CARTESIAN_POINT('Ctrl Pts',(-6.72745411477015,1.92603110417443,70.985713545183));
#55730=CARTESIAN_POINT('Ctrl Pts',(-5.25807689082814,-4.61745190453829,
71.2640828209132));
#55731=CARTESIAN_POINT('Ctrl Pts',(1.04072753429877,-6.91990757741292,71.5424520966435));
#55732=CARTESIAN_POINT('Ctrl Pts',(6.38364676270434,-2.86658135931959,71.8208213723738));
#55733=CARTESIAN_POINT('Ctrl Pts',(5.86332778469723,3.81963636617187,72.099190648104));
#55734=CARTESIAN_POINT('Ctrl Pts',(-0.0423279391977326,6.9976026627802,
72.3775599238344));
#55735=CARTESIAN_POINT('Ctrl Pts',(-5.90910638815427,3.74842585281589,72.6559291995646));
#55736=CARTESIAN_POINT('Ctrl Pts',(-6.34850145756637,-2.94359710623954,
72.9342984752948));
#55737=CARTESIAN_POINT('Ctrl Pts',(-0.956938505156228,-6.93199129961475,
73.2126677510252));
#55738=CARTESIAN_POINT('Ctrl Pts',(5.31355127594381,-4.5535049707342,73.4910370267554));
#55739=CARTESIAN_POINT('Ctrl Pts',(6.70366186143025,2.00727485118249,73.7694063024857));
#55740=CARTESIAN_POINT('Ctrl Pts',(1.93660745801957,6.72441716687232,74.0477755782159));
#55741=CARTESIAN_POINT('Ctrl Pts',(-4.6091780156978,5.26533120517534,74.3261448539462));
#55742=CARTESIAN_POINT('Ctrl Pts',(-6.9215355372788,-1.0298448848113,74.6045141296765));
#55743=CARTESIAN_POINT('Ctrl Pts',(-2.87661592280069,-6.37913125066994,
74.8828834054067));
#55744=CARTESIAN_POINT('Ctrl Pts',(3.81041172344989,-5.86932680793801,75.1612526811371));
#55745=CARTESIAN_POINT('Ctrl Pts',(6.99766057090778,0.0313243506992304,
75.4396219568672));
#55746=CARTESIAN_POINT('Ctrl Pts',(3.75771312446028,5.9032047867954,75.7179912325976));
#55747=CARTESIAN_POINT('Ctrl Pts',(-2.93361062444756,6.35312233352339,75.9963605083277));
#55748=CARTESIAN_POINT('Ctrl Pts',(-6.93047797008259,0.967837686176782,
76.2747297840582));
#55749=CARTESIAN_POINT('Ctrl Pts',(-4.56185475312959,-5.30638444629986,
76.5530990597882));
#55750=CARTESIAN_POINT('Ctrl Pts',(1.99673104711092,-6.70680995750503,76.8314683355187));
#55751=CARTESIAN_POINT('Ctrl Pts',(6.72136359170614,-1.94717902327247,77.1098376112488));
#55752=CARTESIAN_POINT('Ctrl Pts',(5.2725725000929,4.60089272987844,77.3882068869792));
#55753=CARTESIAN_POINT('Ctrl Pts',(-1.01895968885651,6.92314638246727,77.6665761627094));
#55754=CARTESIAN_POINT('Ctrl Pts',(-6.3745999651453,2.88664337335853,77.9449454384397));
#55755=CARTESIAN_POINT('Ctrl Pts',(-5.87531131826721,-3.80117765883502,
78.22331471417));
#55756=CARTESIAN_POINT('Ctrl Pts',(0.0203206847462305,-6.99770117612603,
78.5016839899002));
#55757=CARTESIAN_POINT('Ctrl Pts',(5.89728858875571,-3.76699110451776,78.7800532656305));
#55758=CARTESIAN_POINT('Ctrl Pts',(6.35772750030168,2.92361688880281,79.0584225413607));
#55759=CARTESIAN_POINT('Ctrl Pts',(0.978734474053595,6.9289475037616,79.3367918170911));
#55760=CARTESIAN_POINT('Ctrl Pts',(-5.29920449571548,4.57019325556077,79.6151610928212));
#55761=CARTESIAN_POINT('Ctrl Pts',(-6.70994146984795,-1.98618230578136,
79.8935303685517));
#55762=CARTESIAN_POINT('Ctrl Pts',(-1.95774577379312,-6.71829339682188,
80.1718996442817));
#55763=CARTESIAN_POINT('Ctrl Pts',(4.59259606756707,-5.27980075767568,80.4502689200122));
#55764=CARTESIAN_POINT('Ctrl Pts',(6.9247401089954,1.00807197335037,80.7286381957424));
#55765=CARTESIAN_POINT('Ctrl Pts',(2.89666368619801,6.37005291733483,81.0070074714725));
#55766=CARTESIAN_POINT('Ctrl Pts',(-3.79193419515991,5.88128130088692,81.2853767472031));
#55767=CARTESIAN_POINT('Ctrl Pts',(-6.99772447833453,-0.00931696854672991,
81.563746022933));
#55768=CARTESIAN_POINT('Ctrl Pts',(-3.7762597700471,-5.89135780866416,81.8421152986636));
#55769=CARTESIAN_POINT('Ctrl Pts',(2.91361592401662,-6.36231694651414,82.1204845743937));
#55770=CARTESIAN_POINT('Ctrl Pts',(6.92739990443582,-0.989628841842616,
82.3988538501239));
#55771=CARTESIAN_POINT('Ctrl Pts',(4.57852045740981,5.2920114419439,82.6772231258543));
#55772=CARTESIAN_POINT('Ctrl Pts',(-1.9756286532773,6.71305639071614,82.9555924015846));
#55773=CARTESIAN_POINT('Ctrl Pts',(-6.71520658981113,1.96830768345331,83.2339616773148));
#55774=CARTESIAN_POINT('Ctrl Pts',(-5.28701596005046,-4.58428804927831,
83.5123309530451));
#55775=CARTESIAN_POINT('Ctrl Pts',(0.997181765214038,-6.92631671292251,
83.7907002287754));
#55776=CARTESIAN_POINT('Ctrl Pts',(6.36549011848205,-2.90667683654248,84.0690695045055));
#55777=CARTESIAN_POINT('Ctrl Pts',(5.88723674103532,3.78268135528068,84.347438780236));
#55778=CARTESIAN_POINT('Ctrl Pts',(0.00168677069072056,6.99773047747545,
84.6258080559661));
#55779=CARTESIAN_POINT('Ctrl Pts',(-5.88541246118538,3.78551909813028,84.9041773316965));
#55780=CARTESIAN_POINT('Ctrl Pts',(-6.36689066081281,-2.9036077548181,85.1825466074266));
#55781=CARTESIAN_POINT('Ctrl Pts',(-1.00052076260523,-6.92583517593222,
85.4609158831571));
#55782=CARTESIAN_POINT('Ctrl Pts',(5.28480530277132,-4.5868363380858,85.7392851588871));
#55783=CARTESIAN_POINT('Ctrl Pts',(6.71615471240727,1.96507011569431,86.0176544346176));
#55784=CARTESIAN_POINT('Ctrl Pts',(1.97886472613705,6.71210317830676,86.2960237103478));
#55785=CARTESIAN_POINT('Ctrl Pts',(-4.57596869555562,5.29421808937629,86.574392986078));
#55786=CARTESIAN_POINT('Ctrl Pts',(-6.92787619034991,-0.98628909137584,
86.8527622618084));
#55787=CARTESIAN_POINT('Ctrl Pts',(-2.91668279963266,-6.36091157986905,
87.1311315375386));
#55788=CARTESIAN_POINT('Ctrl Pts',(3.77341916207662,-5.89317762398675,87.4095008132688));
#55789=CARTESIAN_POINT('Ctrl Pts',(6.99771917353418,-0.0126905057570474,
87.6878700889991));
#55790=CARTESIAN_POINT('Ctrl Pts',(3.79476906587156,5.87945256102033,87.9662393647294));
#55791=CARTESIAN_POINT('Ctrl Pts',(-2.89359240595405,6.37144863188822,88.2446086404596));
#55792=CARTESIAN_POINT('Ctrl Pts',(-6.92425332211979,1.01141020940972,88.52297791619));
#55793=CARTESIAN_POINT('Ctrl Pts',(-4.59514087702648,-5.27758609601629,
88.8013471919202));
#55794=CARTESIAN_POINT('Ctrl Pts',(1.9545067191403,-6.71923642726015,89.0797164676505));
#55795=CARTESIAN_POINT('Ctrl Pts',(6.70898316998215,-1.98941687574033,89.3580857433807));
#55796=CARTESIAN_POINT('Ctrl Pts',(5.30140712784506,4.5676380269696,89.636455019111));
#55797=CARTESIAN_POINT('Ctrl Pts',(-0.975393978769655,6.92941853742182,
89.9148242948413));
#55798=CARTESIAN_POINT('Ctrl Pts',(-6.35631731281709,2.92668155072702,90.1931935705715));
#55799=CARTESIAN_POINT('Ctrl Pts',(-5.89910393505123,-3.76414763844981,
90.4715628463019));
#55800=CARTESIAN_POINT('Ctrl Pts',(-0.0236942094442284,-6.99769056653865,
90.749932122032));
#55801=CARTESIAN_POINT('Ctrl Pts',(5.87347812290604,-3.80400965039908,91.0283013977623));
#55802=CARTESIAN_POINT('Ctrl Pts',(6.37599084846996,2.88356990218922,91.3066706734926));
#55803=CARTESIAN_POINT('Ctrl Pts',(1.0222971553301,6.92265434690973,91.5850399492228));
#55804=CARTESIAN_POINT('Ctrl Pts',(-5.27035383952926,4.60343405369778,91.8634092249532));
#55805=CARTESIAN_POINT('Ctrl Pts',(-6.72230152765492,-1.94393848973506,
92.1417785006834));
#55806=CARTESIAN_POINT('Ctrl Pts',(-1.99996410617077,-6.7058465725524,92.4201477764137));
#55807=CARTESIAN_POINT('Ctrl Pts',(4.55929606411945,-5.30858305768019,92.6985170521439));
#55808=CARTESIAN_POINT('Ctrl Pts',(6.93094375032431,0.964496454335416,92.9768863278743));
#55809=CARTESIAN_POINT('Ctrl Pts',(2.93667306510209,6.35170732868644,93.2552556036044));
#55810=CARTESIAN_POINT('Ctrl Pts',(-3.75486680732616,5.90501565957488,93.5336248793348));
#55811=CARTESIAN_POINT('Ctrl Pts',(-6.9976446565594,0.0346978545432685,
93.811994155065));
#55812=CARTESIAN_POINT('Ctrl Pts',(-3.81324082886386,-5.86748916161511,
94.0903634307953));
#55813=CARTESIAN_POINT('Ctrl Pts',(2.87354026830597,-6.38051729932687,94.3687327065256));
#55814=CARTESIAN_POINT('Ctrl Pts',(6.92103825425605,-1.03318157344609,94.6471019822558));
#55815=CARTESIAN_POINT('Ctrl Pts',(4.61171584759291,5.26310855119335,94.9254712579861));
#55816=CARTESIAN_POINT('Ctrl Pts',(-1.93336545361025,6.72535000601245,95.2038405337164));
#55817=CARTESIAN_POINT('Ctrl Pts',(-6.70269339377315,2.01050639134894,95.4822098094466));
#55818=CARTESIAN_POINT('Ctrl Pts',(-5.31574586113814,-4.5509428276322,95.760579085177));
#55819=CARTESIAN_POINT('Ctrl Pts',(0.953596545019199,-6.93245182528603,
96.038948360907));
#55820=CARTESIAN_POINT('Ctrl Pts',(6.34708163887577,-2.94665731805215,96.3173176366376));
#55821=CARTESIAN_POINT('Ctrl Pts',(5.91091278294024,3.74557669165362,96.5956869123676));
#55822=CARTESIAN_POINT('Ctrl Pts',(0.0457014138459489,6.99758144371023,
96.8740561880982));
#55823=CARTESIAN_POINT('Ctrl Pts',(-5.86148569195634,3.82246257844015,97.152425463828));
#55824=CARTESIAN_POINT('Ctrl Pts',(-6.38502797326628,-2.86350352910403,
97.4307947395587));
#55825=CARTESIAN_POINT('Ctrl Pts',(-1.04406343684472,-6.91940504815473,
97.7091640152887));
#55826=CARTESIAN_POINT('Ctrl Pts',(5.2558502489239,-4.61998623823404,97.9875332910192));
#55827=CARTESIAN_POINT('Ctrl Pts',(6.72838185479479,1.9227876369096,98.2659025667492));
#55828=CARTESIAN_POINT('Ctrl Pts',(2.02104370520724,6.69952364144096,98.5442718424796));
#55829=CARTESIAN_POINT('Ctrl Pts',(-4.54257833816235,5.32289552050794,98.8226411182098));
#55830=CARTESIAN_POINT('Ctrl Pts',(-6.93394275857822,-0.942694277772887,
99.1010103939402));
#55831=CARTESIAN_POINT('Ctrl Pts',(-2.95663428488913,-6.34244025482325,
99.3793796696704));
#55832=CARTESIAN_POINT('Ctrl Pts',(3.73627731440385,-5.91679529056526,99.6577489454006));
#55833=CARTESIAN_POINT('Ctrl Pts',(6.99750092814722,-0.0567048601441356,
99.9361182211311));
#55834=CARTESIAN_POINT('Ctrl Pts',(3.83167487632577,5.85546772877446,100.214487496861));
#55835=CARTESIAN_POINT('Ctrl Pts',(-2.85345970940146,6.38952285913484,100.492856772592));
#55836=CARTESIAN_POINT('Ctrl Pts',(-6.91775473264401,1.0549427186182,100.771226048322));
#55837=CARTESIAN_POINT('Ctrl Pts',(-4.62824520517111,-5.24857895066806,
101.049595324052));
#55838=CARTESIAN_POINT('Ctrl Pts',(1.91220506578854,-6.73139706650542,101.327964599782));
#55839=CARTESIAN_POINT('Ctrl Pts',(6.69633732339394,-2.03157602168996,101.606333875513));
#55840=CARTESIAN_POINT('Ctrl Pts',(5.33003201811036,4.53420261639271,101.884703151243));
#55841=CARTESIAN_POINT('Ctrl Pts',(-0.931789679554102,6.93541654651411,
102.163072426973));
#55842=CARTESIAN_POINT('Ctrl Pts',(-6.33778318800533,2.96660394094364,102.441441702703));
#55843=CARTESIAN_POINT('Ctrl Pts',(-5.92266316790465,-3.72696869857125,
102.719810978434));
#55844=CARTESIAN_POINT('Ctrl Pts',(-0.0677081662298231,-6.99740311006948,
102.998180254164));
#55845=CARTESIAN_POINT('Ctrl Pts',(5.84943528694958,-3.84087769974172,103.276549529894));
#55846=CARTESIAN_POINT('Ctrl Pts',(6.39400194581841,2.84340883403278,103.554918805624));
#55847=CARTESIAN_POINT('Ctrl Pts',(1.06581939186588,6.91608731180484,103.833288081355));
#55848=CARTESIAN_POINT('Ctrl Pts',(-5.24129467440546,4.63649272798234,104.111657357085));
#55849=CARTESIAN_POINT('Ctrl Pts',(-6.73439563368848,-1.90161776641409,
104.390026632815));
#55850=CARTESIAN_POINT('Ctrl Pts',(-2.04210331475472,-6.6931344475106,104.668395908546));
#55851=CARTESIAN_POINT('Ctrl Pts',(4.52581568303376,-5.33715533629955,104.946765184276));
#55852=CARTESIAN_POINT('Ctrl Pts',(6.93687318544946,0.920882777326449,105.225134460006));
#55853=CARTESIAN_POINT('Ctrl Pts',(2.97656626156395,6.33311044993717,105.503503735736));
#55854=CARTESIAN_POINT('Ctrl Pts',(-3.71765086717258,5.92851640044929,105.781873011467));
#55855=CARTESIAN_POINT('Ctrl Pts',(-6.99728798971909,0.0787113048955276,
106.060242287197));
#55856=CARTESIAN_POINT('Ctrl Pts',(-3.85007102593217,-5.84338838139839,
106.338611562927));
#55857=CARTESIAN_POINT('Ctrl Pts',(2.83335092785082,-6.39846522224127,106.616980838657));
#55858=CARTESIAN_POINT('Ctrl Pts',(6.91440278975997,-1.07669342969335,106.895350114388));
#55859=CARTESIAN_POINT('Ctrl Pts',(4.64472878627452,5.23399743814782,107.173719390118));
#55860=CARTESIAN_POINT('Ctrl Pts',(-1.89102576496565,6.73737754892958,107.452088665848));
#55861=CARTESIAN_POINT('Ctrl Pts',(-6.68991502171053,2.0526255583705,107.730457941578));
#55862=CARTESIAN_POINT('Ctrl Pts',(-5.34426545746175,-4.51741755882344,
108.008827217309));
#55863=CARTESIAN_POINT('Ctrl Pts',(0.909973598059053,-6.93831267178273,
108.287196493039));
#55864=CARTESIAN_POINT('Ctrl Pts',(6.32842205217333,-2.98652122211621,108.565565768769));
#55865=CARTESIAN_POINT('Ctrl Pts',(5.93435497372563,3.70832384324806,108.843935044499));
#55866=CARTESIAN_POINT('Ctrl Pts',(0.0897142489341528,6.99715556738046,
109.12230432023));
#55867=CARTESIAN_POINT('Ctrl Pts',(-5.83732702707266,3.85925483216542,109.40067359596));
#55868=CARTESIAN_POINT('Ctrl Pts',(-6.40291267736745,-2.82328601572554,
109.679042871691));
#55869=CARTESIAN_POINT('Ctrl Pts',(-1.0875648052126,-6.91270117067468,109.95741214742));
#55870=CARTESIAN_POINT('Ctrl Pts',(5.22668725993863,-4.65295335968247,110.235781423151));
#55871=CARTESIAN_POINT('Ctrl Pts',(6.74034280485554,1.88042908763332,110.514150698881));
#55872=CARTESIAN_POINT('Ctrl Pts',(2.06314272651936,6.68667905395455,110.792519974612));
#55873=CARTESIAN_POINT('Ctrl Pts',(-4.50900826452764,5.35136236401588,111.070889250342));
#55874=CARTESIAN_POINT('Ctrl Pts',(-6.93973500195425,-0.899062168726521,
111.349258526072));
#55875=CARTESIAN_POINT('Ctrl Pts',(-2.99646879798562,-6.3237180063064,111.627627801802));
#55876=CARTESIAN_POINT('Ctrl Pts',(3.69898764986036,-5.94017887329715,111.905997077532));
#55877=CARTESIAN_POINT('Ctrl Pts',(6.99700584338106,-0.100716971138942,
112.184366353263));
#55878=CARTESIAN_POINT('Ctrl Pts',(3.86842909573286,5.83125123895993,112.462735628993));
#55879=CARTESIAN_POINT('Ctrl Pts',(-2.81321412254376,6.40734430020001,112.741104904723));
#55880=CARTESIAN_POINT('Ctrl Pts',(-6.91098245875672,1.09843349154236,113.019474180454));
#55881=CARTESIAN_POINT('Ctrl Pts',(-4.66116642786946,-5.21936415785361,
113.297843456184));
#55882=CARTESIAN_POINT('Ctrl Pts',(1.86982776061911,-6.74329139413405,113.576212731914));
#55883=CARTESIAN_POINT('Ctrl Pts',(6.68342655224396,-2.0736547931962,113.854582007644));
#55884=CARTESIAN_POINT('Ctrl Pts',(5.35844603841386,4.50058782093984,114.132951283375));
#55885=CARTESIAN_POINT('Ctrl Pts',(-0.888148516309729,6.94114017244725,
114.411320559105));
#55886=CARTESIAN_POINT('Ctrl Pts',(-6.31899832396796,3.00640896457457,114.689689834835));
#55887=CARTESIAN_POINT('Ctrl Pts',(-5.9459880847631,-3.68964231009464,114.968059110565));
#55888=CARTESIAN_POINT('Ctrl Pts',(-0.111719444303851,-6.99683881809132,
115.246428386296));
#55889=CARTESIAN_POINT('Ctrl Pts',(5.82516103208404,-3.87759379394926,115.524797662026));
#55890=CARTESIAN_POINT('Ctrl Pts',(6.41176007978063,2.80313527321026,115.803166937756));
#55891=CARTESIAN_POINT('Ctrl Pts',(1.109299461808,6.90924665825571,116.081536213487));
#55892=CARTESIAN_POINT('Ctrl Pts',(-5.2120281500005,4.66936797052745,116.359905489217));
#55893=CARTESIAN_POINT('Ctrl Pts',(-6.74622330947431,-1.85922181013711,
116.638274764947));
#55894=CARTESIAN_POINT('Ctrl Pts',(-2.08416173240764,-6.6801575246211,116.916644040677));
#55895=CARTESIAN_POINT('Ctrl Pts',(4.49215624888088,-5.36551646313994,117.195013316408));
#55896=CARTESIAN_POINT('Ctrl Pts',(6.94252817978723,0.877232667794093,117.473382592138));
#55897=CARTESIAN_POINT('Ctrl Pts',(3.01634169730445,6.31426301682841,117.751751867868));
#55898=CARTESIAN_POINT('Ctrl Pts',(-3.68028784705895,5.95178259375914,118.030121143598));
#55899=CARTESIAN_POINT('Ctrl Pts',(-6.99665449192391,0.122721641223584,
118.308490419329));
#55900=CARTESIAN_POINT('Ctrl Pts',(-3.88674890415396,-5.81905642150383,
118.586859695059));
#55901=CARTESIAN_POINT('Ctrl Pts',(2.79304949264689,-6.41616000519071,118.865228970789));
#55902=CARTESIAN_POINT('Ctrl Pts',(6.90749377346335,-1.12016268914174,119.143598246519));
#55903=CARTESIAN_POINT('Ctrl Pts',(4.67755796737731,5.20467925451912,119.42196752225));
#55904=CARTESIAN_POINT('Ctrl Pts',(-1.84861126241298,6.74913854362568,119.70033679798));
#55905=CARTESIAN_POINT('Ctrl Pts',(-6.67687197916712,2.0946635181759,119.97870607371));
#55906=CARTESIAN_POINT('Ctrl Pts',(-5.37257362071552,-4.48371356920345,
120.257075349441));
#55907=CARTESIAN_POINT('Ctrl Pts',(0.86631465017897,-6.94389902053411,120.535444625171));
#55908=CARTESIAN_POINT('Ctrl Pts',(6.30951209658112,-3.02626697163003,120.813813900901));
#55909=CARTESIAN_POINT('Ctrl Pts',(5.95756238598644,3.67092428391178,121.092183176631));
#55910=CARTESIAN_POINT('Ctrl Pts',(0.133723534638353,6.99645286528214,121.370552452362));
#55911=CARTESIAN_POINT('Ctrl Pts',(-5.81293742221111,3.8958944038083,121.648921728092));
#55912=CARTESIAN_POINT('Ctrl Pts',(-6.42054406574492,-2.78295680598006,
121.927291003822));
#55913=CARTESIAN_POINT('Ctrl Pts',(-1.13102314631542,-6.90572380835968,
122.205660279552));
#55914=CARTESIAN_POINT('Ctrl Pts',(5.19731748888817,-4.68573639883701,122.484029555283));
#55915=CARTESIAN_POINT('Ctrl Pts',(6.75203709068823,1.83799614494737,122.762398831013));
#55916=CARTESIAN_POINT('Ctrl Pts',(2.10516012206219,6.67356992161945,123.040768106744));
#55917=CARTESIAN_POINT('Ctrl Pts',(-4.47525979811722,5.37961749819687,123.319137382473));
#55918=CARTESIAN_POINT('Ctrl Pts',(-6.94525270010952,-0.855394498969912,
123.597506658204));
#55919=CARTESIAN_POINT('Ctrl Pts',(-3.03618474637166,-6.30474555890793,
123.875875933934));
#55920=CARTESIAN_POINT('Ctrl Pts',(3.66155161239148,-5.96332747748852,124.154245209664));
#55921=CARTESIAN_POINT('Ctrl Pts',(6.99623399798153,-0.1447250400655,124.432614485395));
#55922=CARTESIAN_POINT('Ctrl Pts',(3.90503015829615,5.80680394118188,124.710983761125));
#55923=CARTESIAN_POINT('Ctrl Pts',(-2.77285702668229,6.42491245482045,124.989353036855));
#55924=CARTESIAN_POINT('Ctrl Pts',(-6.90393716664472,1.14188042087048,125.267722312585));
#55925=CARTESIAN_POINT('Ctrl Pts',(-4.69390249067992,-5.18994214321111,
125.546091588316));
#55926=CARTESIAN_POINT('Ctrl Pts',(1.82737506027401,-6.75492031829483,125.824460864046));
#55927=CARTESIAN_POINT('Ctrl Pts',(6.67025404840435,-2.11564892221031,126.102830139776));
#55928=CARTESIAN_POINT('Ctrl Pts',(5.38664300218255,4.46679005493539,126.381199415506));
#55929=CARTESIAN_POINT('Ctrl Pts',(-0.844462656677822,6.94659847036505,
126.659568691237));
#55930=CARTESIAN_POINT('Ctrl Pts',(-6.29998151306312,3.04607752130724,126.937937966967));
#55931=CARTESIAN_POINT('Ctrl Pts',(-5.96904368230331,-3.65213685798737,
127.216307242697));
#55932=CARTESIAN_POINT('Ctrl Pts',(-0.155790653488725,-6.99606019700873,
127.494676518427));
#55933=CARTESIAN_POINT('Ctrl Pts',(5.80077782692774,-3.9140384969439,127.773045794158));
#55934=CARTESIAN_POINT('Ctrl Pts',(6.42903511182726,2.76252802932186,128.051415069888));
#55935=CARTESIAN_POINT('Ctrl Pts',(1.15316889662473,6.90255337426073,128.329784345618));
#55936=CARTESIAN_POINT('Ctrl Pts',(-5.18337373568856,4.70126361979388,128.608153621349));
#55937=CARTESIAN_POINT('Ctrl Pts',(-6.75623695130492,-1.81524767029855,
128.886522897079));
#55938=CARTESIAN_POINT('Ctrl Pts',(-2.12907532833933,-6.66978817737252,
129.164892172809));
#55939=CARTESIAN_POINT('Ctrl Pts',(4.46399912483758,-5.3879904519143,129.44326144854));
#55940=CARTESIAN_POINT('Ctrl Pts',(6.52410345000868,-0.214043852273786,
129.675235844981));
#55941=CARTESIAN_POINT('Ctrl Pts',(5.0100391049337,3.57981706251019,129.860815362135));
#55942=CARTESIAN_POINT('Ctrl Pts',(3.47055515188223,4.89229596196689,129.953605120712));
#55943=CARTESIAN_POINT('Ctrl Pts',(2.58391981634458,5.32271443393329,130.));
#55944=CARTESIAN_POINT('Ctrl Pts',(3.24375760296843,-4.54512507566758,-10.3843228291906));
#55945=CARTESIAN_POINT('Ctrl Pts',(4.00086538069068,-4.00479360637521,-10.3379279499022));
#55946=CARTESIAN_POINT('Ctrl Pts',(5.2263164302552,-2.54076122583732,-10.2451381913254));
#55947=CARTESIAN_POINT('Ctrl Pts',(6.03675826576676,1.22812655469745,-10.0595586741719));
#55948=CARTESIAN_POINT('Ctrl Pts',(3.3038612674489,5.71744161547796,-9.82758427773004));
#55949=CARTESIAN_POINT('Ctrl Pts',(-3.03299291957947,5.87028068222262,-9.54921500199974));
#55950=CARTESIAN_POINT('Ctrl Pts',(-6.57280714142195,0.623467478762871,
-9.27084572626949));
#55951=CARTESIAN_POINT('Ctrl Pts',(-4.08153023623295,-5.19191713446524,
-8.99247645053922));
#55952=CARTESIAN_POINT('Ctrl Pts',(2.1616472547184,-6.24078027128343,-8.71410717480895));
#55953=CARTESIAN_POINT('Ctrl Pts',(6.41775644389384,-1.55649378700411,-8.43573789907868));
#55954=CARTESIAN_POINT('Ctrl Pts',(4.78016848203232,4.5567989667075,-8.1573686233484));
#55955=CARTESIAN_POINT('Ctrl Pts',(-1.24835914482659,6.48508986838572,-7.87899934761815));
#55956=CARTESIAN_POINT('Ctrl Pts',(-6.13005252277504,2.45680138155627,-7.60063007188787));
#55957=CARTESIAN_POINT('Ctrl Pts',(-5.38155761977461,-3.82791583738751,
-7.3222607961576));
#55958=CARTESIAN_POINT('Ctrl Pts',(0.309847241136156,-6.59682421882921,
-7.04389152042733));
#55959=CARTESIAN_POINT('Ctrl Pts',(5.71662802486233,-3.30667067493405,-6.76552224469707));
#55960=CARTESIAN_POINT('Ctrl Pts',(5.87283174034777,3.02057345711623,-6.48715296896679));
#55961=CARTESIAN_POINT('Ctrl Pts',(0.634959370610084,6.57349474634657,-6.20878369323653));
#55962=CARTESIAN_POINT('Ctrl Pts',(-5.1861037376981,4.08880295424966,-5.93041441750626));
#55963=CARTESIAN_POINT('Ctrl Pts',(-6.24384824386448,-2.15136185560887,
-5.65204514177599));
#55964=CARTESIAN_POINT('Ctrl Pts',(-1.56675487761984,-6.41554947533565,
-5.37367586604572));
#55965=CARTESIAN_POINT('Ctrl Pts',(4.54936735322769,-4.78719640305079,-5.09530659031545));
#55966=CARTESIAN_POINT('Ctrl Pts',(6.48699682467727,1.23809027700563,-4.81693731458518));
#55967=CARTESIAN_POINT('Ctrl Pts',(2.4664631218177,6.12621860550624,-4.53856803885491));
#55968=CARTESIAN_POINT('Ctrl Pts',(-3.81946222780992,5.38755070830706,-4.26019876312464));
#55969=CARTESIAN_POINT('Ctrl Pts',(-6.59729615370307,-0.299463181352188,
-3.98182948739437));
#55970=CARTESIAN_POINT('Ctrl Pts',(-3.31565960480102,-5.71142679251214,
-3.70346021166411));
#55971=CARTESIAN_POINT('Ctrl Pts',(3.01133685894659,-5.87757134360681,-3.42509093593384));
#55972=CARTESIAN_POINT('Ctrl Pts',(6.57248710337548,-0.645296761764896,
-3.14672166020357));
#55973=CARTESIAN_POINT('Ctrl Pts',(4.09695346479151,5.17966861116296,-2.8683523844733));
#55974=CARTESIAN_POINT('Ctrl Pts',(-2.14154121484956,6.24722304987754,-2.58998310874303));
#55975=CARTESIAN_POINT('Ctrl Pts',(-6.41307770751666,1.57684144270601,-2.31161383301276));
#55976=CARTESIAN_POINT('Ctrl Pts',(-4.7943443218783,-4.54183411606296,-2.03324455728249));
#55977=CARTESIAN_POINT('Ctrl Pts',(1.2278881678272,-6.48893560313017,-1.75487528155222));
#55978=CARTESIAN_POINT('Ctrl Pts',(6.12233256318639,-2.47609341527485,-1.47650600582196));
#55979=CARTESIAN_POINT('Ctrl Pts',(5.39355005832625,3.8109857495363,-1.19813673009168));
#55980=CARTESIAN_POINT('Ctrl Pts',(-0.289088752394491,6.59775888526443,
-0.919767454361418));
#55981=CARTESIAN_POINT('Ctrl Pts',(-5.70620594500332,3.32463657084714,-0.641398178631146));
#55982=CARTESIAN_POINT('Ctrl Pts',(-5.88229932251409,-3.00209082062202,
-0.36302890290088));
#55983=CARTESIAN_POINT('Ctrl Pts',(-0.655631016724059,-6.57146426489795,
-0.0846596271706075));
#55984=CARTESIAN_POINT('Ctrl Pts',(5.17321986111141,-4.10509328560812,0.193709648559658));
#55985=CARTESIAN_POINT('Ctrl Pts',(6.25058284067101,2.13171498255206,0.472078924289931));
#55986=CARTESIAN_POINT('Ctrl Pts',(1.58692387993814,6.41059023914432,0.750448200020196));
#55987=CARTESIAN_POINT('Ctrl Pts',(-4.53428952724171,4.80148030278988,1.02881747575047));
#55988=CARTESIAN_POINT('Ctrl Pts',(-6.49085840076931,-1.21768297848549,
1.30718675148073));
#55989=CARTESIAN_POINT('Ctrl Pts',(-2.48571755217521,-6.11843140565777,
1.58555602721101));
#55990=CARTESIAN_POINT('Ctrl Pts',(3.80249982994736,-5.39953605953158,1.86392530294127));
#55991=CARTESIAN_POINT('Ctrl Pts',(6.59820531227598,0.278713602079585,2.14229457867155));
#55992=CARTESIAN_POINT('Ctrl Pts',(3.33360531111273,5.70097099138844,2.42066385440181));
#55993=CARTESIAN_POINT('Ctrl Pts',(-2.99283735644156,5.88701275459968,2.69903313013208));
#55994=CARTESIAN_POINT('Ctrl Pts',(-6.57042517877034,0.665963651494575,
2.97740240586235));
#55995=CARTESIAN_POINT('Ctrl Pts',(-4.11322295513127,-5.1667583199055,3.25577168159262));
#55996=CARTESIAN_POINT('Ctrl Pts',(2.1218834788284,-6.25392717555989,3.53414095732289));
#55997=CARTESIAN_POINT('Ctrl Pts',(6.40808691970446,-1.59700239337454,3.81251023305315));
#55998=CARTESIAN_POINT('Ctrl Pts',(4.80860441111101,4.52673372669247,4.09087950878343));
#55999=CARTESIAN_POINT('Ctrl Pts',(-1.20747477815584,6.49276514861342,4.36924878451369));
#56000=CARTESIAN_POINT('Ctrl Pts',(-6.11451511929506,2.49533554273639,4.64761806024396));
#56001=CARTESIAN_POINT('Ctrl Pts',(-5.40550870944644,-3.7940045080403,4.92598733597424));
#56002=CARTESIAN_POINT('Ctrl Pts',(0.268337762589008,-6.59863542409339,
5.20435661170449));
#56003=CARTESIAN_POINT('Ctrl Pts',(5.69572194115494,-3.34256580847368,5.48272588743478));
#56004=CARTESIAN_POINT('Ctrl Pts',(5.89171163003959,2.9835764919619,5.76109516316503));
#56005=CARTESIAN_POINT('Ctrl Pts',(0.676294639557663,6.56936984614483,6.03946443889531));
#56006=CARTESIAN_POINT('Ctrl Pts',(-5.16028400300898,4.12134245400949,6.31783371462558));
#56007=CARTESIAN_POINT('Ctrl Pts',(-6.25725604654667,-2.11204672838612,
6.59620299035585));
#56008=CARTESIAN_POINT('Ctrl Pts',(-1.60707695795029,-6.40556775517648,
6.87457226608611));
#56009=CARTESIAN_POINT('Ctrl Pts',(4.51916673302206,-4.81571662933754,7.15294154181639));
#56010=CARTESIAN_POINT('Ctrl Pts',(6.4946558419881,1.19726359213888,7.43131081754665));
#56011=CARTESIAN_POINT('Ctrl Pts',(2.50494736315481,6.11058371375067,7.70968009327693));
#56012=CARTESIAN_POINT('Ctrl Pts',(-3.78549980480989,5.41146799331898,7.98804936900718));
#56013=CARTESIAN_POINT('Ctrl Pts',(-6.5990492196591,-0.25796125958747,8.26641864473747));
#56014=CARTESIAN_POINT('Ctrl Pts',(-3.35151804077057,-5.69045880727739,
8.54478792046771));
#56015=CARTESIAN_POINT('Ctrl Pts',(2.97430825008044,-5.89639593721748,8.82315719619802));
#56016=CARTESIAN_POINT('Ctrl Pts',(6.56829826963177,-0.686623955366883,
9.10152647192824));
#56017=CARTESIAN_POINT('Ctrl Pts',(4.12945176216551,5.15379692643003,9.37989574765855));
#56018=CARTESIAN_POINT('Ctrl Pts',(-2.10220475554805,6.26056944540052,9.65826502338879));
#56019=CARTESIAN_POINT('Ctrl Pts',(-6.40303275178956,1.61714754875415,9.93663429911908));
#56020=CARTESIAN_POINT('Ctrl Pts',(-4.82281693988325,-4.51158856494102,
10.2150035748493));
#56021=CARTESIAN_POINT('Ctrl Pts',(1.18704944568345,-6.49653047621837,10.4933728505796));
#56022=CARTESIAN_POINT('Ctrl Pts',(6.10663719874576,-2.51455298966355,10.7717421263099));
#56023=CARTESIAN_POINT('Ctrl Pts',(5.41741389641379,3.77698574128553,11.0501114020401));
#56024=CARTESIAN_POINT('Ctrl Pts',(-0.247584118732828,6.59944669794996,
11.3284806777704));
#56025=CARTESIAN_POINT('Ctrl Pts',(-5.68518160276977,3.36046198586736,11.6068499535007));
#56026=CARTESIAN_POINT('Ctrl Pts',(-5.9010656645506,-2.96503265371453,11.885219229231));
#56027=CARTESIAN_POINT('Ctrl Pts',(-0.696951573381226,-6.56721045188083,
12.1635885049612));
#56028=CARTESIAN_POINT('Ctrl Pts',(5.14729710620909,-4.13755085954758,12.4419577806915));
#56029=CARTESIAN_POINT('Ctrl Pts',(6.26386736392848,2.09235758465016,12.7203270564218));
#56030=CARTESIAN_POINT('Ctrl Pts',(1.62721414088477,6.40048191581196,12.998696332152));
#56031=CARTESIAN_POINT('Ctrl Pts',(-4.5039992411877,4.82990532519139,13.2770656078823));
#56032=CARTESIAN_POINT('Ctrl Pts',(-6.49838904666884,-1.17683236404584,
13.5554348836125));
#56033=CARTESIAN_POINT('Ctrl Pts',(-2.5241523985111,-6.1026755840387,13.8338041593428));
#56034=CARTESIAN_POINT('Ctrl Pts',(3.76846233851968,-5.42334640402861,14.1121734350731));
#56035=CARTESIAN_POINT('Ctrl Pts',(6.59982785798315,0.237206365684181,14.3905427108034));
#56036=CARTESIAN_POINT('Ctrl Pts',(3.36939762164865,5.67989034068083,14.6689119865337));
#56037=CARTESIAN_POINT('Ctrl Pts',(-2.95574972579951,5.90572080049231,14.9472812622639));
#56038=CARTESIAN_POINT('Ctrl Pts',(-6.56610639558182,0.707277468064,15.2256505379942));
#56039=CARTESIAN_POINT('Ctrl Pts',(-4.14563972612946,-5.14078455841797,
15.5040198137245));
#56040=CARTESIAN_POINT('Ctrl Pts',(2.08250524004114,-6.26714979397594,15.7823890894547));
#56041=CARTESIAN_POINT('Ctrl Pts',(6.39791525355102,-1.63727670945095,16.060758365185));
#56042=CARTESIAN_POINT('Ctrl Pts',(4.83698176773478,4.49639878052789,16.3391276409153));
#56043=CARTESIAN_POINT('Ctrl Pts',(-1.16661237248937,6.50023154874395,16.6174969166455));
#56044=CARTESIAN_POINT('Ctrl Pts',(-6.09869887942524,2.53374556596133,16.8958661923758));
#56045=CARTESIAN_POINT('Ctrl Pts',(-5.42926550149442,-3.7599296175878,17.1742354681061));
#56046=CARTESIAN_POINT('Ctrl Pts',(0.226828026102262,-6.60019269881615,
17.4526047438363));
#56047=CARTESIAN_POINT('Ctrl Pts',(5.6745850340942,-3.37832492601962,17.7309740195666));
#56048=CARTESIAN_POINT('Ctrl Pts',(5.91036133353191,2.94645948928919,18.0093432952969));
#56049=CARTESIAN_POINT('Ctrl Pts',(0.717601613882474,6.5649861034647,18.2877125710271));
#56050=CARTESIAN_POINT('Ctrl Pts',(-5.13425929916017,4.1537183419099,18.5660818467574));
#56051=CARTESIAN_POINT('Ctrl Pts',(-6.27041672742644,-2.0726477460828,18.8444511224877));
#56052=CARTESIAN_POINT('Ctrl Pts',(-1.64733522957113,-6.39533277135328,
19.1228203982179));
#56053=CARTESIAN_POINT('Ctrl Pts',(4.4887872017552,-4.84404625001559,19.4011896739482));
#56054=CARTESIAN_POINT('Ctrl Pts',(6.50205797788772,1.15638949628489,19.6795589496785));
#56055=CARTESIAN_POINT('Ctrl Pts',(2.54333246829336,6.09470709473853,19.9579282254088));
#56056=CARTESIAN_POINT('Ctrl Pts',(-3.75138759958863,5.43517117417511,20.236297501139));
#56057=CARTESIAN_POINT('Ctrl Pts',(-6.60054121954685,-0.216449125649467,
20.5146667768693));
#56058=CARTESIAN_POINT('Ctrl Pts',(-3.3872438769059,-5.6692656961281,20.7930360525995));
#56059=CARTESIAN_POINT('Ctrl Pts',(2.9371619671552,-5.91498725219492,21.0714053283298));
#56060=CARTESIAN_POINT('Ctrl Pts',(6.5638495782996,-0.727923985308585,21.3497746040601));
#56061=CARTESIAN_POINT('Ctrl Pts',(4.1617866869132,5.12772134457041,21.6281438797904));
#56062=CARTESIAN_POINT('Ctrl Pts',(-2.06278512714925,6.27366815620202,21.9065131555207));
#56063=CARTESIAN_POINT('Ctrl Pts',(-6.39273447560434,1.65738967637402,22.1848824312509));
#56064=CARTESIAN_POINT('Ctrl Pts',(-4.85109875456583,-4.48116452369038,
22.4632517069812));
#56065=CARTESIAN_POINT('Ctrl Pts',(1.14616376071003,-6.50386832958405,22.7416209827114));
#56066=CARTESIAN_POINT('Ctrl Pts',(6.09070023984887,-2.55291308180212,23.0199902584417));
#56067=CARTESIAN_POINT('Ctrl Pts',(5.44106340746798,3.74283630564365,23.298359534172));
#56068=CARTESIAN_POINT('Ctrl Pts',(-0.20606968998917,6.60087341931348,23.5767288099022));
#56069=CARTESIAN_POINT('Ctrl Pts',(-5.66393233993547,3.39615445225397,23.8550980856326));
#56070=CARTESIAN_POINT('Ctrl Pts',(-5.91959854504302,-2.92785718238713,
24.1334673613628));
#56071=CARTESIAN_POINT('Ctrl Pts',(-0.738244556818558,-6.56269682289676,
24.4118366370931));
#56072=CARTESIAN_POINT('Ctrl Pts',(5.12117071081501,-4.16984474118904,24.6902059128233));
#56073=CARTESIAN_POINT('Ctrl Pts',(6.27690407226291,2.05291740762767,24.9685751885536));
#56074=CARTESIAN_POINT('Ctrl Pts',(1.66744002499811,6.39012037272897,25.2469444642839));
#56075=CARTESIAN_POINT('Ctrl Pts',(-4.47353076518193,4.85813926394686,25.5253137400141));
#56076=CARTESIAN_POINT('Ctrl Pts',(-6.50566259935649,-1.13593519104989,
25.8036830157444));
#56077=CARTESIAN_POINT('Ctrl Pts',(-2.56248738279775,-6.08667832466393,
26.0820522914747));
#56078=CARTESIAN_POINT('Ctrl Pts',(3.73427575689756,-5.4469421868034,26.360421567205));
#56079=CARTESIAN_POINT('Ctrl Pts',(6.6011892972946,0.195689744786494,26.6387908429352));
#56080=CARTESIAN_POINT('Ctrl Pts',(3.40505663003075,5.65858497870404,26.9171601186655));
#56081=CARTESIAN_POINT('Ctrl Pts',(-2.91854515799281,5.92419520067394,27.1955293943957));
#56082=CARTESIAN_POINT('Ctrl Pts',(-6.56152784010658,0.748563302892809,
27.4738986701261));
#56083=CARTESIAN_POINT('Ctrl Pts',(-4.17789248481245,-5.11460741409143,
27.7522679458563));
#56084=CARTESIAN_POINT('Ctrl Pts',(2.04304461191766,-6.28012446760776,28.0306372215866));
#56085=CARTESIAN_POINT('Ctrl Pts',(6.38749046919093,-1.67748625059234,28.3090064973168));
#56086=CARTESIAN_POINT('Ctrl Pts',(4.86516776074983,4.46588594510562,28.5873757730471));
#56087=CARTESIAN_POINT('Ctrl Pts',(-1.12570381259618,6.50744078276843,28.8657450487773));
#56088=CARTESIAN_POINT('Ctrl Pts',(-6.0826413591286,2.57205534760617,29.1441143245077));
#56089=CARTESIAN_POINT('Ctrl Pts',(-5.45280749764514,-3.72570597451763,
29.4224836002379));
#56090=CARTESIAN_POINT('Ctrl Pts',(0.185309315707581,-6.60148885270917,
29.7008528759682));
#56091=CARTESIAN_POINT('Ctrl Pts',(5.653223625656,-3.41395038822422,29.9792221516984));
#56092=CARTESIAN_POINT('Ctrl Pts',(5.92877720772165,2.90922591699779,30.2575914274287));
#56093=CARTESIAN_POINT('Ctrl Pts',(0.758880198016653,6.56034263281954,30.535960703159));
#56094=CARTESIAN_POINT('Ctrl Pts',(-5.10803147062861,4.18592989788399,30.8143299788893));
#56095=CARTESIAN_POINT('Ctrl Pts',(-6.28332933427362,-2.03316676443131,
31.0926992546195));
#56096=CARTESIAN_POINT('Ctrl Pts',(-1.68752832831564,-6.38484477149316,
31.3710685303498));
#56097=CARTESIAN_POINT('Ctrl Pts',(4.45823008236447,-4.87218422759566,31.6494378060801));
#56098=CARTESIAN_POINT('Ctrl Pts',(6.50920287542301,1.11546965064781,31.9278070818103));
#56099=CARTESIAN_POINT('Ctrl Pts',(2.58161695256905,6.07858935322493,32.2061763575406));
#56100=CARTESIAN_POINT('Ctrl Pts',(-3.71712697969412,5.45865932549019,32.4845456332708));
#56101=CARTESIAN_POINT('Ctrl Pts',(-6.60177208481647,-0.174928428419658,
32.7629149090012));
#56102=CARTESIAN_POINT('Ctrl Pts',(-3.42283570484306,-5.64784829404818,
33.0412841847314));
#56103=CARTESIAN_POINT('Ctrl Pts',(2.89989948244532,-5.93334455485646,33.3196534604617));
#56104=CARTESIAN_POINT('Ctrl Pts',(6.55914120396629,-0.769195216679829,
33.5980227361919));
#56105=CARTESIAN_POINT('Ctrl Pts',(4.1939569605299,5.1014428966866,33.8763920119222));
#56106=CARTESIAN_POINT('Ctrl Pts',(-2.02328388959324,6.28651866433592,34.1547612876525));
#56107=CARTESIAN_POINT('Ctrl Pts',(-6.38218328617755,1.6975662333374,34.4331305633827));
#56108=CARTESIAN_POINT('Ctrl Pts',(-4.87918864713492,-4.45056319588893,
34.711499839113));
#56109=CARTESIAN_POINT('Ctrl Pts',(1.10523273051034,-6.51094887296314,34.9898691148433));
#56110=CARTESIAN_POINT('Ctrl Pts',(6.07452231697217,-2.59117217404372,35.2682383905736));
#56111=CARTESIAN_POINT('Ctrl Pts',(5.46449765586899,3.70853879364014,35.5466076663039));
#56112=CARTESIAN_POINT('Ctrl Pts',(-0.164547108591434,6.60203899291617,
35.8249769420341));
#56113=CARTESIAN_POINT('Ctrl Pts',(-5.64245899717211,3.43171255791666,36.1033462177644));
#56114=CARTESIAN_POINT('Ctrl Pts',(-5.9378972307847,-2.8905658773968,36.3817154934946));
#56115=CARTESIAN_POINT('Ctrl Pts',(-0.779508333376514,-6.55792355651757,
36.6600847692249));
#56116=CARTESIAN_POINT('Ctrl Pts',(5.09484170855686,-4.2019736529018,36.9384540449552));
#56117=CARTESIAN_POINT('Ctrl Pts',(6.28969244990843,2.01339601184075,37.2168233206854));
#56118=CARTESIAN_POINT('Ctrl Pts',(1.70759994083701,6.37950601982511,37.4951925964157));
#56119=CARTESIAN_POINT('Ctrl Pts',(-4.44288530463679,4.88618100204791,37.773561872146));
#56120=CARTESIAN_POINT('Ctrl Pts',(-6.51267877107156,-1.09499307749649,
38.0519311478762));
#56121=CARTESIAN_POINT('Ctrl Pts',(-2.60072098840308,-6.07044026042684,
38.3303004236065));
#56122=CARTESIAN_POINT('Ctrl Pts',(3.69994143759137,-5.47032247434516,38.6086696993368));
#56123=CARTESIAN_POINT('Ctrl Pts',(6.60228957634829,0.154165381892458,38.887038975067));
#56124=CARTESIAN_POINT('Ctrl Pts',(3.44058092549562,5.63705574835366,39.1654082507973));
#56125=CARTESIAN_POINT('Ctrl Pts',(-2.88122512493104,5.94243522424916,39.4437775265276));
#56126=CARTESIAN_POINT('Ctrl Pts',(-6.55668969348419,0.789819522605984,
39.7221468022579));
#56127=CARTESIAN_POINT('Ctrl Pts',(-4.20997995517711,-5.08822792256188,
40.0005160779881));
#56128=CARTESIAN_POINT('Ctrl Pts',(2.00350315562306,-6.29285068314352,40.2788853537184));
#56129=CARTESIAN_POINT('Ctrl Pts',(6.37681297905581,-1.71762942600455,40.5572546294486));
#56130=CARTESIAN_POINT('Ctrl Pts',(4.89316127504496,4.43519642759279,40.835623905179));
#56131=CARTESIAN_POINT('Ctrl Pts',(-1.0847507169254,6.5143925654708,41.1139931809092));
#56132=CARTESIAN_POINT('Ctrl Pts',(-6.06634319368244,2.61026337203627,41.3923624566395));
#56133=CARTESIAN_POINT('Ctrl Pts',(-5.47613376651594,-3.69133493280621,
41.6707317323698));
#56134=CARTESIAN_POINT('Ctrl Pts',(0.143783273993165,-6.60252383449323,
41.9491010081));
#56135=CARTESIAN_POINT('Ctrl Pts',(5.63163856095328,-3.44944078565142,42.2274702838303));
#56136=CARTESIAN_POINT('Ctrl Pts',(5.94695852402892,2.87187724814471,42.5058395595606));
#56137=CARTESIAN_POINT('Ctrl Pts',(0.800128758871884,6.55543961791714,42.7842088352908));
#56138=CARTESIAN_POINT('Ctrl Pts',(-5.08160155505548,4.21797584755876,43.0625781110211));
#56139=CARTESIAN_POINT('Ctrl Pts',(-6.29599335623184,-1.99360534540212,
43.3409473867513));
#56140=CARTESIAN_POINT('Ctrl Pts',(-1.72765466404024,-6.37410417052871,
43.6193166624817));
#56141=CARTESIAN_POINT('Ctrl Pts',(4.42749658376913,-4.90012944886603,43.8976859382118));
#56142=CARTESIAN_POINT('Ctrl Pts',(6.51609025192318,1.07450567412324,44.1760552139422));
#56143=CARTESIAN_POINT('Ctrl Pts',(2.61979930134795,6.06223112686972,44.4544244896724));
#56144=CARTESIAN_POINT('Ctrl Pts',(-3.68271930056586,5.4819315180118,44.7327937654027));
#56145=CARTESIAN_POINT('Ctrl Pts',(-6.60274176677173,-0.133400810565267,
45.011163041133));
#56146=CARTESIAN_POINT('Ctrl Pts',(-3.45829211647637,-5.62620744836598,
45.2895323168632));
#56147=CARTESIAN_POINT('Ctrl Pts',(2.86252227015201,-5.95146711893926,45.5679015925936));
#56148=CARTESIAN_POINT('Ctrl Pts',(6.5541733329074,-0.810436016682913,45.8462708683237));
#56149=CARTESIAN_POINT('Ctrl Pts',(4.22596131027567,5.07496262242242,46.1246401440542));
#56150=CARTESIAN_POINT('Ctrl Pts',(-1.98370260565189,6.2991204614026,46.4030094197842));
#56151=CARTESIAN_POINT('Ctrl Pts',(-6.37137960094171,1.73767563015518,46.6813786955147));
#56152=CARTESIAN_POINT('Ctrl Pts',(-4.90708550628124,-4.41978579220487,
46.9597479712447));
#56153=CARTESIAN_POINT('Ctrl Pts',(1.06425797442239,-6.51777182623093,47.2381172469752));
#56154=CARTESIAN_POINT('Ctrl Pts',(6.05810407015644,-2.62932875275904,47.5164865227053));
#56155=CARTESIAN_POINT('Ctrl Pts',(5.48771571449694,3.67409456217375,47.7948557984358));
#56156=CARTESIAN_POINT('Ctrl Pts',(-0.123018017281035,6.60294337264493,
48.0732250741659));
#56157=CARTESIAN_POINT('Ctrl Pts',(-5.62076242402099,3.46713489608425,48.3515943498962));
#56158=CARTESIAN_POINT('Ctrl Pts',(-5.95596099783199,-2.85316021408464,
48.6299636256265));
#56159=CARTESIAN_POINT('Ctrl Pts',(-0.820741270552748,-6.55289084158609,
48.9083329013567));
#56160=CARTESIAN_POINT('Ctrl Pts',(5.06831114107852,-4.23393632358243,49.186702177087));
#56161=CARTESIAN_POINT('Ctrl Pts',(6.30223199092358,1.9737949608586,49.4650714528173));
#56162=CARTESIAN_POINT('Ctrl Pts',(1.74769229957064,6.36863927703186,49.7434407285475));
#56163=CARTESIAN_POINT('Ctrl Pts',(-4.41206407196639,4.91402943009041,50.0218100042778));
#56164=CARTESIAN_POINT('Ctrl Pts',(-6.51943728423605,-1.05400764316224,
50.3001792800081));
#56165=CARTESIAN_POINT('Ctrl Pts',(-2.63885170270617,-6.05396203374749,
50.5785485557384));
#56166=CARTESIAN_POINT('Ctrl Pts',(3.66546073895617,-5.49348634166886,50.8569178314686));
#56167=CARTESIAN_POINT('Ctrl Pts',(6.60312865161432,0.112634919813896,51.1352871071989));
#56168=CARTESIAN_POINT('Ctrl Pts',(3.47596910260962,5.61530350138215,51.4136563829291));
#56169=CARTESIAN_POINT('Ctrl Pts',(-2.84379110309206,5.96044014959515,51.6920256586594));
#56170=CARTESIAN_POINT('Ctrl Pts',(-6.5515921471244,0.831044494999726,51.9703949343897));
#56171=CARTESIAN_POINT('Ctrl Pts',(-4.24190086775932,-5.06164712747087,
52.24876421012));
#56172=CARTESIAN_POINT('Ctrl Pts',(1.96388243552059,-6.3053279371009,52.5271334858502));
#56173=CARTESIAN_POINT('Ctrl Pts',(6.36588320557505,-1.75770464751873,52.8055027615806));
#56174=CARTESIAN_POINT('Ctrl Pts',(4.92096120312361,4.40433144214688,53.0838720373107));
#56175=CARTESIAN_POINT('Ctrl Pts',(-1.04375470568844,6.52108662182038,53.3622413130411));
#56176=CARTESIAN_POINT('Ctrl Pts',(-6.04980502788473,2.64836812764239,53.6406105887712));
#56177=CARTESIAN_POINT('Ctrl Pts',(-5.4992433852587,-3.65681785226164,53.9189798645017));
#56178=CARTESIAN_POINT('Ctrl Pts',(0.102251543837575,-6.60329760322176,
54.1973491402318));
#56179=CARTESIAN_POINT('Ctrl Pts',(5.60983069394753,-3.48479471420852,54.4757184159621));
#56180=CARTESIAN_POINT('Ctrl Pts',(5.96490456315336,2.83441496034078,54.7540876916924));
#56181=CARTESIAN_POINT('Ctrl Pts',(0.8413456645475,6.55027725273354,55.0324569674226));
#56182=CARTESIAN_POINT('Ctrl Pts',(-5.05497059807721,4.24985492311284,55.310826243153));
#56183=CARTESIAN_POINT('Ctrl Pts',(-6.30840829227937,-1.95396505414819,
55.5891955188831));
#56184=CARTESIAN_POINT('Ctrl Pts',(-1.76771264924237,-6.36311139338609,
55.8675647946135));
#56185=CARTESIAN_POINT('Ctrl Pts',(4.39658792186652,-4.92788080824088,56.1459340703437));
#56186=CARTESIAN_POINT('Ctrl Pts',(6.52271983490569,1.03349918735298,56.424303346074));
#56187=CARTESIAN_POINT('Ctrl Pts',(2.65787800403672,6.04563306284703,56.7026726218042));
#56188=CARTESIAN_POINT('Ctrl Pts',(-3.64816592346122,5.50498683103127,56.9810418975345));
#56189=CARTESIAN_POINT('Ctrl Pts',(-6.60345022704949,-0.091867915026958,
57.2594111732648));
#56190=CARTESIAN_POINT('Ctrl Pts',(-3.49361170905798,-5.60434401524959,
57.537780448995));
#56191=CARTESIAN_POINT('Ctrl Pts',(2.82503180901495,-5.96935422746755,57.8161497247253));
#56192=CARTESIAN_POINT('Ctrl Pts',(6.54894616166488,-0.851644753724631,
58.0945190004557));
#56193=CARTESIAN_POINT('Ctrl Pts',(4.25779846997512,5.04828156940651,58.3728882761858));
#56194=CARTESIAN_POINT('Ctrl Pts',(-1.94404284126394,6.3114730488422,58.6512575519163));
#56195=CARTESIAN_POINT('Ctrl Pts',(-6.36032384731875,1.777716279995,58.9296268276463));
#56196=CARTESIAN_POINT('Ctrl Pts',(-4.9347882283323,-4.38883353027258,59.2079961033768));
#56197=CARTESIAN_POINT('Ctrl Pts',(1.02324111351451,-6.52433691945361,59.4863653791069));
#56198=CARTESIAN_POINT('Ctrl Pts',(6.04144614895033,-2.66738130837423,59.7647346548373));
#56199=CARTESIAN_POINT('Ctrl Pts',(5.51071666478489,3.63950497394812,60.0431039305674));
#56200=CARTESIAN_POINT('Ctrl Pts',(-0.0814840590571557,6.60358652272017,
60.3214732062978));
#56201=CARTESIAN_POINT('Ctrl Pts',(-5.59884347885518,3.5024200653566,60.599842482028));
#56202=CARTESIAN_POINT('Ctrl Pts',(-5.97378913153509,-2.81564167231632,
60.8782117577583));
#56203=CARTESIAN_POINT('Ctrl Pts',(-0.861941737064719,-6.54759887720963,
61.1565810334886));
#56204=CARTESIAN_POINT('Ctrl Pts',(5.04158005799836,-4.26573148870439,61.4349503092188));
#56205=CARTESIAN_POINT('Ctrl Pts',(6.31452219921142,1.93411582140191,61.7133195849491));
#56206=CARTESIAN_POINT('Ctrl Pts',(1.78771551504092,6.35752057426587,61.9916888606794));
#56207=CARTESIAN_POINT('Ctrl Pts',(-4.38106828653906,4.94168344631802,62.2700581364097));
#56208=CARTESIAN_POINT('Ctrl Pts',(-6.5259378714655,-1.01298050953772,62.5484274121399));
#56209=CARTESIAN_POINT('Ctrl Pts',(-2.67687801715671,-6.03724429654741,
62.8267966878701));
#56210=CARTESIAN_POINT('Ctrl Pts',(3.6308350251382,-5.51643287235161,63.1051659636005));
#56211=CARTESIAN_POINT('Ctrl Pts',(6.6037064898967,0.0711000016040934,63.3835352393307));
#56212=CARTESIAN_POINT('Ctrl Pts',(3.51121976132422,5.59332909836506,63.661904515061));
#56213=CARTESIAN_POINT('Ctrl Pts',(-2.80624457346302,5.97820926439015,63.9402737907912));
#56214=CARTESIAN_POINT('Ctrl Pts',(-6.54623540269939,0.872236589107022,
64.2186430665216));
#56215=CARTESIAN_POINT('Ctrl Pts',(-4.2736539596849,-5.03486608042374,64.4970123422518));
#56216=CARTESIAN_POINT('Ctrl Pts',(1.92418401910897,-6.31755573584725,64.775381617982));
#56217=CARTESIAN_POINT('Ctrl Pts',(6.35470158115881,-1.79771032965511,65.0537508937123));
#56218=CARTESIAN_POINT('Ctrl Pts',(4.94856644514845,4.37329220986693,65.3321201694426));
#56219=CARTESIAN_POINT('Ctrl Pts',(-1.00271740079401,6.52752268698292,65.6104894451728));
#56220=CARTESIAN_POINT('Ctrl Pts',(-6.03302751602829,2.68636810690132,65.8888587209031));
#56221=CARTESIAN_POINT('Ctrl Pts',(-5.52213543959689,-3.62215609846939,
66.1672279966334));
#56222=CARTESIAN_POINT('Ctrl Pts',(0.0607157683442206,-6.60381012828248,
66.4455972723636));
#56223=CARTESIAN_POINT('Ctrl Pts',(5.58780088741481,-3.520010775202,66.723966548094));
#56224=CARTESIAN_POINT('Ctrl Pts',(5.9826146151029,2.79684053569169,67.0023358238242));
#56225=CARTESIAN_POINT('Ctrl Pts',(0.882529284395388,6.54485574150535,67.2807050995545));
#56226=CARTESIAN_POINT('Ctrl Pts',(-5.02813965328381,4.28156586332698,67.5590743752847));
#56227=CARTESIAN_POINT('Ctrl Pts',(-6.320573651249,-1.91424745894271,67.8374436510151));
#56228=CARTESIAN_POINT('Ctrl Pts',(-1.80770069912375,-6.35186687496823,
68.1158129267453));
#56229=CARTESIAN_POINT('Ctrl Pts',(4.36550531948381,-4.95543720780412,68.3941822024755));
#56230=CARTESIAN_POINT('Ctrl Pts',(6.52909136208694,0.992451812660304,68.6725514782058));
#56231=CARTESIAN_POINT('Ctrl Pts',(2.69585155414282,6.02879581781948,68.9509207539361));
#56232=CARTESIAN_POINT('Ctrl Pts',(-3.61346821540184,5.52782435242044,69.2292900296664));
#56233=CARTESIAN_POINT('Ctrl Pts',(-6.60389743762118,-0.0503313849543038,
69.5076593053966));
#56234=CARTESIAN_POINT('Ctrl Pts',(-3.52879308525274,-5.58225885967351,
69.786028581127));
#56235=CARTESIAN_POINT('Ctrl Pts',(2.78742958225481,-5.98700517278068,70.0643978568572));
#56236=CARTESIAN_POINT('Ctrl Pts',(6.54345989703921,-0.892819797479564,
70.3427671325874));
#56237=CARTESIAN_POINT('Ctrl Pts',(4.28946718006704,5.02140079321086,70.6211364083178));
#56238=CARTESIAN_POINT('Ctrl Pts',(-1.9043061654729,6.32357593795416,70.8995056840479));
#56239=CARTESIAN_POINT('Ctrl Pts',(-6.34901646270328,1.81768659874434,71.1778749597783));
#56240=CARTESIAN_POINT('Ctrl Pts',(-4.96229571729612,-4.3577076346442,71.4562442355084));
#56241=CARTESIAN_POINT('Ctrl Pts',(0.982183770520482,-6.53064389289886,
71.7346135112389));
#56242=CARTESIAN_POINT('Ctrl Pts',(6.02454921238457,-2.7053283354313,72.0129827869689));
#56243=CARTESIAN_POINT('Ctrl Pts',(5.53349959675533,3.60477139741766,72.2913520626995));
#56244=CARTESIAN_POINT('Ctrl Pts',(-0.0399468771114501,6.60396841769711,
72.5697213384295));
#56245=CARTESIAN_POINT('Ctrl Pts',(-5.57670302884517,3.53756666976046,72.84809061416));
#56246=CARTESIAN_POINT('Ctrl Pts',(-5.99138092656673,-2.77801173642291,
73.12645988989));
#56247=CARTESIAN_POINT('Ctrl Pts',(-0.903108102914542,-6.54204787275223,
73.4048291656205));
#56248=CARTESIAN_POINT('Ctrl Pts',(5.01464951686801,-4.2973578903679,73.6831984413506));
#56249=CARTESIAN_POINT('Ctrl Pts',(6.32656258853912,1.89436016328156,73.961567717081));
#56250=CARTESIAN_POINT('Ctrl Pts',(1.82766800382458,6.34615035141201,74.2399369928112));
#56251=CARTESIAN_POINT('Ctrl Pts',(-4.34989917462906,4.96914195666549,74.5183062685415));
#56252=CARTESIAN_POINT('Ctrl Pts',(-6.53218027557985,-0.971913299763653,
74.7966755442717));
#56253=CARTESIAN_POINT('Ctrl Pts',(-2.71479842733392,-6.02028771022417,
75.0750448200021));
#56254=CARTESIAN_POINT('Ctrl Pts',(3.59606566602131,-5.53916115856847,75.3534140957322));
#56255=CARTESIAN_POINT('Ctrl Pts',(6.60402306833451,0.029562270492965,75.6317833714626));
#56256=CARTESIAN_POINT('Ctrl Pts',(3.54633150703141,5.57113340866723,75.9101526471928));
#56257=CARTESIAN_POINT('Ctrl Pts',(-2.76858702148319,5.99574186564154,76.1885219229231));
#56258=CARTESIAN_POINT('Ctrl Pts',(-6.54061967213588,0.913394175260629,
76.4668911986534));
#56259=CARTESIAN_POINT('Ctrl Pts',(-4.30523797471837,-5.00788584094864,
76.7452604743836));
#56260=CARTESIAN_POINT('Ctrl Pts',(1.88440947696132,-6.32953359561905,77.0236297501139));
#56261=CARTESIAN_POINT('Ctrl Pts',(6.34326854818163,-1.83764488968394,77.3019990258441));
#56262=CARTESIAN_POINT('Ctrl Pts',(4.97597590898363,4.34207995874622,77.5803683015745));
#56263=CARTESIAN_POINT('Ctrl Pts',(-0.961640425785212,6.53370050633074,
77.8587375773046));
#56264=CARTESIAN_POINT('Ctrl Pts',(-6.01601132187544,2.72426180643463,78.1371068530351));
#56265=CARTESIAN_POINT('Ctrl Pts',(-5.54480902386091,-3.58735104273928,
78.4154761287652));
#56266=CARTESIAN_POINT('Ctrl Pts',(0.0191775907770066,-6.60406138939841,
78.6938454044956));
#56267=CARTESIAN_POINT('Ctrl Pts',(5.56555001291159,-3.55508757539258,78.9722146802257));
#56268=CARTESIAN_POINT('Ctrl Pts',(6.00008797922182,2.75915546073972,79.2505839559561));
#56269=CARTESIAN_POINT('Ctrl Pts',(0.923677989083838,6.53917529872184,79.5289532316863));
#56270=CARTESIAN_POINT('Ctrl Pts',(-5.00110978217752,4.3131074136334,79.8073225074166));
#56271=CARTESIAN_POINT('Ctrl Pts',(-6.3324889518473,-1.87445413111732,80.0856917831468));
#56272=CARTESIAN_POINT('Ctrl Pts',(-1.84761723165289,-6.34037106013766,
80.3640610588772));
#56273=CARTESIAN_POINT('Ctrl Pts',(4.33425000633009,-4.98279755735265,80.6424303346073));
#56274=CARTESIAN_POINT('Ctrl Pts',(6.53520458139265,0.95136517398707,80.9207996103378));
#56275=CARTESIAN_POINT('Ctrl Pts',(2.73371844933311,6.01172005791245,81.1991688860678));
#56276=CARTESIAN_POINT('Ctrl Pts',(-3.57862754911977,5.55044317866717,81.4775381617983));
#56277=CARTESIAN_POINT('Ctrl Pts',(-6.6040833807941,-0.00879286364105391,
81.7559074375284));
#56278=CARTESIAN_POINT('Ctrl Pts',(-3.56383485319324,-5.55995285538431,
82.0342767132588));
#56279=CARTESIAN_POINT('Ctrl Pts',(2.74971707751372,-6.00441925656099,82.3126459889889));
#56280=CARTESIAN_POINT('Ctrl Pts',(6.53771475608128,-0.933959518955791,
82.5910152647193));
#56281=CARTESIAN_POINT('Ctrl Pts',(4.32096618765487,4.99432135730924,82.8693845404496));
#56282=CARTESIAN_POINT('Ctrl Pts',(-1.86449415036578,6.33542864991657,83.1477538161797));
#56283=CARTESIAN_POINT('Ctrl Pts',(-6.33745789444466,1.85758500507299,83.4261230919102));
#56284=CARTESIAN_POINT('Ctrl Pts',(-4.98960688490476,-4.32640933674127,
83.7044923676402));
#56285=CARTESIAN_POINT('Ctrl Pts',(0.941087569775988,-6.53669249704657,
83.9828616433708));
#56286=CARTESIAN_POINT('Ctrl Pts',(6.00741392894626,-2.74316833264646,84.2612309191007));
#56287=CARTESIAN_POINT('Ctrl Pts',(5.5560636090558,3.56989520673322,84.5396001948314));
#56288=CARTESIAN_POINT('Ctrl Pts',(0.00159188523690413,6.60408904246697,
84.8179694705613));
#56289=CARTESIAN_POINT('Ctrl Pts',(-5.55434194992508,3.57257331880457,85.0963387462919));
#56290=CARTESIAN_POINT('Ctrl Pts',(-6.00873568694944,-2.74027189514327,
85.3747080220218));
#56291=CARTESIAN_POINT('Ctrl Pts',(-0.944238739453256,-6.53623804782589,
85.6530772977524));
#56292=CARTESIAN_POINT('Ctrl Pts',(4.98752058312948,-4.32881427735017,85.9314465734823));
#56293=CARTESIAN_POINT('Ctrl Pts',(6.33835268255775,1.85452955933434,86.2098158492128));
#56294=CARTESIAN_POINT('Ctrl Pts',(1.86754818529735,6.33452905830612,86.4881851249431));
#56295=CARTESIAN_POINT('Ctrl Pts',(-4.31855796936763,4.99640387480258,86.7665544006733));
#56296=CARTESIAN_POINT('Ctrl Pts',(-6.53816424961312,-0.930807638565494,
87.0449236764036));
#56297=CARTESIAN_POINT('Ctrl Pts',(-2.7526114330082,-6.00309294562432,87.3232929521339));
#56298=CARTESIAN_POINT('Ctrl Pts',(3.56115403717188,-5.56167030112953,87.6016622278641));
#56299=CARTESIAN_POINT('Ctrl Pts',(6.60407837440324,-0.0119766301783775,
87.8800315035943));
#56300=CARTESIAN_POINT('Ctrl Pts',(3.58130295061876,5.5487173104079,88.1584007793249));
#56301=CARTESIAN_POINT('Ctrl Pts',(-2.73081993698305,6.01303725971391,88.4367700550547));
#56302=CARTESIAN_POINT('Ctrl Pts',(-6.53474517760702,0.954515625159502,
88.7151393307855));
#56303=CARTESIAN_POINT('Ctrl Pts',(-4.33665166331373,-4.98070747645445,
88.9935086065153));
#56304=CARTESIAN_POINT('Ctrl Pts',(1.84456038266226,-6.34126104254065,89.2718778822459));
#56305=CARTESIAN_POINT('Ctrl Pts',(6.33158455896374,-1.87750674769037,89.5502471579759));
#56306=CARTESIAN_POINT('Ctrl Pts',(5.00318851023979,4.31069592362259,89.8286164337064));
#56307=CARTESIAN_POINT('Ctrl Pts',(-0.92052540577437,6.53961983545342,90.1069857094364));
#56308=CARTESIAN_POINT('Ctrl Pts',(-5.99875711863103,2.76204772706856,90.385354985167));
#56309=CARTESIAN_POINT('Ctrl Pts',(-5.56726324102471,-3.55240406204953,
90.6637242608969));
#56310=CARTESIAN_POINT('Ctrl Pts',(-0.0223613455058675,-6.60405137662928,
90.9420935366275));
#56311=CARTESIAN_POINT('Ctrl Pts',(5.54307895074079,-3.59002372705058,91.2204628123576));
#56312=CARTESIAN_POINT('Ctrl Pts',(6.01732396421797,2.72136122640474,91.4988320880879));
#56313=CARTESIAN_POINT('Ctrl Pts',(0.964790150663175,6.53323614911586,91.7772013638182));
#56314=CARTESIAN_POINT('Ctrl Pts',(-4.97388205413045,4.34447832616656,92.0555706395484));
#56315=CARTESIAN_POINT('Ctrl Pts',(-6.34415372267409,-1.83458664500002,
92.3339399152788));
#56316=CARTESIAN_POINT('Ctrl Pts',(-1.88746066762744,-6.32862440369867,
92.6123091910088));
#56317=CARTESIAN_POINT('Ctrl Pts',(4.30282321894659,-5.00996077443976,92.8906784667394));
#56318=CARTESIAN_POINT('Ctrl Pts',(6.5410592509681,0.910240896827098,93.1690477424694));
#56319=CARTESIAN_POINT('Ctrl Pts',(2.77147719149483,5.99440645868761,93.4474170181999));
#56320=CARTESIAN_POINT('Ctrl Pts',(-3.54364530300244,5.57284241491177,93.7257862939299));
#56321=CARTESIAN_POINT('Ctrl Pts',(-6.60400804921164,0.0327460055409614,
94.0041555696604));
#56322=CARTESIAN_POINT('Ctrl Pts',(-3.59873562653636,-5.53742688486538,
94.2825248453905));
#56323=CARTESIAN_POINT('Ctrl Pts',(2.71189578679664,-6.02159578986222,94.560894121121));
#56324=CARTESIAN_POINT('Ctrl Pts',(6.531710966084,-0.975062290558369,94.839263396851));
#56325=CARTESIAN_POINT('Ctrl Pts',(4.35229424655544,4.96704433303463,95.1176326725814));
#56326=CARTESIAN_POINT('Ctrl Pts',(-1.82460837100929,6.3470307158052,95.3960019483117));
#56327=CARTESIAN_POINT('Ctrl Pts',(-6.32564859983025,1.89740992049619,95.674371224042));
#56328=CARTESIAN_POINT('Ctrl Pts',(-5.01672065065709,-4.29493987480636,
95.9527404997721));
#56329=CARTESIAN_POINT('Ctrl Pts',(0.899954137153977,-6.54248249259793,
96.2311097755025));
#56330=CARTESIAN_POINT('Ctrl Pts',(5.99004097655152,-2.78089980297108,96.5094790512327));
#56331=CARTESIAN_POINT('Ctrl Pts',(5.57840780899557,3.53487778168767,96.7878483269631));
#56332=CARTESIAN_POINT('Ctrl Pts',(0.0431305846059591,6.60394839225773,
97.0662176026933));
#56333=CARTESIAN_POINT('Ctrl Pts',(-5.53176112675738,3.60743862753435,97.3445868784233));
#56334=CARTESIAN_POINT('Ctrl Pts',(-6.02585272608368,-2.70242364156341,
97.622956154154));
#56335=CARTESIAN_POINT('Ctrl Pts',(-0.985332019446007,-6.53016963228263,
97.9013254298839));
#56336=CARTESIAN_POINT('Ctrl Pts',(4.96019433007453,-4.36009940515447,98.1796947056146));
#56337=CARTESIAN_POINT('Ctrl Pts',(6.34989201482012,1.81462558536316,98.4580639813445));
#56338=CARTESIAN_POINT('Ctrl Pts',(1.90735448169537,6.32265715471649,98.7364332570749));
#56339=CARTESIAN_POINT('Ctrl Pts',(-4.28704591069449,5.0234681221771,99.0148025328052));
#56340=CARTESIAN_POINT('Ctrl Pts',(-6.54388955682393,-0.889665152190753,
99.2931718085354));
#56341=CARTESIAN_POINT('Ctrl Pts',(-2.79031553819798,-5.98566068301753,
99.5715410842657));
#56342=CARTESIAN_POINT('Ctrl Pts',(3.52610151978467,-5.58395940951429,99.849910359996));
#56343=CARTESIAN_POINT('Ctrl Pts',(6.60387240591485,-0.0535150570232872,
100.128279635726));
#56344=CARTESIAN_POINT('Ctrl Pts',(3.61613270852506,5.5260816904265,100.406648911456));
#56345=CARTESIAN_POINT('Ctrl Pts',(-2.69294481412704,6.03009476235633,100.685018187187));
#56346=CARTESIAN_POINT('Ctrl Pts',(-6.52861215152283,0.995599311931976,
100.963387462917));
#56347=CARTESIAN_POINT('Ctrl Pts',(-4.36789378266397,-4.95333206218776,
101.241756738647));
#56348=CARTESIAN_POINT('Ctrl Pts',(1.80463831274576,-6.35273761264401,101.520126014377));
#56349=CARTESIAN_POINT('Ctrl Pts',(6.31965007575454,-1.91729432663498,101.798495290108));
#56350=CARTESIAN_POINT('Ctrl Pts',(5.03020317231507,4.27914134613035,102.076864565838));
#56351=CARTESIAN_POINT('Ctrl Pts',(-0.879373967378626,6.54528044016669,
102.355233841568));
#56352=CARTESIAN_POINT('Ctrl Pts',(-5.98126558891647,2.79972437389389,102.633603117299));
#56353=CARTESIAN_POINT('Ctrl Pts',(-5.58949720274087,-3.51731653899433,
102.911972393029));
#56354=CARTESIAN_POINT('Ctrl Pts',(-0.0638993971154535,-6.60378009037091,
103.190341668759));
#56355=CARTESIAN_POINT('Ctrl Pts',(5.52038858991582,-3.62481784801088,103.468710944489));
#56356=CARTESIAN_POINT('Ctrl Pts',(6.03432188819125,2.68345932792503,103.74708022022));
#56357=CARTESIAN_POINT('Ctrl Pts',(1.00586414262883,6.52703852765597,104.02544949595));
#56358=CARTESIAN_POINT('Ctrl Pts',(-4.94645754634252,4.37567735981095,104.30381877168));
#56359=CARTESIAN_POINT('Ctrl Pts',(-6.35556750224043,-1.79464657785212,
104.58218804741));
#56360=CARTESIAN_POINT('Ctrl Pts',(-1.9272294307376,-6.31662737037975,104.860557323141));
#56361=CARTESIAN_POINT('Ctrl Pts',(4.2712262006594,-5.03692578441776,105.138926598871));
#56362=CARTESIAN_POINT('Ctrl Pts',(6.54665513918701,0.869080608164411,105.417295874602));
#56363=CARTESIAN_POINT('Ctrl Pts',(2.80912628679378,5.97685570511578,105.695665150331));
#56364=CARTESIAN_POINT('Ctrl Pts',(-3.50852286103865,5.59502117498236,105.974034426062));
#56365=CARTESIAN_POINT('Ctrl Pts',(-6.60367144585437,0.0742835792054609,
106.252403701792));
#56366=CARTESIAN_POINT('Ctrl Pts',(-3.63349402451605,-5.51468183930289,
106.530772977523));
#56367=CARTESIAN_POINT('Ctrl Pts',(2.67396720641217,-6.03853409313579,106.809142253253));
#56368=CARTESIAN_POINT('Ctrl Pts',(6.52544876457291,-1.01612648615505,107.087511528983));
#56369=CARTESIAN_POINT('Ctrl Pts',(4.38345011734935,4.93957079953733,107.365880804713));
#56370=CARTESIAN_POINT('Ctrl Pts',(-1.78465040538896,6.35838167661206,107.644250080444));
#56371=CARTESIAN_POINT('Ctrl Pts',(-6.31358904606623,1.93715976943654,107.922619356174));
#56372=CARTESIAN_POINT('Ctrl Pts',(-5.04363594186223,-4.26330049385302,
108.200988631904));
#56373=CARTESIAN_POINT('Ctrl Pts',(0.858785100000153,-6.54801365048589,
108.479357907634));
#56374=CARTESIAN_POINT('Ctrl Pts',(5.97243104252002,-2.81852125364953,108.757727183365));
#56375=CARTESIAN_POINT('Ctrl Pts',(5.60053131257941,3.49972050766179,109.036096459095));
#56376=CARTESIAN_POINT('Ctrl Pts',(0.0846675776166999,6.60354647263366,
109.314465734825));
#56377=CARTESIAN_POINT('Ctrl Pts',(-5.50896145269841,3.64216121658758,109.592835010555));
#56378=CARTESIAN_POINT('Ctrl Pts',(-6.04273136677475,-2.66446847305942,
109.871204286286));
#56379=CARTESIAN_POINT('Ctrl Pts',(-1.02638631713515,-6.52384286620461,
110.149573562016));
#56380=CARTESIAN_POINT('Ctrl Pts',(4.93267183880067,-4.3912120360596,110.427942837746));
#56381=CARTESIAN_POINT('Ctrl Pts',(6.36118012880049,1.77464982007316,110.706312113476));
#56382=CARTESIAN_POINT('Ctrl Pts',(1.9470853181774,6.31053511032693,110.984681389207));
#56383=CARTESIAN_POINT('Ctrl Pts',(-4.25536424530892,5.05033362805641,111.263050664937));
#56384=CARTESIAN_POINT('Ctrl Pts',(-6.54935597070397,-0.848487468343064,
111.541419940667));
#56385=CARTESIAN_POINT('Ctrl Pts',(-2.82790925123099,-5.96799161206968,
111.819789216398));
#56386=CARTESIAN_POINT('Ctrl Pts',(3.49090950062908,-5.60602760190756,112.098158492128));
#56387=CARTESIAN_POINT('Ctrl Pts',(6.6034051710178,-0.095051366672858,112.376527767858));
#56388=CARTESIAN_POINT('Ctrl Pts',(3.6508194027943,5.50322744424684,112.654897043588));
#56389=CARTESIAN_POINT('Ctrl Pts',(-2.65496315135363,6.04691369872981,112.933266319319));
#56390=CARTESIAN_POINT('Ctrl Pts',(-6.52222083652212,1.03664361020002,113.211635595049));
#56391=CARTESIAN_POINT('Ctrl Pts',(-4.39896309674896,-4.92576068119147,
113.490004870779));
#56392=CARTESIAN_POINT('Ctrl Pts',(1.76464484663277,-6.36396285188586,113.768374146509));
#56393=CARTESIAN_POINT('Ctrl Pts',(6.30746557071311,-1.95700605241798,114.04674342224));
#56394=CARTESIAN_POINT('Ctrl Pts',(5.05701882643932,4.24741747465094,114.32511269797));
#56395=CARTESIAN_POINT('Ctrl Pts',(-0.838187738656269,6.55068209652226,
114.603481973701));
#56396=CARTESIAN_POINT('Ctrl Pts',(-5.963537424742,2.83729025632424,114.88185124943));
#56397=CARTESIAN_POINT('Ctrl Pts',(-5.61151002937618,-3.48208986172708,
115.160220525161));
#56398=CARTESIAN_POINT('Ctrl Pts',(-0.105434920698308,-6.60324754135638,
115.438589800891));
#56399=CARTESIAN_POINT('Ctrl Pts',(5.49747982812689,-3.65946856172709,115.716959076621));
#56400=CARTESIAN_POINT('Ctrl Pts',(6.05108107865909,2.64545126479867,115.995328352351));
#56401=CARTESIAN_POINT('Ctrl Pts',(1.04689833998677,6.520582679536,116.273697628082));
#56402=CARTESIAN_POINT('Ctrl Pts',(-4.91883734379885,4.40670328025178,116.552066903812));
#56403=CARTESIAN_POINT('Ctrl Pts',(-6.36672983898753,-1.75463550980728,
116.830436179542));
#56404=CARTESIAN_POINT('Ctrl Pts',(-1.96692194762707,-6.30438043481466,
117.108805455273));
#56405=CARTESIAN_POINT('Ctrl Pts',(4.23946020152865,-5.06369152048054,117.387174731003));
#56406=CARTESIAN_POINT('Ctrl Pts',(6.55199202466173,0.827885936407187,117.665544006733));
#56407=CARTESIAN_POINT('Ctrl Pts',(2.84666424573328,5.95906849155092,117.943913282464));
#56408=CARTESIAN_POINT('Ctrl Pts',(-3.47326161276393,5.61697858142893,118.222282558194));
#56409=CARTESIAN_POINT('Ctrl Pts',(-6.60307358403887,0.115818214018131,
118.500651833924));
#56410=CARTESIAN_POINT('Ctrl Pts',(-3.66810867199999,-5.49171861855029,
118.779021109654));
#56411=CARTESIAN_POINT('Ctrl Pts',(2.63593283691441,-6.05523349625818,119.057390385385));
#56412=CARTESIAN_POINT('Ctrl Pts',(6.51892839929654,-1.05715048113904,119.335759661115));
#56413=CARTESIAN_POINT('Ctrl Pts',(4.41443256742969,4.91190184374221,119.614128936845));
#56414=CARTESIAN_POINT('Ctrl Pts',(-1.74462183434705,6.36948108326269,119.892498212575));
#56415=CARTESIAN_POINT('Ctrl Pts',(-6.3012797102582,1.97683297928823,120.170867488306));
#56416=CARTESIAN_POINT('Ctrl Pts',(-5.07035169368467,-4.23149244562176,
120.449236764036));
#56417=CARTESIAN_POINT('Ctrl Pts',(0.817582087076372,-6.55328575187579,
120.727606039766));
#56418=CARTESIAN_POINT('Ctrl Pts',(5.95458482353203,-2.85603119629362,121.005975315497));
#56419=CARTESIAN_POINT('Ctrl Pts',(5.62243324457135,3.4644247755954,121.284344591226));
#56420=CARTESIAN_POINT('Ctrl Pts',(0.126201220905966,6.60288329944592,121.562713866957));
#56421=CARTESIAN_POINT('Ctrl Pts',(-5.48594382966552,3.67673971234222,121.841083142687));
#56422=CARTESIAN_POINT('Ctrl Pts',(-6.05937094144284,-2.62640789141387,
122.119452418417));
#56423=CARTESIAN_POINT('Ctrl Pts',(-1.0674000079603,-6.5172579995599,122.397821694148));
#56424=CARTESIAN_POINT('Ctrl Pts',(4.90495419751704,-4.4221509398022,122.676190969878));
#56425=CARTESIAN_POINT('Ctrl Pts',(6.37221657914332,1.73460384620578,122.954560245608));
#56426=CARTESIAN_POINT('Ctrl Pts',(1.98673912056242,6.29816340245835,123.232929521338));
#56427=CARTESIAN_POINT('Ctrl Pts',(-4.22351422222807,5.07699933383612,123.511298797069));
#56428=CARTESIAN_POINT('Ctrl Pts',(-6.55456328328112,-0.80727622417212,
123.789668072799));
#56429=CARTESIAN_POINT('Ctrl Pts',(-2.86539106914205,-5.95008641661004,
124.068037348529));
#56430=CARTESIAN_POINT('Ctrl Pts',(3.45557934242459,-5.62787403394446,124.34640662426));
#56431=CARTESIAN_POINT('Ctrl Pts',(6.60267674402822,-0.136583861631543,
124.62477589999));
#56432=CARTESIAN_POINT('Ctrl Pts',(3.68536155571016,5.48015537368143,124.90314517572));
#56433=CARTESIAN_POINT('Ctrl Pts',(-2.61687625226222,6.06349359671225,125.18151445145));
#56434=CARTESIAN_POINT('Ctrl Pts',(-6.51557186131684,1.07764653119394,125.459883727181));
#56435=CARTESIAN_POINT('Ctrl Pts',(-4.42985766669503,-4.89799373516042,
125.738253002911));
#56436=CARTESIAN_POINT('Ctrl Pts',(1.72458022652849,-6.37493761732919,126.016622278641));
#56437=CARTESIAN_POINT('Ctrl Pts',(6.29503405616005,-1.99663789708001,126.294991554372));
#56438=CARTESIAN_POINT('Ctrl Pts',(5.08362963405118,4.21552092521275,126.573360830102));
#56439=CARTESIAN_POINT('Ctrl Pts',(-0.796959327840158,6.55583335028739,
126.851730105832));
#56440=CARTESIAN_POINT('Ctrl Pts',(-5.94559036134429,2.87472734849176,127.130099381562));
#56441=CARTESIAN_POINT('Ctrl Pts',(-5.63326868663984,-3.44669419364702,
127.408468657293));
#56442=CARTESIAN_POINT('Ctrl Pts',(-0.14702700410348,-6.60251271983441,
127.686837933023));
#56443=CARTESIAN_POINT('Ctrl Pts',(5.47446824479836,-3.69386315072671,127.965207208753));
#56444=CARTESIAN_POINT('Ctrl Pts',(6.06738434301238,2.60712828918945,128.243576484483));
#56445=CARTESIAN_POINT('Ctrl Pts',(1.08829999938262,6.51426591103059,128.521945760214));
#56446=CARTESIAN_POINT('Ctrl Pts',(-4.89179481848511,4.43680471220902,128.800315035944));
#56447=CARTESIAN_POINT('Ctrl Pts',(-6.37618018613959,-1.7131350353328,129.078684311674));
#56448=CARTESIAN_POINT('Ctrl Pts',(-2.00930903122581,-6.29459439164505,
129.357053587405));
#56449=CARTESIAN_POINT('Ctrl Pts',(4.21288699254892,-5.08490128605854,129.635422863135));
#56450=CARTESIAN_POINT('Ctrl Pts',(6.15710482774512,-0.202003301493498,
129.867397259577));
#56451=CARTESIAN_POINT('Ctrl Pts',(4.72821073371232,3.37844258401427,130.05297677673));
#56452=CARTESIAN_POINT('Ctrl Pts',(3.27532695401748,4.61709096383853,130.145766535307));
#56453=CARTESIAN_POINT('Ctrl Pts',(2.43856727558522,5.02329722221597,130.192161414595));
#56454=CARTESIAN_POINT('Ctrl Pts',(3.05041111877606,-4.274209655604,-10.1921614145953));
#56455=CARTESIAN_POINT('Ctrl Pts',(3.76239094771356,-3.76608502870656,-10.1457665353069));
#56456=CARTESIAN_POINT('Ctrl Pts',(4.9147981139233,-2.38931734182567,-10.0529767767301));
#56457=CARTESIAN_POINT('Ctrl Pts',(5.67693298611737,1.15492319595148,-9.86739725957665));
#56458=CARTESIAN_POINT('Ctrl Pts',(3.10693226149187,5.3766494323891,-9.63542286313474));
#56459=CARTESIAN_POINT('Ctrl Pts',(-2.85220921458105,5.52037841761172,-9.35705358740447));
#56460=CARTESIAN_POINT('Ctrl Pts',(-6.18103028642409,0.586305255261647,
-9.0786843116742));
#56461=CARTESIAN_POINT('Ctrl Pts',(-3.83824771704109,-4.88244921267984,
-8.80031503594394));
#56462=CARTESIAN_POINT('Ctrl Pts',(2.03280072920052,-5.86879411456106,-8.52194576021367));
#56463=CARTESIAN_POINT('Ctrl Pts',(6.03522149624778,-1.46371786530544,-8.24357648448339));
#56464=CARTESIAN_POINT('Ctrl Pts',(4.49524313218507,4.28518771604633,-7.96520720875314));
#56465=CARTESIAN_POINT('Ctrl Pts',(-1.17394980812342,6.09854146397534,-7.68683793302285));
#56466=CARTESIAN_POINT('Ctrl Pts',(-5.7646663724329,2.31036198391266,-7.4084686572926));
#56467=CARTESIAN_POINT('Ctrl Pts',(-5.06078604168037,-3.59975018522352,
-7.13009938156231));
#56468=CARTESIAN_POINT('Ctrl Pts',(0.291378575457491,-6.20361580881232,
-6.85173010583206));
#56469=CARTESIAN_POINT('Ctrl Pts',(5.37588433642207,-3.10957421224122,-6.57336083010178));
#56470=CARTESIAN_POINT('Ctrl Pts',(5.52277741809884,2.84053002303097,-6.29499155437152));
#56471=CARTESIAN_POINT('Ctrl Pts',(0.597112164703471,6.18167690616701,-6.01662227864124));
#56472=CARTESIAN_POINT('Ctrl Pts',(-4.876982327571,3.84508693951616,-5.73825300291099));
#56473=CARTESIAN_POINT('Ctrl Pts',(-5.87167921844947,-2.02312839863673,
-5.45988372718071));
#56474=CARTESIAN_POINT('Ctrl Pts',(-1.47336733630053,-6.03314607562369,
-5.18151445145044));
#56475=CARTESIAN_POINT('Ctrl Pts',(4.2781990691855,-4.50185214896148,-4.90314517572017));
#56476=CARTESIAN_POINT('Ctrl Pts',(6.10033475477778,1.16429302348895,-4.62477589998991));
#56477=CARTESIAN_POINT('Ctrl Pts',(2.31944782925857,5.76106097853586,-4.34640662425962));
#56478=CARTESIAN_POINT('Ctrl Pts',(-3.59180045907085,5.06642190789875,-4.06803734852937));
#56479=CARTESIAN_POINT('Ctrl Pts',(-6.2040596136716,-0.281613464959076,
-3.78966807279909));
#56480=CARTESIAN_POINT('Ctrl Pts',(-3.11802735053584,-5.37099312723374,
-3.51129879706883));
#56481=CARTESIAN_POINT('Ctrl Pts',(2.83184397887941,-5.52723451392706,-3.23292952133855));
#56482=CARTESIAN_POINT('Ctrl Pts',(6.1807293244735,-0.60683338828964,-2.95456024560829));
#56483=CARTESIAN_POINT('Ctrl Pts',(3.85275163306719,4.87093077134018,-2.67619096987801));
#56484=CARTESIAN_POINT('Ctrl Pts',(-2.01389312417038,5.87485286674442,-2.39782169414775));
#56485=CARTESIAN_POINT('Ctrl Pts',(-6.03082163928753,1.48285268448469,-2.11945241841748));
#56486=CARTESIAN_POINT('Ctrl Pts',(-4.50857401099197,-4.27111485599194,
-1.84108314268722));
#56487=CARTESIAN_POINT('Ctrl Pts',(1.15469901830053,-6.10215797095896,-1.56271386695694));
#56488=CARTESIAN_POINT('Ctrl Pts',(5.7574065665386,-2.32850410220939,-1.28434459122668));
#56489=CARTESIAN_POINT('Ctrl Pts',(5.07206366238349,3.58382922732706,-1.0059753154964));
#56490=CARTESIAN_POINT('Ctrl Pts',(-0.271857411234665,6.2044947637884,-0.727606039766137));
#56491=CARTESIAN_POINT('Ctrl Pts',(-5.3660834720623,3.12646923812167,-0.449236764035865));
#56492=CARTESIAN_POINT('Ctrl Pts',(-5.53168067828129,-2.82314905726007,
-0.170867488305599));
#56493=CARTESIAN_POINT('Ctrl Pts',(-0.616551662615334,-6.17976745301254,
0.107501787424673));
#56494=CARTESIAN_POINT('Ctrl Pts',(4.86486640363235,-3.86040627406166,0.385871063154939));
#56495=CARTESIAN_POINT('Ctrl Pts',(5.87801239481268,2.00465259145346,0.664240338885211));
#56496=CARTESIAN_POINT('Ctrl Pts',(1.49233415085848,6.02848243824067,0.942609614615477));
#56497=CARTESIAN_POINT('Ctrl Pts',(-4.26401996776543,4.51528464667454,1.22097889034575));
#56498=CARTESIAN_POINT('Ctrl Pts',(-6.10396615887418,-1.14510211654415,
1.49934816607602));
#56499=CARTESIAN_POINT('Ctrl Pts',(-2.33755458556937,-5.75373794028536,
1.77771744180629));
#56500=CARTESIAN_POINT('Ctrl Pts',(3.57584911702428,-5.07769286371995,2.05608671753656));
#56501=CARTESIAN_POINT('Ctrl Pts',(6.2049145811997,0.262100679150067,2.33445599326682));
#56502=CARTESIAN_POINT('Ctrl Pts',(3.13490339023048,5.36116055158928,2.61282526899709));
#56503=CARTESIAN_POINT('Ctrl Pts',(-2.8144471524083,5.53611316288752,2.89119454472736));
#56504=CARTESIAN_POINT('Ctrl Pts',(-6.17879030235427,0.626268413324878,
3.16956382045763));
#56505=CARTESIAN_POINT('Ctrl Pts',(-3.86805136883776,-4.85879000719604,
3.44793309618789));
#56506=CARTESIAN_POINT('Ctrl Pts',(1.9954071015175,-5.88115738823654,3.72630237191817));
#56507=CARTESIAN_POINT('Ctrl Pts',(6.02612833094048,-1.50181192731717,4.00467164764843));
#56508=CARTESIAN_POINT('Ctrl Pts',(4.52198411744087,4.25691453609398,4.28304092337871));
#56509=CARTESIAN_POINT('Ctrl Pts',(-1.13550238327193,6.10575925365384,4.56141019910898));
#56510=CARTESIAN_POINT('Ctrl Pts',(-5.75005508696296,2.3465992889471,4.83977947483924));
#56511=CARTESIAN_POINT('Ctrl Pts',(-5.0833095095791,-3.56786016483527,5.11814875056952));
#56512=CARTESIAN_POINT('Ctrl Pts',(0.252343298968592,-6.20531905589563,
5.39651802629978));
#56513=CARTESIAN_POINT('Ctrl Pts',(5.35622437473667,-3.14332979075887,5.67488730203006));
#56514=CARTESIAN_POINT('Ctrl Pts',(5.5405319585073,2.80573828835742,5.95325657776032));
#56515=CARTESIAN_POINT('Ctrl Pts',(0.635983615480163,6.17779787358219,6.23162585349059));
#56516=CARTESIAN_POINT('Ctrl Pts',(-4.85270159657326,3.87568689919748,6.50999512922086));
#56517=CARTESIAN_POINT('Ctrl Pts',(-5.88428783949522,-1.98615667759732,
6.78836440495113));
#56518=CARTESIAN_POINT('Ctrl Pts',(-1.51128599028987,-6.02375932300995,
7.06673368068139));
#56519=CARTESIAN_POINT('Ctrl Pts',(4.24979857847531,-4.52867240683016,7.34510295641167));
#56520=CARTESIAN_POINT('Ctrl Pts',(6.10753725090218,1.12589984227641,7.62347223214193));
#56521=CARTESIAN_POINT('Ctrl Pts',(2.35563818995783,5.74635801564849,7.9018415078722));
#56522=CARTESIAN_POINT('Ctrl Pts',(-3.55986239050335,5.08891358608843,8.18021078360247));
#56523=CARTESIAN_POINT('Ctrl Pts',(-6.20570818688168,-0.242585294825209,
8.45858005933274));
#56524=CARTESIAN_POINT('Ctrl Pts',(-3.15174841886823,-5.35127495370563,
8.73694933506301));
#56525=CARTESIAN_POINT('Ctrl Pts',(2.79702248664004,-5.54493705421672,9.01531861079328));
#56526=CARTESIAN_POINT('Ctrl Pts',(6.17679016915104,-0.645697245057467,
9.29368788652355));
#56527=CARTESIAN_POINT('Ctrl Pts',(3.88331284626025,4.84660118681802,9.57205716225382));
#56528=CARTESIAN_POINT('Ctrl Pts',(-1.97690134256598,5.88740374084846,9.85042643798408));
#56529=CARTESIAN_POINT('Ctrl Pts',(-6.02137542030695,1.52075631635018,10.1287957137144));
#56530=CARTESIAN_POINT('Ctrl Pts',(-4.53534949830443,-4.24267211250473,
10.4071649894446));
#56531=CARTESIAN_POINT('Ctrl Pts',(1.11629451730146,-6.10930014622284,10.6855342651749));
#56532=CARTESIAN_POINT('Ctrl Pts',(5.74264673548367,-2.36467126625128,10.9639035409052));
#56533=CARTESIAN_POINT('Ctrl Pts',(5.09450507939081,3.55185581380451,11.2422728166354));
#56534=CARTESIAN_POINT('Ctrl Pts',(-0.232826690848401,6.20608197319566,
11.5206420923657));
#56535=CARTESIAN_POINT('Ctrl Pts',(-5.34631230073448,3.16015925374197,11.799011368096));
#56536=CARTESIAN_POINT('Ctrl Pts',(-5.54932843912339,-2.78829976880751,
12.0773806438262));
#56537=CARTESIAN_POINT('Ctrl Pts',(-0.655409278038173,-6.17576719155257,
12.3557499195565));
#56538=CARTESIAN_POINT('Ctrl Pts',(4.84048879301466,-3.89092919116954,12.6341191952868));
#56539=CARTESIAN_POINT('Ctrl Pts',(5.89050508459169,1.96764111930887,12.912488471017));
#56540=CARTESIAN_POINT('Ctrl Pts',(1.53022288208102,6.01897662872612,13.1908577467473));
#56541=CARTESIAN_POINT('Ctrl Pts',(-4.23553515580366,4.54201537535343,13.4692270224776));
#56542=CARTESIAN_POINT('Ctrl Pts',(-6.11104793525676,-1.10668643209798,
13.7475962982079));
#56543=CARTESIAN_POINT('Ctrl Pts',(-2.37369849549166,-5.7389212556452,14.0259655739381));
#56544=CARTESIAN_POINT('Ctrl Pts',(3.54384045453631,-5.10008397566036,14.3043348496684));
#56545=CARTESIAN_POINT('Ctrl Pts',(6.20644041391337,0.223067511167865,14.5827041253987));
#56546=CARTESIAN_POINT('Ctrl Pts',(3.16856227458287,5.34133642809414,14.8610734011289));
#56547=CARTESIAN_POINT('Ctrl Pts',(-2.77957015642807,5.55370610236895,15.1394426768592));
#56548=CARTESIAN_POINT('Ctrl Pts',(-6.17472894331627,0.665119690407707,
15.4178119525895));
#56549=CARTESIAN_POINT('Ctrl Pts',(-3.89853591509276,-4.834364430277,15.6961812283197));
#56550=CARTESIAN_POINT('Ctrl Pts',(1.95837603072338,-5.89359186305633,15.97455050405));
#56551=CARTESIAN_POINT('Ctrl Pts',(6.01656295419885,-1.53968566407487,16.2529197797802));
#56552=CARTESIAN_POINT('Ctrl Pts',(4.54867002149468,4.22838772601937,16.5312890555106));
#56553=CARTESIAN_POINT('Ctrl Pts',(-1.0970756104234,6.11278061368228,16.8096583312408));
#56554=CARTESIAN_POINT('Ctrl Pts',(-5.73518158534497,2.38271985535767,17.0880276069711));
#56555=CARTESIAN_POINT('Ctrl Pts',(-5.10565026110237,-3.53581633251799,
17.3663968827013));
#56556=CARTESIAN_POINT('Ctrl Pts',(0.213307779914776,-6.20678350814845,
17.6447661584316));
#56557=CARTESIAN_POINT('Ctrl Pts',(5.33634734808843,-3.1769574606131,17.9231354341619));
#56558=CARTESIAN_POINT('Ctrl Pts',(5.55807003312879,2.77083367108736,18.2015047098922));
#56559=CARTESIAN_POINT('Ctrl Pts',(0.674828458155247,6.17367542700939,18.4798739856224));
#56560=CARTESIAN_POINT('Ctrl Pts',(-4.8282281137487,3.90613299922089,18.7582432613527));
#56561=CARTESIAN_POINT('Ctrl Pts',(-5.89666406860973,-1.9491060997192,19.0366125370829));
#56562=CARTESIAN_POINT('Ctrl Pts',(-1.5491446389332,-6.01413440269339,19.3149818128132));
#56563=CARTESIAN_POINT('Ctrl Pts',(4.22122984082524,-4.55531342027332,19.5933510885435));
#56564=CARTESIAN_POINT('Ctrl Pts',(6.11449817721499,1.08746207604232,19.8717203642738));
#56565=CARTESIAN_POINT('Ctrl Pts',(2.39173532354231,5.73142773382999,20.150089640004));
#56566=CARTESIAN_POINT('Ctrl Pts',(-3.52778346759073,5.11120392195315,20.4284589157343));
#56567=CARTESIAN_POINT('Ctrl Pts',(-6.20711125505255,-0.20354752122192,
20.7068281914646));
#56568=CARTESIAN_POINT('Ctrl Pts',(-3.18534479107406,-5.33134507305361,
20.9851974671948));
#56569=CARTESIAN_POINT('Ctrl Pts',(2.76209033438777,-5.56242022061237,21.2635667429251));
#56570=CARTESIAN_POINT('Ctrl Pts',(6.1726066452369,-0.684535557274347,21.5419360186554));
#56571=CARTESIAN_POINT('Ctrl Pts',(3.91372042476886,4.82207985860276,21.8203052943857));
#56572=CARTESIAN_POINT('Ctrl Pts',(-1.93983134921762,5.89972169365541,22.0986745701159));
#56573=CARTESIAN_POINT('Ctrl Pts',(-6.01169098021472,1.55859978326723,22.3770438458462));
#56574=CARTESIAN_POINT('Ctrl Pts',(-4.56194555526257,-4.21406151792019,
22.6554131215764));
#56575=CARTESIAN_POINT('Ctrl Pts',(1.07784585272568,-6.11620062160797,22.9337823973067));
#56576=CARTESIAN_POINT('Ctrl Pts',(5.72765971038225,-2.40074487775348,23.212151673037));
#56577=CARTESIAN_POINT('Ctrl Pts',(5.11674494448041,3.51974187961701,23.4905209487673));
#56578=CARTESIAN_POINT('Ctrl Pts',(-0.193786759222999,6.20742365381528,
23.7688902244975));
#56579=CARTESIAN_POINT('Ctrl Pts',(-5.32632961535865,3.19372424522674,24.0472595002278));
#56580=CARTESIAN_POINT('Ctrl Pts',(-5.56675665406317,-2.75334016794859,
24.3256287759581));
#56581=CARTESIAN_POINT('Ctrl Pts',(-0.694240963762592,-6.17152260064156,
24.6039980516883));
#56582=CARTESIAN_POINT('Ctrl Pts',(4.81591968004187,-3.92129817297552,24.8823673274186));
#56583=CARTESIAN_POINT('Ctrl Pts',(5.9027647306328,1.93055180215219,25.1607366031489));
#56584=CARTESIAN_POINT('Ctrl Pts',(1.56805107369734,6.00923269280466,25.4391058788792));
#56585=CARTESIAN_POINT('Ctrl Pts',(-4.20688277502926,4.56856641006321,25.7174751546094));
#56586=CARTESIAN_POINT('Ctrl Pts',(-6.1178879426516,-1.06822696425142,25.9958444303397));
#56587=CARTESIAN_POINT('Ctrl Pts',(-2.40974849571335,-5.72387752431889,
26.27421370607));
#56588=CARTESIAN_POINT('Ctrl Pts',(3.51169158848119,-5.12227331498293,26.5525829818002));
#56589=CARTESIAN_POINT('Ctrl Pts',(6.20772070366418,0.18402551805332,26.8309522575305));
#56590=CARTESIAN_POINT('Ctrl Pts',(3.20209580235133,5.32130098740521,27.1093215332608));
#56591=CARTESIAN_POINT('Ctrl Pts',(-2.74458319340624,5.57107932275853,27.387690808991));
#56592=CARTESIAN_POINT('Ctrl Pts',(-6.17042329590389,0.703944653621518,
27.6660600847213));
#56593=CARTESIAN_POINT('Ctrl Pts',(-3.92886622510352,-4.80974759329806,
27.9444293604515));
#56594=CARTESIAN_POINT('Ctrl Pts',(1.92126748146815,-5.90579317201751,28.2227986361818));
#56595=CARTESIAN_POINT('Ctrl Pts',(6.00675954654171,-1.57749848685371,28.5011679119121));
#56596=CARTESIAN_POINT('Ctrl Pts',(4.57517596830407,4.19969362990309,28.7795371876424));
#56597=CARTESIAN_POINT('Ctrl Pts',(-1.05860543440373,6.11956013617373,29.0579064633726));
#56598=CARTESIAN_POINT('Ctrl Pts',(-5.72008118499199,2.41874615515898,29.3362757391029));
#56599=CARTESIAN_POINT('Ctrl Pts',(-5.12778901979094,-3.50363261408887,
29.6146450148332));
#56600=CARTESIAN_POINT('Ctrl Pts',(0.1742638218492,-6.20800240386472,29.8930142905635));
#56601=CARTESIAN_POINT('Ctrl Pts',(5.31625920162736,-3.21045944174788,30.1713835662937));
#56602=CARTESIAN_POINT('Ctrl Pts',(5.57538821600995,2.73581943241381,30.449752842024));
#56603=CARTESIAN_POINT('Ctrl Pts',(0.713646602857252,6.16930873374205,30.7281221177543));
#56604=CARTESIAN_POINT('Ctrl Pts',(-4.80356361363291,3.93642456243958,31.0064913934845));
#56605=CARTESIAN_POINT('Ctrl Pts',(-5.90880701032121,-1.91197841012251,
31.2848606692148));
#56606=CARTESIAN_POINT('Ctrl Pts',(-1.58694199937596,-6.00427154754116,
31.563229944945));
#56607=CARTESIAN_POINT('Ctrl Pts',(4.19249410031801,-4.58177421364196,31.8415992206754));
#56608=CARTESIAN_POINT('Ctrl Pts',(6.12121719803953,1.04898128697357,32.1199684964056));
#56609=CARTESIAN_POINT('Ctrl Pts',(2.42773783384219,5.71627070178861,32.3983377721359));
#56610=CARTESIAN_POINT('Ctrl Pts',(-3.49556497636723,5.1332920452659,32.6767070478661));
#56611=CARTESIAN_POINT('Ctrl Pts',(-6.20826875372037,-0.164501694747944,
32.9550763235964));
#56612=CARTESIAN_POINT('Ctrl Pts',(-3.21881514273589,-5.31120427049176,
33.2334455993267));
#56613=CARTESIAN_POINT('Ctrl Pts',(2.72704890664107,-5.57968332316301,33.511814875057));
#56614=CARTESIAN_POINT('Ctrl Pts',(6.16817891691201,-0.723346787480091,
33.7901841507872));
#56615=CARTESIAN_POINT('Ctrl Pts',(3.94397316629452,4.79736775633728,34.0685534265175));
#56616=CARTESIAN_POINT('Ctrl Pts',(-1.90268461108404,5.91180623809167,34.3469227022477));
#56617=CARTESIAN_POINT('Ctrl Pts',(-6.00176870195498,1.59638158791352,34.6252919779781));
#56618=CARTESIAN_POINT('Ctrl Pts',(-4.58836112976159,-4.18528420407607,
34.9036612537083));
#56619=CARTESIAN_POINT('Ctrl Pts',(1.03935454575815,-6.12285912415169,35.1820305294386));
#56620=CARTESIAN_POINT('Ctrl Pts',(5.71244608413083,-2.43672350952955,35.4603998051688));
#56621=CARTESIAN_POINT('Ctrl Pts',(5.13878237780069,3.48748869526495,35.7387690808992));
#56622=CARTESIAN_POINT('Ctrl Pts',(-0.15473916088826,6.20851975257254,36.0171383566293));
#56623=CARTESIAN_POINT('Ctrl Pts',(-5.30613620649767,3.22716288465429,36.2955076323597));
#56624=CARTESIAN_POINT('Ctrl Pts',(-5.58396463359725,-2.71827163777478,
36.5738769080898));
#56625=CARTESIAN_POINT('Ctrl Pts',(-0.733045183504503,-6.16703384820746,
36.8522461838203));
#56626=CARTESIAN_POINT('Ctrl Pts',(4.79116003673157,-3.95151201800298,37.1306154595503));
#56627=CARTESIAN_POINT('Ctrl Pts',(5.91479084791276,1.89338610733341,37.4089847352808));
#56628=CARTESIAN_POINT('Ctrl Pts',(1.60581722912522,5.99925101597193,37.6873540110109));
#56629=CARTESIAN_POINT('Ctrl Pts',(-4.17806395900508,4.59493670037558,37.9657232867413));
#56630=CARTESIAN_POINT('Ctrl Pts',(-6.12448591045022,-1.02972523456137,
38.2440925624714));
#56631=CARTESIAN_POINT('Ctrl Pts',(-2.44570316000227,-5.70860734147573,
38.5224618382019));
#56632=CARTESIAN_POINT('Ctrl Pts',(3.47940379075197,-5.14426000381944,38.800831113932));
#56633=CARTESIAN_POINT('Ctrl Pts',(6.20875539980056,0.144976244409641,39.0792003896624));
#56634=CARTESIAN_POINT('Ctrl Pts',(3.23550264686201,5.30105502217667,39.3575696653926));
#56635=CARTESIAN_POINT('Ctrl Pts',(-2.70948764751817,5.58823213672641,39.6359389411229));
#56636=CARTESIAN_POINT('Ctrl Pts',(-6.16587353045974,0.74274176694977,39.9143082168531));
#56637=CARTESIAN_POINT('Ctrl Pts',(-3.95904109892399,-4.78494047016537,
40.1926774925834));
#56638=CARTESIAN_POINT('Ctrl Pts',(1.88408292186256,-5.91776083240456,40.4710467683136));
#56639=CARTESIAN_POINT('Ctrl Pts',(5.99671849581738,-1.61524889967998,40.7494160440439));
#56640=CARTESIAN_POINT('Ctrl Pts',(4.60150090922485,4.1708333829582,41.0277853197742));
#56641=CARTESIAN_POINT('Ctrl Pts',(-1.02009337719325,6.12609755291264,41.3061545955045));
#56642=CARTESIAN_POINT('Ctrl Pts',(-5.70475448331516,2.45467676305686,41.5845238712348));
#56643=CARTESIAN_POINT('Ctrl Pts',(-5.14972490977789,-3.47131028281956,
41.862893146965));
#56644=CARTESIAN_POINT('Ctrl Pts',(0.135212969452428,-6.20897569482178,
42.1412624226953));
#56645=CARTESIAN_POINT('Ctrl Pts',(5.29596073009285,-3.2438344087376,42.4196316984255));
#56646=CARTESIAN_POINT('Ctrl Pts',(5.59248582199842,2.70069695759119,42.6980009741559));
#56647=CARTESIAN_POINT('Ctrl Pts',(0.752436513839245,6.16469796653795,42.9763702498861));
#56648=CARTESIAN_POINT('Ctrl Pts',(-4.77870907201771,3.96656039044047,43.2547395256164));
#56649=CARTESIAN_POINT('Ctrl Pts',(-5.92071618422324,-1.87477507767536,
43.5331088013466));
#56650=CARTESIAN_POINT('Ctrl Pts',(-1.6246765762562,-5.99417114775347,43.8114780770769));
#56651=CARTESIAN_POINT('Ctrl Pts',(4.16359249381437,-4.60805374007816,44.0898473528071));
#56652=CARTESIAN_POINT('Ctrl Pts',(6.12769404755385,1.01045899747034,44.3682166285375));
#56653=CARTESIAN_POINT('Ctrl Pts',(2.46364429650437,5.70088751917604,44.6465859042677));
#56654=CARTESIAN_POINT('Ctrl Pts',(-3.46320819148043,5.15517708216299,44.9249551799981));
#56655=CARTESIAN_POINT('Ctrl Pts',(-6.20918063709147,-0.12544936015814,
45.2033244557282));
#56656=CARTESIAN_POINT('Ctrl Pts',(-3.25215814967919,-5.29085334284281,
45.4816937314586));
#56657=CARTESIAN_POINT('Ctrl Pts',(2.69189958973031,-5.59672567889524,45.7600630071887));
#56658=CARTESIAN_POINT('Ctrl Pts',(6.16350715934888,-0.762129400201062,
46.0384322829191));
#56659=CARTESIAN_POINT('Ctrl Pts',(3.97406987395981,4.7724658576967,46.3168015586493));
#56660=CARTESIAN_POINT('Ctrl Pts',(-1.86546259778696,5.92365689606119,46.5951708343796));
#56661=CARTESIAN_POINT('Ctrl Pts',(-5.99160897807888,1.63410023554255,46.8735401101098));
#56662=CARTESIAN_POINT('Ctrl Pts',(-4.6145951767326,-4.15634130947783,47.1519093858402));
#56663=CARTESIAN_POINT('Ctrl Pts',(1.0008221192151,-6.12927539042631,47.4302786615703));
#56664=CARTESIAN_POINT('Ctrl Pts',(5.69700645862006,-2.47260573817116,47.7086479373007));
#56665=CARTESIAN_POINT('Ctrl Pts',(5.16061650749346,3.4550975367682,47.9870172130309));
#56666=CARTESIAN_POINT('Ctrl Pts',(-0.115685440668852,6.20937022610289,
48.2653864887612));
#56667=CARTESIAN_POINT('Ctrl Pts',(-5.28573287305531,3.26047384910508,48.5437557644915));
#56668=CARTESIAN_POINT('Ctrl Pts',(-5.60095169693318,-2.68309556568845,
48.8221250402218));
#56669=CARTESIAN_POINT('Ctrl Pts',(-0.771820402068029,-6.16230111183698,
49.100494315952));
#56670=CARTESIAN_POINT('Ctrl Pts',(4.76621084263973,-3.98156953091355,49.3788635916823));
#56671=CARTESIAN_POINT('Ctrl Pts',(5.92658296064706,1.8561455052241,49.6572328674126));
#56672=CARTESIAN_POINT('Ctrl Pts',(1.64351985423726,5.98903199312908,49.9356021431428));
#56673=CARTESIAN_POINT('Ctrl Pts',(-4.1490798478785,4.62112520301324,50.2139714188731));
#56674=CARTESIAN_POINT('Ctrl Pts',(-6.13084157761981,-0.991182766256508,
50.4923406946034));
#56675=CARTESIAN_POINT('Ctrl Pts',(-2.4815610658984,-5.69311131124387,50.7707099703336));
#56676=CARTESIAN_POINT('Ctrl Pts',(3.44697833873802,-5.16604317231927,51.0490792460639));
#56677=CARTESIAN_POINT('Ctrl Pts',(6.20954446138722,0.105921235127679,51.3274485217941));
#56678=CARTESIAN_POINT('Ctrl Pts',(3.26878148645317,5.28059933339168,51.6058177975245));
#56679=CARTESIAN_POINT('Ctrl Pts',(-2.67428490723522,5.60516386566259,51.8841870732547));
#56680=CARTESIAN_POINT('Ctrl Pts',(-6.16107982698442,0.78150949547734,52.162556348985));
#56681=CARTESIAN_POINT('Ctrl Pts',(-3.98905934275737,-4.75994404231351,
52.4409256247152));
#56682=CARTESIAN_POINT('Ctrl Pts',(1.84682382302487,-5.92949437074557,52.7192949004455));
#56683=CARTESIAN_POINT('Ctrl Pts',(5.98644019927607,-1.65293540904875,52.9976641761758));
#56684=CARTESIAN_POINT('Ctrl Pts',(4.62764380277359,4.14180812697147,53.2760334519061));
#56685=CARTESIAN_POINT('Ctrl Pts',(-0.981540962429502,6.13239260526172,
53.5544027276362));
#56686=CARTESIAN_POINT('Ctrl Pts',(-5.68920208667882,2.49051025754264,53.8327720033667));
#56687=CARTESIAN_POINT('Ctrl Pts',(-5.17145706322212,-3.43885061746587,
54.1111412790968));
#56688=CARTESIAN_POINT('Ctrl Pts',(0.0961567676780714,-6.20970334251366,
54.3895105548272));
#56689=CARTESIAN_POINT('Ctrl Pts',(5.27545273654541,-3.2770810411815,54.6678798305573));
#56690=CARTESIAN_POINT('Ctrl Pts',(5.60936217466827,2.66546763615629,54.9462491062877));
#56691=CARTESIAN_POINT('Ctrl Pts',(0.791196656471176,6.15984330781104,55.2246183820179));
#56692=CARTESIAN_POINT('Ctrl Pts',(-4.75366547221362,3.9965392909716,55.5029876577482));
#56693=CARTESIAN_POINT('Ctrl Pts',(-5.93239111915783,-1.83749757423864,
55.7813569334784));
#56694=CARTESIAN_POINT('Ctrl Pts',(-1.66234687669558,-5.98383360292849,
56.0597262092088));
#56695=CARTESIAN_POINT('Ctrl Pts',(4.13452616473729,-4.6341509598953,56.338095484939));
#56696=CARTESIAN_POINT('Ctrl Pts',(6.13392846951687,0.971896731574924,56.6164647606693));
#56697=CARTESIAN_POINT('Ctrl Pts',(2.4994532909755,5.68527879459112,56.8948340363995));
#56698=CARTESIAN_POINT('Ctrl Pts',(-3.43071439304901,5.17685816681528,57.1732033121299));
#56699=CARTESIAN_POINT('Ctrl Pts',(-6.20984686908935,-0.0863920624645414,
57.4515725878601));
#56700=CARTESIAN_POINT('Ctrl Pts',(-3.2853724927679,-5.27029309524236,57.7299418635904));
#56701=CARTESIAN_POINT('Ctrl Pts',(2.65664377425388,-5.61354661356913,58.0083111393206));
#56702=CARTESIAN_POINT('Ctrl Pts',(6.15859155737437,-0.800881861096334,
58.2866804150509));
#56703=CARTESIAN_POINT('Ctrl Pts',(4.00400935706071,4.74737514786502,58.5650496907811));
#56704=CARTESIAN_POINT('Ctrl Pts',(-1.82816678192627,5.93527319872107,58.8434189665115));
#56705=CARTESIAN_POINT('Ctrl Pts',(-5.98121221053155,1.67175423390625,59.1217882422417));
#56706=CARTESIAN_POINT('Ctrl Pts',(-4.64064665828831,-4.1272339791819,59.400157517972));
#56707=CARTESIAN_POINT('Ctrl Pts',(0.962250097539924,-6.1354491665876,59.6785267937022));
#56708=CARTESIAN_POINT('Ctrl Pts',(5.6813414446818,-2.50839014408368,59.9568960694325));
#56709=CARTESIAN_POINT('Ctrl Pts',(5.18224646974358,3.42256968560548,60.2352653451627));
#56710=CARTESIAN_POINT('Ctrl Pts',(-0.0766271436318026,6.20997504075942,
60.5136346208931));
#56711=CARTESIAN_POINT('Ctrl Pts',(-5.26512042224072,3.29365582071042,60.7920038966233));
#56712=CARTESIAN_POINT('Ctrl Pts',(-5.61771717201837,-2.6478133433468,61.0703731723536));
#56713=CARTESIAN_POINT('Ctrl Pts',(-0.810565085404379,-6.15732457876948,
61.3487424480839));
#56714=CARTESIAN_POINT('Ctrl Pts',(4.74107308482143,-4.01146952255369,61.627111723814));
#56715=CARTESIAN_POINT('Ctrl Pts',(5.93814060230899,1.81883146915945,61.9054809995444));
#56716=CARTESIAN_POINT('Ctrl Pts',(1.68115745741945,5.97857602856726,62.1838502752747));
#56717=CARTESIAN_POINT('Ctrl Pts',(-4.11993158833646,4.64713088189084,62.4622195510049));
#56718=CARTESIAN_POINT('Ctrl Pts',(-6.1369546927136,-0.952601084177306,
62.7405888267352));
#56719=CARTESIAN_POINT('Ctrl Pts',(-2.51732079476958,-5.67739004668659,
63.0189581024655));
#56720=CARTESIAN_POINT('Ctrl Pts',(3.41441651527462,-5.18762195868357,63.2973273781957));
#56721=CARTESIAN_POINT('Ctrl Pts',(6.21008785720687,0.0668620353253585,
63.575696653926));
#56722=CARTESIAN_POINT('Ctrl Pts',(3.30193100452715,5.25993473033056,63.8540659296562));
#56723=CARTESIAN_POINT('Ctrl Pts',(-2.63897636526924,5.62187383970377,64.1324352053865));
#56724=CARTESIAN_POINT('Ctrl Pts',(-6.15604237512935,0.820246305452156,
64.4108044811168));
#56725=CARTESIAN_POINT('Ctrl Pts',(-4.01891976900398,-4.7347592986661,64.6891737568471));
#56726=CARTESIAN_POINT('Ctrl Pts',(1.80949165902193,-5.94099332283124,64.9675430325774));
#56727=CARTESIAN_POINT('Ctrl Pts',(5.97592506355382,-1.69055652398388,65.2459123083075));
#56728=CARTESIAN_POINT('Ctrl Pts',(4.65360361466952,4.11261901025744,65.524281584038));
#56729=CARTESIAN_POINT('Ctrl Pts',(-0.942949715346173,6.1384450441724,65.802650859768));
#56730=CARTESIAN_POINT('Ctrl Pts',(-5.67342461037618,2.52624522095008,66.0810201354985));
#56731=CARTESIAN_POINT('Ctrl Pts',(-5.1929846203432,-3.40625490221655,66.3593894112286));
#56732=CARTESIAN_POINT('Ctrl Pts',(0.0570967616911944,-6.21018531815279,
66.6377586869591));
#56733=CARTESIAN_POINT('Ctrl Pts',(5.25473603233471,-3.31019802375619,66.9161279626891));
#56734=CARTESIAN_POINT('Ctrl Pts',(5.62601660634699,2.6301328618728,67.1944972384196));
#56735=CARTESIAN_POINT('Ctrl Pts',(0.829925497300859,6.15474494962425,67.4728665141497));
#56736=CARTESIAN_POINT('Ctrl Pts',(-4.72843380501069,4.02636007798958,67.7512357898801));
#56737=CARTESIAN_POINT('Ctrl Pts',(-5.94383135323418,-1.80014737460753,
68.0296050656102));
#56738=CARTESIAN_POINT('Ctrl Pts',(-1.69995141035886,-5.9732593220464,68.3079743413406));
#56739=CARTESIAN_POINT('Ctrl Pts',(4.10529626302638,-4.66006484061938,68.5863436170708));
#56740=CARTESIAN_POINT('Ctrl Pts',(6.13992021727863,0.933296014910856,68.8647128928011));
#56741=CARTESIAN_POINT('Ctrl Pts',(2.53516340055861,5.66944514555562,69.1430821685314));
#56742=CARTESIAN_POINT('Ctrl Pts',(-3.39808486661228,5.19833444146264,69.4214514442617));
#56743=CARTESIAN_POINT('Ctrl Pts',(-6.21026742335611,-0.047331346875596,
69.6998207199918));
#56744=CARTESIAN_POINT('Ctrl Pts',(-3.31845685795602,-5.24952434110749,
69.9781899957223));
#56745=CARTESIAN_POINT('Ctrl Pts',(2.621282855024,-5.63014546170463,70.2565592714524));
#56746=CARTESIAN_POINT('Ctrl Pts',(6.15343230546253,-0.839602637017208,
70.5349285471828));
#56747=CARTESIAN_POINT('Ctrl Pts',(4.03379043111301,4.72209661949609,70.813297822913));
#56748=CARTESIAN_POINT('Ctrl Pts',(-1.79079863902149,5.94665468650014,71.0916670986432));
#56749=CARTESIAN_POINT('Ctrl Pts',(-5.97057881063638,1.70934209331426,71.3700363743736));
#56750=CARTESIAN_POINT('Ctrl Pts',(-4.66651454376411,-4.09796336475011,
71.6484056501037));
#56751=CARTESIAN_POINT('Ctrl Pts',(0.923640006742209,-6.1413802083848,71.9267749258341));
#56752=CARTESIAN_POINT('Ctrl Pts',(5.66545166206479,-2.544075311543,72.2051442015643));
#56753=CARTESIAN_POINT('Ctrl Pts',(5.20367140881343,3.38990642866345,72.4835134772947));
#56754=CARTESIAN_POINT('Ctrl Pts',(-0.0375658150251663,6.21033417261403,
72.7618827530248));
#56755=CARTESIAN_POINT('Ctrl Pts',(-5.24429966953607,3.32670748670501,73.0402520287552));
#56756=CARTESIAN_POINT('Ctrl Pts',(-5.63426039556707,-2.61242636660629,
73.3186213044854));
#56757=CARTESIAN_POINT('Ctrl Pts',(-0.849277700672862,-6.15210444588971,
73.5969905802157));
#56758=CARTESIAN_POINT('Ctrl Pts',(4.71574775779221,-4.0412108100016,73.8753598559459));
#56759=CARTESIAN_POINT('Ctrl Pts',(5.94946331564799,1.78144547538063,74.1537291316763));
#56760=CARTESIAN_POINT('Ctrl Pts',(1.71872854962958,5.96788353595171,74.4320984074064));
#56761=CARTESIAN_POINT('Ctrl Pts',(-4.09062033356033,4.67295270815561,74.7104676831368));
#56762=CARTESIAN_POINT('Ctrl Pts',(-6.1428250138809,-0.913981714715994,
74.9888369588671));
#56763=CARTESIAN_POINT('Ctrl Pts',(-2.55298093186715,-5.66144416977842,
75.2672062345973));
#56764=CARTESIAN_POINT('Ctrl Pts',(3.38171960859274,-5.20899550919893,75.5455755103276));
#56765=CARTESIAN_POINT('Ctrl Pts',(6.21038556576122,0.0278001902866955,
75.8239447860578));
#56766=CARTESIAN_POINT('Ctrl Pts',(3.33494988960255,5.23906203053906,76.1023140617882));
#56767=CARTESIAN_POINT('Ctrl Pts',(-2.60356341851882,5.6383613977597,76.3806833375183));
#56768=CARTESIAN_POINT('Ctrl Pts',(-6.15076137418917,0.858950664344476,
76.6590526132487));
#56769=CARTESIAN_POINT('Ctrl Pts',(-4.04862119630716,-4.7093872355974,76.9374218889788));
#56770=CARTESIAN_POINT('Ctrl Pts',(1.77208790681172,-5.95225723373308,77.2157911647093));
#56771=CARTESIAN_POINT('Ctrl Pts',(5.96517350465712,-1.72811075609542,77.4941604404393));
#56772=CARTESIAN_POINT('Ctrl Pts',(4.67937931787436,4.08326718761399,77.7725297161699));
#56773=CARTESIAN_POINT('Ctrl Pts',(-0.904321162713915,6.14425463019421,
78.0508989918999));
#56774=CARTESIAN_POINT('Ctrl Pts',(-5.65742267860557,2.56188023951072,78.3292682676303));
#56775=CARTESIAN_POINT('Ctrl Pts',(-5.21430672945461,-3.37352442664352,
78.6076375433605));
#56776=CARTESIAN_POINT('Ctrl Pts',(0.0180344968077807,-6.2104216026708,
78.8860068190908));
#56777=CARTESIAN_POINT('Ctrl Pts',(5.23381143706748,-3.34318404626741,79.164376094821));
#56778=CARTESIAN_POINT('Ctrl Pts',(5.64244845814195,2.59469403267662,79.4427453705514));
#56779=CARTESIAN_POINT('Ctrl Pts',(0.868621504114074,6.14940309368207,79.7211146462815));
#56780=CARTESIAN_POINT('Ctrl Pts',(-4.70301506863955,4.05602157170603,79.999483922012));
#56781=CARTESIAN_POINT('Ctrl Pts',(-5.95503643384666,-1.76272595645327,
80.277853197742));
#56782=CARTESIAN_POINT('Ctrl Pts',(-1.73748868951266,-5.96244872345345,
80.5562224734725));
#56783=CARTESIAN_POINT('Ctrl Pts',(4.0759039450931,-4.68579435702962,80.8345917492026));
#56784=CARTESIAN_POINT('Ctrl Pts',(6.1456690537899,0.894658374623772,81.112961024933));
#56785=CARTESIAN_POINT('Ctrl Pts',(2.5707732124682,5.65338719849006,81.3913303006631));
#56786=CARTESIAN_POINT('Ctrl Pts',(-3.36532090307962,5.21960505644742,81.6696995763936));
#56787=CARTESIAN_POINT('Ctrl Pts',(-6.21044228325367,-0.00826875873537722,
81.9480688521236));
#56788=CARTESIAN_POINT('Ctrl Pts',(-3.35140993633938,-5.22854790210446,
82.2264381278542));
#56789=CARTESIAN_POINT('Ctrl Pts',(2.58581823101083,-5.64652156660783,82.5048074035842));
#56790=CARTESIAN_POINT('Ctrl Pts',(6.14802960772673,-0.878290196068972,
82.7831766793146));
#56791=CARTESIAN_POINT('Ctrl Pts',(4.06341191789994,4.69663127267458,83.0615459550448));
#56792=CARTESIAN_POINT('Ctrl Pts',(-1.75335964745426,5.95780090911698,83.3399152307751));
#56793=CARTESIAN_POINT('Ctrl Pts',(-5.95970919907819,1.74686232669266,83.6182845065053));
#56794=CARTESIAN_POINT('Ctrl Pts',(-4.69219780975906,-4.06853062420423,
83.8966537822357));
#56795=CARTESIAN_POINT('Ctrl Pts',(0.884993374337941,-6.14706828117063,
84.1750230579659));
#56796=CARTESIAN_POINT('Ctrl Pts',(5.64933773941046,-2.57965982875044,84.4533923336961));
#56797=CARTESIAN_POINT('Ctrl Pts',(5.22489047707629,3.35710905818575,84.7317616094266));
#56798=CARTESIAN_POINT('Ctrl Pts',(0.00149699978309382,6.2104476074585,
85.0101308851566));
#56799=CARTESIAN_POINT('Ctrl Pts',(-5.2232714386648,3.35962753947885,85.288500160887));
#56800=CARTESIAN_POINT('Ctrl Pts',(-5.65058071308607,-2.57693603546843,
85.5668694366171));
#56801=CARTESIAN_POINT('Ctrl Pts',(-0.887956716301287,-6.14664091971955,
85.8452387123476));
#56802=CARTESIAN_POINT('Ctrl Pts',(4.69023586348765,-4.07079221661454,86.1236079880777));
#56803=CARTESIAN_POINT('Ctrl Pts',(5.96055065270824,1.74398900297437,86.4019772638081));
#56804=CARTESIAN_POINT('Ctrl Pts',(1.75623164445764,5.95695493830545,86.6803465395383));
#56805=CARTESIAN_POINT('Ctrl Pts',(-4.06114724317963,4.69858966022888,86.9587158152687));
#56806=CARTESIAN_POINT('Ctrl Pts',(-6.14845230887633,-0.87532618575515,
87.2370850909987));
#56807=CARTESIAN_POINT('Ctrl Pts',(-2.58854006638374,-5.64527431137958,
87.5154543667293));
#56808=CARTESIAN_POINT('Ctrl Pts',(3.34888891226714,-5.23016297827231,87.7938236424592));
#56809=CARTESIAN_POINT('Ctrl Pts',(6.2104375752723,-0.0112627545997063,
88.0721929181899));
#56810=CARTESIAN_POINT('Ctrl Pts',(3.36783683536597,5.21798205979547,88.3505621939197));
#56811=CARTESIAN_POINT('Ctrl Pts',(-2.56804746801205,5.6546258875396,88.6289314696503));
#56812=CARTESIAN_POINT('Ctrl Pts',(-6.14523703309425,0.897621040909271,
88.9073007453804));
#56813=CARTESIAN_POINT('Ctrl Pts',(-4.07816244960097,-4.6838288568926,89.1856700211108));
#56814=CARTESIAN_POINT('Ctrl Pts',(1.73461404618421,-5.96328565782118,89.464039296841));
#56815=CARTESIAN_POINT('Ctrl Pts',(5.95418594794534,-1.7655966196404,89.7424085725712));
#56816=CARTESIAN_POINT('Ctrl Pts',(4.70496989263451,4.05375382027557,90.0207778483016));
#56817=CARTESIAN_POINT('Ctrl Pts',(-0.865656832779086,6.14982113348502,
90.2991471240318));
#56818=CARTESIAN_POINT('Ctrl Pts',(-5.64119692444495,2.5974139034101,90.5775163997621));
#56819=CARTESIAN_POINT('Ctrl Pts',(-5.23542254699819,-3.34066048564925,
90.8558856754923));
#56820=CARTESIAN_POINT('Ctrl Pts',(-0.0210284815675073,-6.2104121867199,
91.1342549512226));
#56821=CARTESIAN_POINT('Ctrl Pts',(5.21267977857556,-3.37603780370208,91.4126242269529));
#56822=CARTESIAN_POINT('Ctrl Pts',(5.65865707996597,2.55915255062027,91.6909935026832));
#56823=CARTESIAN_POINT('Ctrl Pts',(0.907283145996256,6.14381795132199,91.9693627784133));
#56824=CARTESIAN_POINT('Ctrl Pts',(-4.67741026873163,4.08552259863533,92.2477320541438));
#56825=CARTESIAN_POINT('Ctrl Pts',(-5.96600591769324,-1.72523480026497,
92.5261013298739));
#56826=CARTESIAN_POINT('Ctrl Pts',(-1.77495722908411,-5.95140223484494,
92.8044706056043));
#56827=CARTESIAN_POINT('Ctrl Pts',(4.04635037377374,-4.71133849119933,93.0828398813344));
#56828=CARTESIAN_POINT('Ctrl Pts',(6.15117475161187,0.855985339318785,93.3612091570649));
#56829=CARTESIAN_POINT('Ctrl Pts',(2.60628131788759,5.63710558868877,93.6395784327949));
#56830=CARTESIAN_POINT('Ctrl Pts',(-3.33242379867873,5.24066917024868,93.9179477085254));
#56831=CARTESIAN_POINT('Ctrl Pts',(-6.21037144186387,0.0307941565386455,
94.1963169842555));
#56832=CARTESIAN_POINT('Ctrl Pts',(-3.38423042420886,-5.20736460811563,
94.4746862599858));
#56833=CARTESIAN_POINT('Ctrl Pts',(2.55025130528732,-5.6626742803976,94.7530555357162));
#56834=CARTESIAN_POINT('Ctrl Pts',(6.14238367791196,-0.91694300767064,95.0314248114463));
#56835=CARTESIAN_POINT('Ctrl Pts',(4.09287264551796,4.6709801148759,95.3097940871767));
#56836=CARTESIAN_POINT('Ctrl Pts',(-1.71585128840834,5.96871142559795,95.5881633629069));
#56837=CARTESIAN_POINT('Ctrl Pts',(-5.94860380588736,1.78431344964343,95.8665326386373));
#56838=CARTESIAN_POINT('Ctrl Pts',(-4.71769544017605,-4.03893692198051,
96.1449019143674));
#56839=CARTESIAN_POINT('Ctrl Pts',(0.84631172928875,-6.15251315990983,96.4232711900978));
#56840=CARTESIAN_POINT('Ctrl Pts',(5.63300031422728,-2.61514228789002,96.7016404658279));
#56841=CARTESIAN_POINT('Ctrl Pts',(5.24590283505089,3.32417887172173,96.9800097415584));
#56842=CARTESIAN_POINT('Ctrl Pts',(0.0405597553659755,6.21031534080523,
97.2583790172885));
#56843=CARTESIAN_POINT('Ctrl Pts',(-5.20203656155841,3.39241467662855,97.5367482930187));
#56844=CARTESIAN_POINT('Ctrl Pts',(-5.66667747890107,-2.54134375402281,
97.8151175687492));
#56845=CARTESIAN_POINT('Ctrl Pts',(-0.9266006020473,-6.14093421641053,98.0934868444793));
#56846=CARTESIAN_POINT('Ctrl Pts',(4.66453841122517,-4.1002125720749,98.3718561202097));
#56847=CARTESIAN_POINT('Ctrl Pts',(5.97140217484545,1.70646353381673,98.6502253959399));
#56848=CARTESIAN_POINT('Ctrl Pts',(1.79366525818349,5.945790667992,98.9285946716701));
#56849=CARTESIAN_POINT('Ctrl Pts',(-4.03151348322664,4.72404072384627,99.2069639474005));
#56850=CARTESIAN_POINT('Ctrl Pts',(-6.15383635506962,-0.836636026608615,
99.4853332231307));
#56851=CARTESIAN_POINT('Ctrl Pts',(-2.62399679150684,-5.62888111121181,
99.7637024988609));
#56852=CARTESIAN_POINT('Ctrl Pts',(3.31592572516549,-5.25112352846331,100.042071774591));
#56853=CARTESIAN_POINT('Ctrl Pts',(6.21024388368248,-0.0503252539024463,
100.320441050321));
#56854=CARTESIAN_POINT('Ctrl Pts',(3.40059054072436,5.19669565207855,100.598810326052));
#56855=CARTESIAN_POINT('Ctrl Pts',(-2.53242991885262,5.67066666557781,100.877179601782));
#56856=CARTESIAN_POINT('Ctrl Pts',(-6.13946957040164,0.936255905245747,
101.155548877512));
#56857=CARTESIAN_POINT('Ctrl Pts',(-4.10754236015684,-4.65808517370746,
101.433918153243));
#56858=CARTESIAN_POINT('Ctrl Pts',(1.69707155970298,-5.97407815878261,101.712287428973));
#56859=CARTESIAN_POINT('Ctrl Pts',(5.94296282811514,-1.80301263158,101.990656704703));
#56860=CARTESIAN_POINT('Ctrl Pts',(4.73037432651978,4.024080075868,102.269025980433));
#56861=CARTESIAN_POINT('Ctrl Pts',(-0.826958255203146,6.15514433381927,
102.547395256164));
#56862=CARTESIAN_POINT('Ctrl Pts',(-5.62474798982763,2.63284480684413,102.825764531894));
#56863=CARTESIAN_POINT('Ctrl Pts',(-5.25633123757708,-3.3076643794174,103.104133807624));
#56864=CARTESIAN_POINT('Ctrl Pts',(-0.0600906280010852,-6.21015707067235,
103.382503083354));
#56865=CARTESIAN_POINT('Ctrl Pts',(5.19134189288205,-3.40875799628004,103.660872359085));
#56866=CARTESIAN_POINT('Ctrl Pts',(5.67464183056409,2.52350982181727,103.939241634815));
#56867=CARTESIAN_POINT('Ctrl Pts',(0.945908893391775,6.13798974350711,104.217610910545));
#56868=CARTESIAN_POINT('Ctrl Pts',(-4.65162041827958,4.11486199163955,104.495980186275));
#56869=CARTESIAN_POINT('Ctrl Pts',(-5.97673937079238,-1.68767538929013,
104.774349462006));
#56870=CARTESIAN_POINT('Ctrl Pts',(-1.81235554672049,-5.94012029324891,
105.052718737736));
#56871=CARTESIAN_POINT('Ctrl Pts',(4.01663671828505,-4.73669623253596,105.331088013466));
#56872=CARTESIAN_POINT('Ctrl Pts',(6.15643709292455,0.817278439002367,105.609457289197));
#56873=CARTESIAN_POINT('Ctrl Pts',(2.64168631202361,5.6206009602944,105.887826564927));
#56874=CARTESIAN_POINT('Ctrl Pts',(-3.29939485490473,5.26152594951544,106.166195840657));
#56875=CARTESIAN_POINT('Ctrl Pts',(-6.21005490198965,0.0698558535153989,
106.444565116388));
#56876=CARTESIAN_POINT('Ctrl Pts',(-3.41691702309993,-5.18597529720738,
106.722934392118));
#56877=CARTESIAN_POINT('Ctrl Pts',(2.51458348497352,-5.67860296403031,107.001303667848));
#56878=CARTESIAN_POINT('Ctrl Pts',(6.13649473938585,-0.955559542616737,
107.279672943578));
#56879=CARTESIAN_POINT('Ctrl Pts',(4.12217144842418,4.64514416092682,107.558042219308));
#56880=CARTESIAN_POINT('Ctrl Pts',(-1.67827504581228,5.97938580429455,107.836411495039));
#56881=CARTESIAN_POINT('Ctrl Pts',(-5.93726307042192,1.82169398050257,108.114780770769));
#56882=CARTESIAN_POINT('Ctrl Pts',(-4.74300642626271,-4.00918342888258,
108.3931500465));
#56883=CARTESIAN_POINT('Ctrl Pts',(0.807596601941249,-6.15771462918907,
108.671519322229));
#56884=CARTESIAN_POINT('Ctrl Pts',(5.61644003286672,-2.65052128518285,108.94988859796));
#56885=CARTESIAN_POINT('Ctrl Pts',(5.26670765143319,3.29111717207553,109.22825787369));
#56886=CARTESIAN_POINT('Ctrl Pts',(0.079620906299245,6.20993737788685,109.506627149421));
#56887=CARTESIAN_POINT('Ctrl Pts',(-5.18059587832416,3.42506760100976,109.78499642515));
#56888=CARTESIAN_POINT('Ctrl Pts',(-5.68255005618204,-2.50565093039329,
110.063365700881));
#56889=CARTESIAN_POINT('Ctrl Pts',(-0.965207829057699,-6.13498456173453,
110.341734976611));
#56890=CARTESIAN_POINT('Ctrl Pts',(4.6386564176627,-4.12947071243673,110.620104252342));
#56891=CARTESIAN_POINT('Ctrl Pts',(5.98201745274544,1.668870552513,110.898473528072));
#56892=CARTESIAN_POINT('Ctrl Pts',(1.83102790983545,5.93439116669932,111.176842803802));
#56893=CARTESIAN_POINT('Ctrl Pts',(-4.0017202260902,4.74930489209694,111.455212079532));
#56894=CARTESIAN_POINT('Ctrl Pts',(-6.15897693945369,-0.797912767959604,
111.733581355263));
#56895=CARTESIAN_POINT('Ctrl Pts',(-2.65934970447637,-5.61226521783295,
112.011950630993));
#56896=CARTESIAN_POINT('Ctrl Pts',(3.28283135139781,-5.27187633051798,112.290319906723));
#56897=CARTESIAN_POINT('Ctrl Pts',(6.20980449865453,-0.089385762206777,
112.568689182453));
#56898=CARTESIAN_POINT('Ctrl Pts',(3.43320970985575,5.17520364953375,112.847058458183));
#56899=CARTESIAN_POINT('Ctrl Pts',(-2.49671218016352,5.6864830972596,113.125427733914));
#56900=CARTESIAN_POINT('Ctrl Pts',(-6.13345921428751,0.974853728857669,
113.403797009644));
#56901=CARTESIAN_POINT('Ctrl Pts',(-4.13675976562846,-4.63215720452932,
113.682166285374));
#56902=CARTESIAN_POINT('Ctrl Pts',(1.65946193264643,-5.9846343096377,113.960535561105));
#56903=CARTESIAN_POINT('Ctrl Pts',(5.93150458918226,-1.84035731163975,114.238904836835));
#56904=CARTESIAN_POINT('Ctrl Pts',(4.75559161446478,3.99424712836203,114.517274112565));
#56905=CARTESIAN_POINT('Ctrl Pts',(-0.788226961002809,6.16022402059727,
114.795643388296));
#56906=CARTESIAN_POINT('Ctrl Pts',(-5.60807652551605,2.66817154807391,115.074012664026));
#56907=CARTESIAN_POINT('Ctrl Pts',(-5.27703197398926,-3.2745374133595,115.352381939756));
#56908=CARTESIAN_POINT('Ctrl Pts',(-0.0991503970927691,-6.20965626462145,
115.630751215486));
#56909=CARTESIAN_POINT('Ctrl Pts',(5.16979862416974,-3.44134332950492,115.909120491217));
#56910=CARTESIAN_POINT('Ctrl Pts',(5.69040207753754,2.48776725638707,116.187489766947));
#56911=CARTESIAN_POINT('Ctrl Pts',(0.984497218165544,6.13191870081628,116.465859042677));
#56912=CARTESIAN_POINT('Ctrl Pts',(-4.62564653759719,4.14403858997612,116.744228318407));
#56913=CARTESIAN_POINT('Ctrl Pts',(-5.98723636850076,-1.65004920947743,
117.022597594138));
#56914=CARTESIAN_POINT('Ctrl Pts',(-1.8496821628465,-5.92860334500824,117.300966869868));
#56915=CARTESIAN_POINT('Ctrl Pts',(3.98676415417643,-4.76186657782114,117.579336145598));
#56916=CARTESIAN_POINT('Ctrl Pts',(6.16145586953622,0.778539205020277,117.857705421328));
#56917=CARTESIAN_POINT('Ctrl Pts',(2.67698679416211,5.60387396627344,118.136074697059));
#56918=CARTESIAN_POINT('Ctrl Pts',(-3.2662353784689,5.28217456909872,118.414443972789));
#56919=CARTESIAN_POINT('Ctrl Pts',(-6.20949267615386,0.108914786812677,
118.692813248519));
#56920=CARTESIAN_POINT('Ctrl Pts',(-3.44946843984602,-5.16438081559675,
118.97118252425));
#56921=CARTESIAN_POINT('Ctrl Pts',(2.47881618118194,-5.69430698732565,119.24955179998));
#56922=CARTESIAN_POINT('Ctrl Pts',(6.13036302512973,-0.994138273136335,
119.52792107571));
#56923=CARTESIAN_POINT('Ctrl Pts',(4.15130716748207,4.6191244329653,119.80629035144));
#56924=CARTESIAN_POINT('Ctrl Pts',(-1.64063240628113,5.98982362289971,120.084659627171));
#56925=CARTESIAN_POINT('Ctrl Pts',(-5.92568744134926,1.85900244040056,120.363028902901));
#56926=CARTESIAN_POINT('Ctrl Pts',(-4.76812976665383,-3.97927132204007,
120.641398178631));
#56927=CARTESIAN_POINT('Ctrl Pts',(0.768849523973782,-6.16267248321747,
120.919767454361));
#56928=CARTESIAN_POINT('Ctrl Pts',(5.59965755048293,-2.6857954209572,121.198136730092));
#56929=CARTESIAN_POINT('Ctrl Pts',(5.28730410315625,3.25792526727902,121.476506005822));
#56930=CARTESIAN_POINT('Ctrl Pts',(0.118678907173586,6.20931373360969,121.754875281552));
#56931=CARTESIAN_POINT('Ctrl Pts',(-5.15895023711994,3.45758502087614,122.033244557282));
#56932=CARTESIAN_POINT('Ctrl Pts',(-5.69819781714075,-2.46985897684768,
122.311613833013));
#56933=CARTESIAN_POINT('Ctrl Pts',(-1.00377686960519,-6.1287921907601,122.589983108743));
#56934=CARTESIAN_POINT('Ctrl Pts',(4.61259090614592,-4.15856548076738,122.868352384473));
#56935=CARTESIAN_POINT('Ctrl Pts',(5.9923960675984,1.63121154746421,123.146721660204));
#56936=CARTESIAN_POINT('Ctrl Pts',(1.86831811906265,5.92275688329723,123.425090935934));
#56937=CARTESIAN_POINT('Ctrl Pts',(-3.97176864633893,4.77438116947538,123.703460211664));
#56938=CARTESIAN_POINT('Ctrl Pts',(-6.16387386645271,-0.759157949374332,
123.981829487395));
#56939=CARTESIAN_POINT('Ctrl Pts',(-2.69459739191245,-5.59542727431215,
124.260198763124));
#56940=CARTESIAN_POINT('Ctrl Pts',(3.2496070724577,-5.29242059040039,124.538568038855));
#56941=CARTESIAN_POINT('Ctrl Pts',(6.20911949007491,-0.128442683197594,
124.816937314585));
#56942=CARTESIAN_POINT('Ctrl Pts',(3.46569295312417,5.153506806181,125.095306590315));
#56943=CARTESIAN_POINT('Ctrl Pts',(-2.46089547784216,5.70207473860405,125.373675866046));
#56944=CARTESIAN_POINT('Ctrl Pts',(-6.12720655598897,1.01341264151739,125.652045141776));
#56945=CARTESIAN_POINT('Ctrl Pts',(-4.16581284271013,-4.60604532710973,
125.930414417506));
#56946=CARTESIAN_POINT('Ctrl Pts',(1.62178539278297,-5.99495491636355,126.208783693237));
#56947=CARTESIAN_POINT('Ctrl Pts',(5.91981406391576,-1.8776268719497,126.487152968967));
#56948=CARTESIAN_POINT('Ctrl Pts',(4.78061626591979,3.96425179549011,126.765522244697));
#56949=CARTESIAN_POINT('Ctrl Pts',(-0.749455999002484,6.16506823020972,
127.043891520427));
#56950=CARTESIAN_POINT('Ctrl Pts',(-5.59119920962547,2.70337717567628,127.322260796158));
#56951=CARTESIAN_POINT('Ctrl Pts',(-5.29749369097637,-3.24125152930667,
127.600630071888));
#56952=CARTESIAN_POINT('Ctrl Pts',(-0.13826335471824,-6.2089652426601,127.878999347618));
#56953=CARTESIAN_POINT('Ctrl Pts',(5.14815866266899,-3.47368780450951,128.157368623348));
#56954=CARTESIAN_POINT('Ctrl Pts',(5.7057335741975,2.45172854905703,128.435737899079));
#56955=CARTESIAN_POINT('Ctrl Pts',(1.02343110214051,6.12597844780046,128.714107174809));
#56956=CARTESIAN_POINT('Ctrl Pts',(-4.60021590128167,4.17234580462416,128.992476450539));
#56957=CARTESIAN_POINT('Ctrl Pts',(-5.99612342097425,-1.61102240036703,
129.270845726269));
#56958=CARTESIAN_POINT('Ctrl Pts',(-1.88954273411231,-5.91940060591759,
129.549215002));
#56959=CARTESIAN_POINT('Ctrl Pts',(3.96177486026028,-4.78181212020278,129.82758427773));
#56960=CARTESIAN_POINT('Ctrl Pts',(5.79010620548154,-0.189962750713211,
130.059558674172));
#56961=CARTESIAN_POINT('Ctrl Pts',(4.44638236249096,3.17706810551834,130.245138191326));
#56962=CARTESIAN_POINT('Ctrl Pts',(3.08009875615274,4.34188596571016,130.337927949902));
#56963=CARTESIAN_POINT('Ctrl Pts',(2.29321473482586,4.72388001049864,130.384322829191));
#56964=CARTESIAN_POINT('Ctrl Pts',(2.85706463458369,-4.00329423554042,-10.));
#56965=CARTESIAN_POINT('Ctrl Pts',(3.52391651473643,-3.52737645103792,-9.95360512071162));
#56966=CARTESIAN_POINT('Ctrl Pts',(4.6032797975914,-2.23787345781402,-9.86081536213486));
#56967=CARTESIAN_POINT('Ctrl Pts',(5.31710770646798,1.0817198372055,-9.67523584498136));
#56968=CARTESIAN_POINT('Ctrl Pts',(2.91000325553484,5.03585724930024,-9.44326144853946));
#56969=CARTESIAN_POINT('Ctrl Pts',(-2.67142550958262,5.17047615300083,-9.16489217280919));
#56970=CARTESIAN_POINT('Ctrl Pts',(-5.78925343142622,0.549143031760425,
-8.88652289707893));
#56971=CARTESIAN_POINT('Ctrl Pts',(-3.59496519784923,-4.57298129089445,
-8.60815362134865));
#56972=CARTESIAN_POINT('Ctrl Pts',(1.90395420368265,-5.4968079578387,-8.32978434561839));
#56973=CARTESIAN_POINT('Ctrl Pts',(5.65268654860171,-1.37094194360677,-8.05141506988812));
#56974=CARTESIAN_POINT('Ctrl Pts',(4.21031778233782,4.01357646538516,-7.77304579415784));
#56975=CARTESIAN_POINT('Ctrl Pts',(-1.09954047142025,5.71199305956496,-7.49467651842759));
#56976=CARTESIAN_POINT('Ctrl Pts',(-5.39928022209077,2.16392258626905,-7.21630724269731));
#56977=CARTESIAN_POINT('Ctrl Pts',(-4.74001446358611,-3.37158453305954,
-6.93793796696704));
#56978=CARTESIAN_POINT('Ctrl Pts',(0.272909909778823,-5.81040739879541,
-6.65956869123677));
#56979=CARTESIAN_POINT('Ctrl Pts',(5.03514064798181,-2.9124777495484,-6.38119941550651));
#56980=CARTESIAN_POINT('Ctrl Pts',(5.17272309584991,2.66048658894571,-6.10283013977622));
#56981=CARTESIAN_POINT('Ctrl Pts',(0.559264958796863,5.78985906598745,-5.82446086404598));
#56982=CARTESIAN_POINT('Ctrl Pts',(-4.56786091744391,3.60137092478267,-5.54609158831568));
#56983=CARTESIAN_POINT('Ctrl Pts',(-5.49951019303444,-1.89489494166458,
-5.26772231258544));
#56984=CARTESIAN_POINT('Ctrl Pts',(-1.37997979498124,-5.65074267591175,
-4.98935303685515));
#56985=CARTESIAN_POINT('Ctrl Pts',(4.00703078514331,-4.21650789487217,-4.7109837611249));
#56986=CARTESIAN_POINT('Ctrl Pts',(5.71367268487829,1.09049576997227,-4.43261448539462));
#56987=CARTESIAN_POINT('Ctrl Pts',(2.17243253669944,5.39590335156548,-4.15424520966435));
#56988=CARTESIAN_POINT('Ctrl Pts',(-3.36413869033177,4.74529310749045,-3.87587593393408));
#56989=CARTESIAN_POINT('Ctrl Pts',(-5.81082307364013,-0.263763748565971,
-3.59750665820381));
#56990=CARTESIAN_POINT('Ctrl Pts',(-2.92039509627066,-5.03055946195533,
-3.31913738247355));
#56991=CARTESIAN_POINT('Ctrl Pts',(2.65235109881223,-5.17689768424732,-3.04076810674327));
#56992=CARTESIAN_POINT('Ctrl Pts',(5.78897154557153,-0.568370014814376,
-2.76239883101301));
#56993=CARTESIAN_POINT('Ctrl Pts',(3.60854980134286,4.56219293151739,-2.48402955528274));
#56994=CARTESIAN_POINT('Ctrl Pts',(-1.8862450334912,5.50248268361132,-2.20566027955247));
#56995=CARTESIAN_POINT('Ctrl Pts',(-5.6485655710584,1.38886392626336,-1.9272910038222));
#56996=CARTESIAN_POINT('Ctrl Pts',(-4.22280370010565,-4.00039559592092,
-1.64892172809193));
#56997=CARTESIAN_POINT('Ctrl Pts',(1.08150986877385,-5.71538033878776,-1.37055245236166));
#56998=CARTESIAN_POINT('Ctrl Pts',(5.39248056989081,-2.18091478914392,-1.0921831766314));
#56999=CARTESIAN_POINT('Ctrl Pts',(4.75057726644074,3.35667270511782,-0.813813900901123));
#57000=CARTESIAN_POINT('Ctrl Pts',(-0.254626070074851,5.81123064231236,
-0.535444625170857));
#57001=CARTESIAN_POINT('Ctrl Pts',(-5.02596099912126,2.9283019053962,-0.257075349440584));
#57002=CARTESIAN_POINT('Ctrl Pts',(-5.18106203404851,-2.64420729389814,
0.0212939262896814));
#57003=CARTESIAN_POINT('Ctrl Pts',(-0.577472308506603,-5.78807064112712,
0.299663202019953));
#57004=CARTESIAN_POINT('Ctrl Pts',(4.5565129461533,-3.61571926251521,0.578032477750221));
#57005=CARTESIAN_POINT('Ctrl Pts',(5.50544194895434,1.87759020035487,0.856401753480491));
#57006=CARTESIAN_POINT('Ctrl Pts',(1.3977444217788,5.64637463733703,1.13477102921076));
#57007=CARTESIAN_POINT('Ctrl Pts',(-3.99375040828915,4.2290889905592,1.41314030494103));
#57008=CARTESIAN_POINT('Ctrl Pts',(-5.71707391697906,-1.07252125460282,
1.6915095806713));
#57009=CARTESIAN_POINT('Ctrl Pts',(-2.18939161896353,-5.38904447491294,
1.96987885640157));
#57010=CARTESIAN_POINT('Ctrl Pts',(3.34919840410121,-4.75584966790831,2.24824813213183));
#57011=CARTESIAN_POINT('Ctrl Pts',(5.81162385012341,0.245487756220548,2.5266174078621));
#57012=CARTESIAN_POINT('Ctrl Pts',(2.93620146934825,5.02135011179013,2.80498668359237));
#57013=CARTESIAN_POINT('Ctrl Pts',(-2.63605694837504,5.18521357117537,3.08335595932264));
#57014=CARTESIAN_POINT('Ctrl Pts',(-5.7871554259382,0.586573175155174,3.36172523505291));
#57015=CARTESIAN_POINT('Ctrl Pts',(-3.62287978254425,-4.55082169448657,
3.64009451078318));
#57016=CARTESIAN_POINT('Ctrl Pts',(1.86893072420659,-5.50838760091319,3.91846378651344));
#57017=CARTESIAN_POINT('Ctrl Pts',(5.64416974217652,-1.40662146125979,4.19683306224373));
#57018=CARTESIAN_POINT('Ctrl Pts',(4.23536382377072,3.98709534549548,4.47520233797398));
#57019=CARTESIAN_POINT('Ctrl Pts',(-1.06352998838801,5.71875335869428,4.75357161370427));
#57020=CARTESIAN_POINT('Ctrl Pts',(-5.38559505463087,2.1978630351578,5.03194088943452));
#57021=CARTESIAN_POINT('Ctrl Pts',(-4.76111030971177,-3.34171582163024,
5.3103101651648));
#57022=CARTESIAN_POINT('Ctrl Pts',(0.236348835348182,-5.81200268769786,
5.58867944089506));
#57023=CARTESIAN_POINT('Ctrl Pts',(5.01672680831839,-2.94409377304407,5.86704871662534));
#57024=CARTESIAN_POINT('Ctrl Pts',(5.18935228697503,2.62790008475296,6.1454179923556));
#57025=CARTESIAN_POINT('Ctrl Pts',(0.59567259140266,5.78622590101952,6.42378726808587));
#57026=CARTESIAN_POINT('Ctrl Pts',(-4.54511919013754,3.63003134438547,6.70215654381614));
#57027=CARTESIAN_POINT('Ctrl Pts',(-5.51131963244376,-1.86026662680852,
6.9805258195464));
#57028=CARTESIAN_POINT('Ctrl Pts',(-1.41549502262945,-5.64195089084342,
7.25889509527668));
#57029=CARTESIAN_POINT('Ctrl Pts',(3.98043042392857,-4.24162818432278,7.53726437100694));
#57030=CARTESIAN_POINT('Ctrl Pts',(5.72041865981625,1.05453609241393,7.81563364673722));
#57031=CARTESIAN_POINT('Ctrl Pts',(2.20632901676084,5.38213231754632,8.09400292246748));
#57032=CARTESIAN_POINT('Ctrl Pts',(-3.33422497619683,4.76635917885788,8.37237219819775));
#57033=CARTESIAN_POINT('Ctrl Pts',(-5.81236715410425,-0.227209330062944,
8.65074147392803));
#57034=CARTESIAN_POINT('Ctrl Pts',(-2.9519787969659,-5.01209110013389,8.92911074965828));
#57035=CARTESIAN_POINT('Ctrl Pts',(2.61973672319965,-5.19347817121596,9.20748002538857));
#57036=CARTESIAN_POINT('Ctrl Pts',(5.7852820686703,-0.60477053474805,9.48584930111882));
#57037=CARTESIAN_POINT('Ctrl Pts',(3.63717393035499,4.53940544720601,9.7642185768491));
#57038=CARTESIAN_POINT('Ctrl Pts',(-1.8515979295839,5.51423803629642,10.0425878525794));
#57039=CARTESIAN_POINT('Ctrl Pts',(-5.63971808882434,1.42436508394621,10.3209571283096));
#57040=CARTESIAN_POINT('Ctrl Pts',(-4.24788205672562,-3.97375566006845,
10.5993264040399));
#57041=CARTESIAN_POINT('Ctrl Pts',(1.04553958891947,-5.72206981622731,10.8776956797702));
#57042=CARTESIAN_POINT('Ctrl Pts',(5.37865627222158,-2.214789542839,11.1560649555005));
#57043=CARTESIAN_POINT('Ctrl Pts',(4.77159626236785,3.32672588632348,11.4344342312307));
#57044=CARTESIAN_POINT('Ctrl Pts',(-0.218069262963983,5.81271724844138,
11.712803506961));
#57045=CARTESIAN_POINT('Ctrl Pts',(-5.00744299869918,2.95985652161657,11.9911727826912));
#57046=CARTESIAN_POINT('Ctrl Pts',(-5.19759121369619,-2.61156688390049,
12.2695420584215));
#57047=CARTESIAN_POINT('Ctrl Pts',(-0.613866982695112,-5.78432393122432,
12.5479113341518));
#57048=CARTESIAN_POINT('Ctrl Pts',(4.53368047982022,-3.64430752279149,12.8262806098821));
#57049=CARTESIAN_POINT('Ctrl Pts',(5.51714280525491,1.84292465396758,13.1046498856123));
#57050=CARTESIAN_POINT('Ctrl Pts',(1.43323162327729,5.63747134164028,13.3830191613426));
#57051=CARTESIAN_POINT('Ctrl Pts',(-3.96707107041965,4.25412542551546,13.6613884370729));
#57052=CARTESIAN_POINT('Ctrl Pts',(-5.72370682384467,-1.0365405001501,13.9397577128031));
#57053=CARTESIAN_POINT('Ctrl Pts',(-2.22324459247222,-5.3751669272517,14.2181269885334));
#57054=CARTESIAN_POINT('Ctrl Pts',(3.31921857055293,-4.77682154729211,14.4964962642637));
#57055=CARTESIAN_POINT('Ctrl Pts',(5.81305296984359,0.208928656651545,14.774865539994));
#57056=CARTESIAN_POINT('Ctrl Pts',(2.96772692751709,5.00278251550746,15.0532348157242));
#57057=CARTESIAN_POINT('Ctrl Pts',(-2.60339058705663,5.2016914042456,15.3316040914545));
#57058=CARTESIAN_POINT('Ctrl Pts',(-5.78335149105072,0.62296191275141,15.6099733671847));
#57059=CARTESIAN_POINT('Ctrl Pts',(-3.65143210405607,-4.52794430213603,
15.888342642915));
#57060=CARTESIAN_POINT('Ctrl Pts',(1.83424682140562,-5.52003393213674,16.1667119186453));
#57061=CARTESIAN_POINT('Ctrl Pts',(5.63521065484668,-1.44209461869877,16.4450811943755));
#57062=CARTESIAN_POINT('Ctrl Pts',(4.26035827525457,3.96037667151086,16.7234504701058));
#57063=CARTESIAN_POINT('Ctrl Pts',(-1.02753884835743,5.7253296786206,17.0018197458361));
#57064=CARTESIAN_POINT('Ctrl Pts',(-5.37166429126469,2.23169414475401,17.2801890215664));
#57065=CARTESIAN_POINT('Ctrl Pts',(-4.78203502071031,-3.31170304744819,
17.5585582972966));
#57066=CARTESIAN_POINT('Ctrl Pts',(0.199787533727289,-5.81337431748075,
17.8369275730269));
#57067=CARTESIAN_POINT('Ctrl Pts',(4.99810966208265,-2.97558999520659,18.1152968487571));
#57068=CARTESIAN_POINT('Ctrl Pts',(5.20577873272567,2.59520785288553,18.3936661244875));
#57069=CARTESIAN_POINT('Ctrl Pts',(0.632055302428017,5.78236475055406,18.6720354002177));
#57070=CARTESIAN_POINT('Ctrl Pts',(-4.52219692833723,3.65854765653187,18.950404675948));
#57071=CARTESIAN_POINT('Ctrl Pts',(-5.52291140979303,-1.8255644533556,19.2287739516782));
#57072=CARTESIAN_POINT('Ctrl Pts',(-1.45095404829527,-5.63293603403351,
19.5071432274085));
#57073=CARTESIAN_POINT('Ctrl Pts',(3.95367247989527,-4.26658059053105,19.7855125031388));
#57074=CARTESIAN_POINT('Ctrl Pts',(5.72693837654226,1.01853465579974,20.063881778869));
#57075=CARTESIAN_POINT('Ctrl Pts',(2.24013817879126,5.36814837292146,20.3422510545993));
#57076=CARTESIAN_POINT('Ctrl Pts',(-3.30417933559282,4.78723666973118,20.6206203303296));
#57077=CARTESIAN_POINT('Ctrl Pts',(-5.81368129055826,-0.190645916794373,
20.8989896060598));
#57078=CARTESIAN_POINT('Ctrl Pts',(-2.98344570524222,-4.99342444997913,
21.1773588817902));
#57079=CARTESIAN_POINT('Ctrl Pts',(2.58701870162035,-5.20985318902981,21.4557281575204));
#57080=CARTESIAN_POINT('Ctrl Pts',(5.7813637121742,-0.641147129240114,21.7340974332507));
#57081=CARTESIAN_POINT('Ctrl Pts',(3.66565416262452,4.51643837263511,22.0124667089809));
#57082=CARTESIAN_POINT('Ctrl Pts',(-1.81687757128598,5.5257752311088,22.2908359847112));
#57083=CARTESIAN_POINT('Ctrl Pts',(-5.6306474848251,1.45980989016045,22.5692052604415));
#57084=CARTESIAN_POINT('Ctrl Pts',(-4.2727923559593,-3.94695851215,22.8475745361717));
#57085=CARTESIAN_POINT('Ctrl Pts',(1.00952794474132,-5.72853291363189,23.1259438119021));
#57086=CARTESIAN_POINT('Ctrl Pts',(5.36461918091565,-2.24857667370483,23.4043130876322));
#57087=CARTESIAN_POINT('Ctrl Pts',(4.79242648149282,3.29664745359036,23.6826823633626));
#57088=CARTESIAN_POINT('Ctrl Pts',(-0.181503828456812,5.8139738883171,23.9610516390928));
#57089=CARTESIAN_POINT('Ctrl Pts',(-4.98872689078183,2.99129403819949,24.2394209148231));
#57090=CARTESIAN_POINT('Ctrl Pts',(-5.2139147630833,-2.57882315351005,24.5177901905534));
#57091=CARTESIAN_POINT('Ctrl Pts',(-0.650237370706631,-5.78034837838638,
24.7961594662836));
#57092=CARTESIAN_POINT('Ctrl Pts',(4.51066864926873,-3.67275160476199,25.0745287420139));
#57093=CARTESIAN_POINT('Ctrl Pts',(5.52862538900271,1.8081861966767,25.3528980177442));
#57094=CARTESIAN_POINT('Ctrl Pts',(1.46866212239656,5.62834501288036,25.6312672934744));
#57095=CARTESIAN_POINT('Ctrl Pts',(-3.94023478487658,4.27899355617956,25.9096365692047));
#57096=CARTESIAN_POINT('Ctrl Pts',(-5.73011328594672,-1.00051873745295,
26.1880058449349));
#57097=CARTESIAN_POINT('Ctrl Pts',(-2.25700960862895,-5.36107672397384,
26.4663751206653));
#57098=CARTESIAN_POINT('Ctrl Pts',(3.28910742006482,-4.79760444316246,26.7447443963955));
#57099=CARTESIAN_POINT('Ctrl Pts',(5.81425211003376,0.17236129132015,27.0231136721258));
#57100=CARTESIAN_POINT('Ctrl Pts',(2.99913497467191,4.98401699610638,27.3014829478561));
#57101=CARTESIAN_POINT('Ctrl Pts',(-2.57062122881967,5.21796344484313,27.5798522235863));
#57102=CARTESIAN_POINT('Ctrl Pts',(-5.7793187517012,0.659326004350221,27.8582214993166));
#57103=CARTESIAN_POINT('Ctrl Pts',(-3.6798399653946,-4.50488777250468,28.1365907750468));
#57104=CARTESIAN_POINT('Ctrl Pts',(1.79949035101865,-5.53146187642727,28.4149600507771));
#57105=CARTESIAN_POINT('Ctrl Pts',(5.62602862389248,-1.47751072311508,28.6933293265074));
#57106=CARTESIAN_POINT('Ctrl Pts',(4.28518417585832,3.93350131470056,28.9716986022376));
#57107=CARTESIAN_POINT('Ctrl Pts',(-0.991507056211286,5.73167948957902,
29.250067877968));
#57108=CARTESIAN_POINT('Ctrl Pts',(-5.35752101085537,2.26543696271178,29.5284371536982));
#57109=CARTESIAN_POINT('Ctrl Pts',(-4.80277054193674,-3.2815592536601,29.8068064294285));
#57110=CARTESIAN_POINT('Ctrl Pts',(0.163218327990816,-5.81451595502028,
30.0851757051587));
#57111=CARTESIAN_POINT('Ctrl Pts',(4.97929477759872,-3.00696849527155,30.363544980889));
#57112=CARTESIAN_POINT('Ctrl Pts',(5.22199922429825,2.56241294782984,30.6419142566192));
#57113=CARTESIAN_POINT('Ctrl Pts',(0.668413007697845,5.77827483466457,30.9202835323496));
#57114=CARTESIAN_POINT('Ctrl Pts',(-4.4990957566372,3.68691922699517,31.1986528080798));
#57115=CARTESIAN_POINT('Ctrl Pts',(-5.53428468636881,-1.79079005581371,
31.4770220838101));
#57116=CARTESIAN_POINT('Ctrl Pts',(-1.48635567043628,-5.62369832358916,
31.7553913595403));
#57117=CARTESIAN_POINT('Ctrl Pts',(3.92675811827154,-4.29136419968826,32.0337606352706));
#57118=CARTESIAN_POINT('Ctrl Pts',(5.73323152065607,0.982492923299337,32.3121299110009));
#57119=CARTESIAN_POINT('Ctrl Pts',(2.27385871511533,5.35395205035231,32.5904991867312));
#57120=CARTESIAN_POINT('Ctrl Pts',(-3.27400297304034,4.80792476504159,32.8688684624614));
#57121=CARTESIAN_POINT('Ctrl Pts',(-5.81476542262427,-0.154074961076227,
33.1472377381917));
#57122=CARTESIAN_POINT('Ctrl Pts',(-3.01479458062872,-4.97456024693533,
33.425607013922));
#57123=CARTESIAN_POINT('Ctrl Pts',(2.55419833083681,-5.22602209146957,33.7039762896522));
#57124=CARTESIAN_POINT('Ctrl Pts',(5.77721662985775,-0.677498358280351,
33.9823455653825));
#57125=CARTESIAN_POINT('Ctrl Pts',(3.69398937205911,4.49329261598795,34.2607148411128));
#57126=CARTESIAN_POINT('Ctrl Pts',(-1.78208533257483,5.53709381184744,34.539084116843));
#57127=CARTESIAN_POINT('Ctrl Pts',(-5.62135411773242,1.49519694248963,34.8174533925734));
#57128=CARTESIAN_POINT('Ctrl Pts',(-4.29753361238825,-3.92000521226321,
35.0958226683035));
#57129=CARTESIAN_POINT('Ctrl Pts',(0.973476361005944,-5.73476937534023,
35.3741919440339));
#57130=CARTESIAN_POINT('Ctrl Pts',(5.3503698512895,-2.28227484501538,35.6525612197641));
#57131=CARTESIAN_POINT('Ctrl Pts',(4.81306709973239,3.26643859688978,35.9309304954944));
#57132=CARTESIAN_POINT('Ctrl Pts',(-0.144931213185082,5.81500051222889,
36.2092997712246));
#57133=CARTESIAN_POINT('Ctrl Pts',(-4.96981341582323,3.02261321139193,36.4876690469549));
#57134=CARTESIAN_POINT('Ctrl Pts',(-5.23003203640979,-2.54597739815277,
36.7660383226852));
#57135=CARTESIAN_POINT('Ctrl Pts',(-0.6865820336325,-5.77614413989737,37.0444075984155));
#57136=CARTESIAN_POINT('Ctrl Pts',(4.48747836490629,-3.70105038310417,37.3227768741457));
#57137=CARTESIAN_POINT('Ctrl Pts',(5.53988924591708,1.77337620282608,37.601146149876));
#57138=CARTESIAN_POINT('Ctrl Pts',(1.50403451741344,5.61899601211875,37.8795154256062));
#57139=CARTESIAN_POINT('Ctrl Pts',(-3.91324261337339,4.30369239870326,38.1578847013366));
#57140=CARTESIAN_POINT('Ctrl Pts',(-5.73629304982887,-0.964457391626264,
38.4362539770668));
#57141=CARTESIAN_POINT('Ctrl Pts',(-2.29068533160149,-5.3467744225246,38.7146232527971));
#57142=CARTESIAN_POINT('Ctrl Pts',(3.25886614391259,-4.81819753329374,38.9929925285273));
#57143=CARTESIAN_POINT('Ctrl Pts',(5.81522122325282,0.135787106926827,39.2713618042576));
#57144=CARTESIAN_POINT('Ctrl Pts',(3.03042436822842,4.96505429599969,39.5497310799879));
#57145=CARTESIAN_POINT('Ctrl Pts',(-2.53775017010531,5.23402904920365,39.8281003557182));
#57146=CARTESIAN_POINT('Ctrl Pts',(-5.77505736743528,0.695664011293557,
40.1064696314484));
#57147=CARTESIAN_POINT('Ctrl Pts',(-3.70810224267088,-4.48165301776886,
40.3848389071787));
#57148=CARTESIAN_POINT('Ctrl Pts',(1.76466268810206,-5.5426709816656,40.663208182909));
#57149=CARTESIAN_POINT('Ctrl Pts',(5.61662401257895,-1.5128683733554,40.9415774586392));
#57150=CARTESIAN_POINT('Ctrl Pts',(4.30984054340475,3.90647033832362,41.2199467343696));
#57151=CARTESIAN_POINT('Ctrl Pts',(-0.955436037461097,5.73780254035447,
41.4983160100997));
#57152=CARTESIAN_POINT('Ctrl Pts',(-5.34316577294787,2.29909015407745,41.7766852858301));
#57153=CARTESIAN_POINT('Ctrl Pts',(-4.82331605303984,-3.25128563283292,
42.0550545615603));
#57154=CARTESIAN_POINT('Ctrl Pts',(0.126642664911688,-5.81542755515032,
42.3334238372905));
#57155=CARTESIAN_POINT('Ctrl Pts',(4.96028289923243,-3.03822803182378,42.6117931130208));
#57156=CARTESIAN_POINT('Ctrl Pts',(5.23801311996793,2.52951666703768,42.8901623887511));
#57157=CARTESIAN_POINT('Ctrl Pts',(0.704744268806608,5.77395631515876,43.1685316644814));
#57158=CARTESIAN_POINT('Ctrl Pts',(-4.47581658897993,3.7151449333222,43.4469009402115));
#57159=CARTESIAN_POINT('Ctrl Pts',(-5.54543901221464,-1.7559448099486,43.725270215942));
#57160=CARTESIAN_POINT('Ctrl Pts',(-1.52169848847216,-5.61423812497824,
44.0036394916721));
#57161=CARTESIAN_POINT('Ctrl Pts',(3.89968840385962,-4.31597803129028,44.2820087674025));
#57162=CARTESIAN_POINT('Ctrl Pts',(5.73929784318452,0.946412320817448,44.5603780431327));
#57163=CARTESIAN_POINT('Ctrl Pts',(2.30748929166079,5.33954391148237,44.838747318863));
#57164=CARTESIAN_POINT('Ctrl Pts',(-3.24369708239501,4.82842264631418,45.1171165945933));
#57165=CARTESIAN_POINT('Ctrl Pts',(-5.8156195074112,-0.117497909751016,
45.3954858703235));
#57166=CARTESIAN_POINT('Ctrl Pts',(-3.046024182882,-4.95549923731964,45.6738551460538));
#57167=CARTESIAN_POINT('Ctrl Pts',(2.52127690930862,-5.24198423885123,45.9522244217841));
#57168=CARTESIAN_POINT('Ctrl Pts',(5.77284098579036,-0.713822783719208,
46.2305936975144));
#57169=CARTESIAN_POINT('Ctrl Pts',(3.72217843764396,4.46996909297098,46.5089629732446));
#57170=CARTESIAN_POINT('Ctrl Pts',(-1.74722258992204,5.54819333071977,46.7873322489749));
#57171=CARTESIAN_POINT('Ctrl Pts',(-5.61183835521605,1.53052484092992,47.0657015247051));
#57172=CARTESIAN_POINT('Ctrl Pts',(-4.32210484718396,-3.89289682675079,
47.3440708004355));
#57173=CARTESIAN_POINT('Ctrl Pts',(0.937386264007801,-5.74077895462167,
47.6224400761656));
#57174=CARTESIAN_POINT('Ctrl Pts',(5.33590884708369,-2.31588272358329,47.900809351896));
#57175=CARTESIAN_POINT('Ctrl Pts',(4.83351730048996,3.23610051136267,48.1791786276262));
#57176=CARTESIAN_POINT('Ctrl Pts',(-0.108352864056654,5.81579707956082,
48.4575479033566));
#57177=CARTESIAN_POINT('Ctrl Pts',(-4.95070332208964,3.05381280212593,48.7359171790867));
#57178=CARTESIAN_POINT('Ctrl Pts',(-5.24594239603436,-2.51303091729227,
49.0142864548171));
#57179=CARTESIAN_POINT('Ctrl Pts',(-0.722899533583313,-5.77171138208786,
49.2926557305472));
#57180=CARTESIAN_POINT('Ctrl Pts',(4.46411054420093,-3.72920273824468,49.5710250062776));
#57181=CARTESIAN_POINT('Ctrl Pts',(5.55093393037054,1.73849604958962,49.8493942820078));
#57182=CARTESIAN_POINT('Ctrl Pts',(1.53934740890388,5.60942470922629,50.1277635577381));
#57183=CARTESIAN_POINT('Ctrl Pts',(-3.88609562379059,4.32822097593609,50.4061328334684));
#57184=CARTESIAN_POINT('Ctrl Pts',(-5.74224587100358,-0.92835788935079,
50.6845021091986));
#57185=CARTESIAN_POINT('Ctrl Pts',(-2.32427042909063,-5.33226058874023,
50.962871384929));
#57186=CARTESIAN_POINT('Ctrl Pts',(3.22849593851986,-4.8386000029697,51.2412406606591));
#57187=CARTESIAN_POINT('Ctrl Pts',(5.81596027116012,0.0992075504414687,
51.5196099363895));
#57188=CARTESIAN_POINT('Ctrl Pts',(3.06159387029672,4.94589516540121,51.7979792121197));
#57189=CARTESIAN_POINT('Ctrl Pts',(-2.50477871137838,5.24988758173003,52.07634848785));
#57190=CARTESIAN_POINT('Ctrl Pts',(-5.77056750684446,0.731974495954949,
52.3547177635803));
#57191=CARTESIAN_POINT('Ctrl Pts',(-3.73621781775542,-4.45824095715614,
52.6330870393105));
#57192=CARTESIAN_POINT('Ctrl Pts',(1.72976521052916,-5.55366080439025,52.9114563150408));
#57193=CARTESIAN_POINT('Ctrl Pts',(5.6069971929771,-1.54816617057876,53.1898255907711));
#57194=CARTESIAN_POINT('Ctrl Pts',(4.33432640242356,3.87928481179605,53.4681948665013));
#57195=CARTESIAN_POINT('Ctrl Pts',(-0.919327219170563,5.74369858870307,
53.7465641422317));
#57196=CARTESIAN_POINT('Ctrl Pts',(-5.3285991454729,2.33265238744289,54.0249334179618));
#57197=CARTESIAN_POINT('Ctrl Pts',(-4.84367074118554,-3.2208833826701,54.3033026936922));
#57198=CARTESIAN_POINT('Ctrl Pts',(0.0900619915185718,-5.81610908180557,
54.5816719694224));
#57199=CARTESIAN_POINT('Ctrl Pts',(4.94107477914329,-3.06936736815449,54.8600412451526));
#57200=CARTESIAN_POINT('Ctrl Pts',(5.25381978618318,2.49652031197179,55.138410520883));
#57201=CARTESIAN_POINT('Ctrl Pts',(0.741047648394848,5.76940936288854,55.4167797966132));
#57202=CARTESIAN_POINT('Ctrl Pts',(-4.45236034635004,3.74322365883036,55.6951490723435));
#57203=CARTESIAN_POINT('Ctrl Pts',(-5.55637394603631,-1.7210300943291,55.9735183480737));
#57204=CARTESIAN_POINT('Ctrl Pts',(-1.55698110414879,-5.60455581247088,
56.2518876238041));
#57205=CARTESIAN_POINT('Ctrl Pts',(3.87246440760804,-4.34042111154972,56.5302568995343));
#57206=CARTESIAN_POINT('Ctrl Pts',(5.74513710412806,0.910294275796876,56.8086261752646));
#57207=CARTESIAN_POINT('Ctrl Pts',(2.34102857791428,5.3249245263352,57.0869954509948));
#57208=CARTESIAN_POINT('Ctrl Pts',(-3.21326286263679,4.8487295025993,57.3653647267251));
#57209=CARTESIAN_POINT('Ctrl Pts',(-5.81624351112921,-0.0809162099021229,
57.6437340024553));
#57210=CARTESIAN_POINT('Ctrl Pts',(-3.0771332764778,-4.93624217523513,57.9221032781857));
#57211=CARTESIAN_POINT('Ctrl Pts',(2.4882557394928,-5.25773899967072,58.2004725539159));
#57212=CARTESIAN_POINT('Ctrl Pts',(5.76823695308387,-0.750118968468039,
58.4788418296462));
#57213=CARTESIAN_POINT('Ctrl Pts',(3.7502202441463,4.44646872632352,58.7572111053764));
#57214=CARTESIAN_POINT('Ctrl Pts',(-1.7122907225886,5.55907334859995,59.0355803811067));
#57215=CARTESIAN_POINT('Ctrl Pts',(-5.60210057374436,1.5657921878175,59.313949656837));
#57216=CARTESIAN_POINT('Ctrl Pts',(-4.34650508824432,-3.86563442809122,
59.5923189325673));
#57217=CARTESIAN_POINT('Ctrl Pts',(0.901259081565336,-5.74656141372159,
59.8706882082974));
#57218=CARTESIAN_POINT('Ctrl Pts',(5.32123674041329,-2.34939897979313,60.1490574840279));
#57219=CARTESIAN_POINT('Ctrl Pts',(4.85377627470227,3.20563439726283,60.4274267597579));
#57220=CARTESIAN_POINT('Ctrl Pts',(-0.0717702282064447,5.81636355879867,
60.7057960354884));
#57221=CARTESIAN_POINT('Ctrl Pts',(-4.93139736562627,3.08489157606423,60.9841653112185));
#57222=CARTESIAN_POINT('Ctrl Pts',(-5.26164521250164,-2.47998501437728,
61.2625345869489));
#57223=CARTESIAN_POINT('Ctrl Pts',(-0.75918843374404,-5.76705028032932,
61.5409038626791));
#57224=CARTESIAN_POINT('Ctrl Pts',(4.4405661116445,-3.75720755640298,61.8192731384095));
#57225=CARTESIAN_POINT('Ctrl Pts',(5.56175900540656,1.703547116917,62.0976424141395));
#57226=CARTESIAN_POINT('Ctrl Pts',(1.57459939979797,5.59963148286865,62.3760116898701));
#57227=CARTESIAN_POINT('Ctrl Pts',(-3.85879489013386,4.35257831746365,62.6543809656001));
#57228=CARTESIAN_POINT('Ctrl Pts',(-5.74797151396171,-0.89222165881688,
62.9327502413306));
#57229=CARTESIAN_POINT('Ctrl Pts',(-2.35776357238246,-5.31753579682578,
63.2111195170607));
#57230=CARTESIAN_POINT('Ctrl Pts',(3.19799800541104,-4.85881104501553,63.489488792791));
#57231=CARTESIAN_POINT('Ctrl Pts',(5.81646922451705,0.0626240690466223,
63.7678580685212));
#57232=CARTESIAN_POINT('Ctrl Pts',(3.09264224773008,4.92654036229607,64.0462273442516));
#57233=CARTESIAN_POINT('Ctrl Pts',(-2.47170815707546,5.26553841501739,64.3245966199818));
#57234=CARTESIAN_POINT('Ctrl Pts',(-5.76584934755931,0.768256021797297,
64.6029658957121));
#57235=CARTESIAN_POINT('Ctrl Pts',(-3.76418557832305,-4.43465251690848,
64.8813351714424));
#57236=CARTESIAN_POINT('Ctrl Pts',(1.69479929893489,-5.56443090981521,65.1597044471726));
#57237=CARTESIAN_POINT('Ctrl Pts',(5.59714854594884,-1.58340271831267,65.4380737229028));
#57238=CARTESIAN_POINT('Ctrl Pts',(4.3586407841906,3.85194581064795,65.7164429986333));
#57239=CARTESIAN_POINT('Ctrl Pts',(-0.883182029898331,5.74936740136187,
65.9948122743633));
#57240=CARTESIAN_POINT('Ctrl Pts',(-5.31382170472409,2.36612233499885,66.2731815500938));
#57241=CARTESIAN_POINT('Ctrl Pts',(-4.8638338010895,-3.19035370596371,66.5515508258239));
#57242=CARTESIAN_POINT('Ctrl Pts',(0.0534777550381669,-5.8165605080231,
66.8299201015543));
#57243=CARTESIAN_POINT('Ctrl Pts',(4.92167117725461,-3.10038527231038,67.1082893772844));
#57244=CARTESIAN_POINT('Ctrl Pts',(5.26941859759108,2.46342518805391,67.3866586530149));
#57245=CARTESIAN_POINT('Ctrl Pts',(0.777321710206332,5.76463415774316,67.665027928745));
#57246=CARTESIAN_POINT('Ctrl Pts',(-4.42872795673757,3.77115429265218,67.9433972044754));
#57247=CARTESIAN_POINT('Ctrl Pts',(-5.56708905521936,-1.68604729027233,
68.2217664802056));
#57248=CARTESIAN_POINT('Ctrl Pts',(-1.59220212159397,-5.59465176912459,
68.5001357559359));
#57249=CARTESIAN_POINT('Ctrl Pts',(3.84508720656895,-4.36469247343464,68.7785050316661));
#57250=CARTESIAN_POINT('Ctrl Pts',(5.75074907247032,0.874140217161407,69.0568743073964));
#57251=CARTESIAN_POINT('Ctrl Pts',(2.37447524697441,5.31009447329176,69.3352435831267));
#57252=CARTESIAN_POINT('Ctrl Pts',(-3.18270151782271,4.86884453050484,69.6136128588569));
#57253=CARTESIAN_POINT('Ctrl Pts',(-5.81663740909106,-0.0443313087968929,
69.8919821345872));
#57254=CARTESIAN_POINT('Ctrl Pts',(-3.10812063065928,-4.91678982254146,
70.1703514103174));
#57255=CARTESIAN_POINT('Ctrl Pts',(2.45513612779318,-5.2732857506286,70.4487206860478));
#57256=CARTESIAN_POINT('Ctrl Pts',(5.76340471388584,-0.786385476554853,
70.7270899617779));
#57257=CARTESIAN_POINT('Ctrl Pts',(3.77811368215897,4.42279244578133,71.0054592375083));
#57258=CARTESIAN_POINT('Ctrl Pts',(-1.67729111257008,5.56973343504611,71.2838285132385));
#57259=CARTESIAN_POINT('Ctrl Pts',(-5.5921411585695,1.60099758788418,71.5621977889689));
#57260=CARTESIAN_POINT('Ctrl Pts',(-4.3707333702321,-3.83821909485602,71.840567064699));
#57261=CARTESIAN_POINT('Ctrl Pts',(0.865096242963933,-5.75211652387075,
72.1189363404294));
#57262=CARTESIAN_POINT('Ctrl Pts',(5.30635411174501,-2.38282228765471,72.3973056161595));
#57263=CARTESIAN_POINT('Ctrl Pts',(4.87384322087152,3.17504145990924,72.67567489189));
#57264=CARTESIAN_POINT('Ctrl Pts',(-0.0351847529388852,5.81669992753095,
72.95404416762));
#57265=CARTESIAN_POINT('Ctrl Pts',(-4.91189631022696,3.11584830364957,73.2324134433506));
#57266=CARTESIAN_POINT('Ctrl Pts',(-5.27713986456742,-2.44684099678966,
73.5107827190805));
#57267=CARTESIAN_POINT('Ctrl Pts',(-0.795447298431173,-5.7621610190272,
73.7891519948111));
#57268=CARTESIAN_POINT('Ctrl Pts',(4.41684599871641,-3.78506372963529,74.0675212705412));
#57269=CARTESIAN_POINT('Ctrl Pts',(5.57236404275686,1.66853078747969,74.3458905462716));
#57270=CARTESIAN_POINT('Ctrl Pts',(1.60978909543459,5.58961672049141,74.6242598220017));
#57271=CARTESIAN_POINT('Ctrl Pts',(-3.83134149249159,4.37676345964574,74.9026290977321));
#57272=CARTESIAN_POINT('Ctrl Pts',(-5.75346975218196,-0.856050129668336,
75.1809983734624));
#57273=CARTESIAN_POINT('Ctrl Pts',(-2.39116343640037,-5.30260062933267,
75.4593676491925));
#57274=CARTESIAN_POINT('Ctrl Pts',(3.16737355116417,-4.87882985982939,75.7377369249229));
#57275=CARTESIAN_POINT('Ctrl Pts',(5.81674806318794,0.0260381100804274,
76.016106200653));
#57276=CARTESIAN_POINT('Ctrl Pts',(3.12356827217368,4.90699065241089,76.2944754763835));
#57277=CARTESIAN_POINT('Ctrl Pts',(-2.43853981555445,5.28098092987785,76.5728447521136));
#57278=CARTESIAN_POINT('Ctrl Pts',(-5.76090307624246,0.80450715342832,76.851214027844));
#57279=CARTESIAN_POINT('Ctrl Pts',(-3.79200441789593,-4.41088863024617,
77.1295833035741));
#57280=CARTESIAN_POINT('Ctrl Pts',(1.65976633666211,-5.5749808718471,77.4079525793045));
#57281=CARTESIAN_POINT('Ctrl Pts',(5.58707846113262,-1.61857662250689,77.6863218550347));
#57282=CARTESIAN_POINT('Ctrl Pts',(4.38278272676508,3.82445441648177,77.964691130765));
#57283=CARTESIAN_POINT('Ctrl Pts',(-0.847001899642621,5.75480875405768,
78.2430604064953));
#57284=CARTESIAN_POINT('Ctrl Pts',(-5.2988340353357,2.39949867258681,78.5214296822255));
#57285=CARTESIAN_POINT('Ctrl Pts',(-4.88380443504831,-3.15969781054777,
78.7997989579558));
#57286=CARTESIAN_POINT('Ctrl Pts',(0.0168914028385561,-5.81678181594319,
79.0781682336861));
#57287=CARTESIAN_POINT('Ctrl Pts',(4.90207286122337,-3.13128051714223,79.3565375094163));
#57288=CARTESIAN_POINT('Ctrl Pts',(5.28480893706208,2.43023260461352,79.6349067851467));
#57289=CARTESIAN_POINT('Ctrl Pts',(0.813565019144324,5.75963088864231,79.9132760608768));
#57290=CARTESIAN_POINT('Ctrl Pts',(-4.40492035510159,3.79893572977866,80.1916453366072));
#57291=CARTESIAN_POINT('Ctrl Pts',(-5.57758391584602,-1.65099778178922,
80.4700146123374));
#57292=CARTESIAN_POINT('Ctrl Pts',(-1.62736014737243,-5.58452638676924,
80.7483838880677));
#57293=CARTESIAN_POINT('Ctrl Pts',(3.81755788385611,-4.3887911567066,81.0267531637979));
#57294=CARTESIAN_POINT('Ctrl Pts',(5.75613352618714,0.837951575260477,81.3051224395282));
#57295=CARTESIAN_POINT('Ctrl Pts',(2.40782797560329,5.29505433906766,81.5834917152585));
#57296=CARTESIAN_POINT('Ctrl Pts',(-3.15201425703949,4.88876693422767,81.8618609909888));
#57297=CARTESIAN_POINT('Ctrl Pts',(-5.81680118571323,-0.00774465382969917,
82.1402302667191));
#57298=CARTESIAN_POINT('Ctrl Pts',(-3.13898501948552,-4.89714294882462,
82.4185995424493));
#57299=CARTESIAN_POINT('Ctrl Pts',(2.42191938450794,-5.28862387665468,82.6969688181796));
#57300=CARTESIAN_POINT('Ctrl Pts',(5.75834445937218,-0.822620873182145,
82.9753380939098));
#57301=CARTESIAN_POINT('Ctrl Pts',(3.805857648145,4.39894118803992,83.2537073696402));
#57302=CARTESIAN_POINT('Ctrl Pts',(-1.64222514454274,5.5801731683174,83.5320766453704));
#57303=CARTESIAN_POINT('Ctrl Pts',(-5.58196050371171,1.63613964831234,83.8104459211006));
#57304=CARTESIAN_POINT('Ctrl Pts',(-4.39478873461335,-3.81065191166719,
84.0888151968309));
#57305=CARTESIAN_POINT('Ctrl Pts',(0.828899178899882,-5.75744406529468,
84.3671844725612));
#57306=CARTESIAN_POINT('Ctrl Pts',(5.29126154987468,-2.41615132485442,84.6455537482915));
#57307=CARTESIAN_POINT('Ctrl Pts',(4.89371734509677,3.14432290963829,84.9239230240216));
#57308=CARTESIAN_POINT('Ctrl Pts',(0.00140211432928147,5.81680617245002,
85.2022922997521));
#57309=CARTESIAN_POINT('Ctrl Pts',(-4.8922009274045,3.14668176015314,85.4806615754822));
#57310=CARTESIAN_POINT('Ctrl Pts',(-5.29242573922271,-2.41360017579359,
85.7590308512126));
#57311=CARTESIAN_POINT('Ctrl Pts',(-0.831674693149312,-5.75704379161321,
86.0374001269427));
#57312=CARTESIAN_POINT('Ctrl Pts',(4.39295114384581,-3.81277015587892,86.3157694026731));
#57313=CARTESIAN_POINT('Ctrl Pts',(5.58274862285872,1.6334484466144,86.5941386784033));
#57314=CARTESIAN_POINT('Ctrl Pts',(1.64491510361793,5.5793808183048,86.8725079541337));
#57315=CARTESIAN_POINT('Ctrl Pts',(-3.80373651699164,4.40077544565517,87.1508772298638));
#57316=CARTESIAN_POINT('Ctrl Pts',(-5.75874036813954,-0.819844732944801,
87.4292465055942));
#57317=CARTESIAN_POINT('Ctrl Pts',(-2.42446869975928,-5.28745567713485,
87.7076157813245));
#57318=CARTESIAN_POINT('Ctrl Pts',(3.1366237873624,-4.89865565541509,87.9859850570546));
#57319=CARTESIAN_POINT('Ctrl Pts',(5.81679677614137,-0.0105488790210397,
88.2643543327851));
#57320=CARTESIAN_POINT('Ctrl Pts',(3.15437072011317,4.88724680918305,88.5427236085151));
#57321=CARTESIAN_POINT('Ctrl Pts',(-2.40527499904105,5.29621451536529,88.8210928842456));
#57322=CARTESIAN_POINT('Ctrl Pts',(-5.75572888858148,0.840726456659049,
89.0994621599757));
#57323=CARTESIAN_POINT('Ctrl Pts',(-3.81967323588822,-4.38695023733077,
89.3778314357061));
#57324=CARTESIAN_POINT('Ctrl Pts',(1.62466770970617,-5.58531027310169,89.6562007114362));
#57325=CARTESIAN_POINT('Ctrl Pts',(5.57678733692693,-1.65368649159043,89.9345699871666));
#57326=CARTESIAN_POINT('Ctrl Pts',(4.40675127502924,3.79681171692856,90.2129392628969));
#57327=CARTESIAN_POINT('Ctrl Pts',(-0.810788259783799,5.76002243151662,
90.4913085386271));
#57328=CARTESIAN_POINT('Ctrl Pts',(-5.28363673025889,2.43278007975165,90.7696778143574));
#57329=CARTESIAN_POINT('Ctrl Pts',(-4.90358185297166,-3.12891690924898,
91.0480470900876));
#57330=CARTESIAN_POINT('Ctrl Pts',(-0.0196956176291403,-5.81677299681053,
91.3264163658181));
#57331=CARTESIAN_POINT('Ctrl Pts',(4.88228060641031,-3.16205188035358,91.6047856415481));
#57332=CARTESIAN_POINT('Ctrl Pts',(5.29999019571399,2.3969438748358,91.8831549172785));
#57333=CARTESIAN_POINT('Ctrl Pts',(0.849776141329328,5.75439975352813,92.1615241930086));
#57334=CARTESIAN_POINT('Ctrl Pts',(-4.38093848333281,3.82656687110411,92.4398934687391));
#57335=CARTESIAN_POINT('Ctrl Pts',(-5.5878581127124,-1.61588295552992,92.7182627444692));
#57336=CARTESIAN_POINT('Ctrl Pts',(-1.66245379054078,-5.57418006599121,
92.9966320201996));
#57337=CARTESIAN_POINT('Ctrl Pts',(3.78987752860088,-4.41271620795891,93.2750012959297));
#57338=CARTESIAN_POINT('Ctrl Pts',(5.76129025225566,0.801729781810469,93.5533705716601));
#57339=CARTESIAN_POINT('Ctrl Pts',(2.44108544428034,5.27980471868994,93.8317398473903));
#57340=CARTESIAN_POINT('Ctrl Pts',(-3.12120229435501,4.90849592558558,94.1101091231206));
#57341=CARTESIAN_POINT('Ctrl Pts',(-5.81673483451611,0.0288423075363337,
94.3884783988509));
#57342=CARTESIAN_POINT('Ctrl Pts',(-3.16972522188136,-4.87730233136589,
94.6668476745812));
#57343=CARTESIAN_POINT('Ctrl Pts',(2.38860682377799,-5.30375277093297,94.9452169503114));
#57344=CARTESIAN_POINT('Ctrl Pts',(5.75305638973991,-0.858823724782912,
95.2235862260417));
#57345=CARTESIAN_POINT('Ctrl Pts',(3.83345104448049,4.37491589671717,95.5019555017719));
#57346=CARTESIAN_POINT('Ctrl Pts',(-1.60709420580738,5.59039213539071,95.7803247775023));
#57347=CARTESIAN_POINT('Ctrl Pts',(-5.57155901194447,1.67121697879068,96.0586940532323));
#57348=CARTESIAN_POINT('Ctrl Pts',(-4.41867022969501,-3.78293396915468,
96.3370633289629));
#57349=CARTESIAN_POINT('Ctrl Pts',(0.792669321423524,-5.76254382722172,
96.6154326046929));
#57350=CARTESIAN_POINT('Ctrl Pts',(5.27595965190304,-2.44938477280896,96.8938018804233));
#57351=CARTESIAN_POINT('Ctrl Pts',(4.91339786110621,3.11347996175579,97.1721711561536));
#57352=CARTESIAN_POINT('Ctrl Pts',(0.0379889261259919,5.81668228935273,
97.4505404318838));
#57353=CARTESIAN_POINT('Ctrl Pts',(-4.87231199635946,3.17739072572275,97.7289097076141));
#57354=CARTESIAN_POINT('Ctrl Pts',(-5.30750223171846,-2.38026386648219,
98.0072789833443));
#57355=CARTESIAN_POINT('Ctrl Pts',(-0.867869184648594,-5.75169880053843,
98.2856482590747));
#57356=CARTESIAN_POINT('Ctrl Pts',(4.36888249237581,-3.84032573899534,98.5640175348048));
#57357=CARTESIAN_POINT('Ctrl Pts',(5.59291233487078,1.5983014822703,98.8423868105353));
#57358=CARTESIAN_POINT('Ctrl Pts',(1.67997603467162,5.56892418126753,99.1207560862653));
#57359=CARTESIAN_POINT('Ctrl Pts',(-3.77598105575879,4.42461332551543,99.3991253619959));
#57360=CARTESIAN_POINT('Ctrl Pts',(-5.76378315331532,-0.783606901026482,
99.6774946377258));
#57361=CARTESIAN_POINT('Ctrl Pts',(-2.4576780448157,-5.27210153940609,99.9558639134564));
#57362=CARTESIAN_POINT('Ctrl Pts',(3.10574993054631,-4.91828764741234,100.234233189186));
#57363=CARTESIAN_POINT('Ctrl Pts',(5.81661536145012,-0.0471354507815979,
100.512602464917));
#57364=CARTESIAN_POINT('Ctrl Pts',(3.18504837292365,4.8673096137306,100.790971740647));
#57365=CARTESIAN_POINT('Ctrl Pts',(-2.3719150235782,5.3112385687993,101.069341016377));
#57366=CARTESIAN_POINT('Ctrl Pts',(-5.75032698928046,0.876912498559519,
101.347710292108));
#57367=CARTESIAN_POINT('Ctrl Pts',(-3.8471909376497,-4.36283828522717,101.626079567838));
#57368=CARTESIAN_POINT('Ctrl Pts',(1.58950480666019,-5.5954187049212,101.904448843568));
#57369=CARTESIAN_POINT('Ctrl Pts',(5.56627558047574,-1.68873093652502,102.182818119298));
#57370=CARTESIAN_POINT('Ctrl Pts',(4.43054548072448,3.76901880560565,102.461187395029));
#57371=CARTESIAN_POINT('Ctrl Pts',(-0.774542543027661,5.76500822747185,
102.739556670759));
#57372=CARTESIAN_POINT('Ctrl Pts',(-5.26823039073879,2.46596523979438,103.017925946489));
#57373=CARTESIAN_POINT('Ctrl Pts',(-4.92316527241329,-3.09801221984049,
103.296295222219));
#57374=CARTESIAN_POINT('Ctrl Pts',(-0.0562818588867149,-5.81653405097377,
103.57466449795));
#57375=CARTESIAN_POINT('Ctrl Pts',(4.86229519584828,-3.19269814454921,103.85303377368));
#57376=CARTESIAN_POINT('Ctrl Pts',(5.31496177293694,2.36356031570952,104.13140304941));
#57377=CARTESIAN_POINT('Ctrl Pts',(0.885953644154715,5.74894095935824,104.409772325141));
#57378=CARTESIAN_POINT('Ctrl Pts',(-4.35678329021663,3.85404662346816,104.688141600871));
#57379=CARTESIAN_POINT('Ctrl Pts',(-5.59791123934433,-1.58070420072815,
104.966510876601));
#57380=CARTESIAN_POINT('Ctrl Pts',(-1.69748166270338,-5.56361321611808,
105.244880152331));
#57381=CARTESIAN_POINT('Ctrl Pts',(3.76204723591069,-4.43646668065416,105.523249428062));
#57382=CARTESIAN_POINT('Ctrl Pts',(5.76621904666208,0.765476269840323,105.801618703792));
#57383=CARTESIAN_POINT('Ctrl Pts',(2.47424633725344,5.26434621547303,106.079987979522));
#57384=CARTESIAN_POINT('Ctrl Pts',(-3.0902668487708,4.92803072404851,106.358357255252));
#57385=CARTESIAN_POINT('Ctrl Pts',(-5.81643835812494,0.0654281278253369,
106.636726530983));
#57386=CARTESIAN_POINT('Ctrl Pts',(-3.20034002168381,-4.85726875511187,
106.915095806713));
#57387=CARTESIAN_POINT('Ctrl Pts',(2.35519976353486,-5.31867183492482,107.193465082443));
#57388=CARTESIAN_POINT('Ctrl Pts',(5.74754071419879,-0.894992599078435,
107.471834358174));
#57389=CARTESIAN_POINT('Ctrl Pts',(3.860892779499,4.35071752231632,107.750203633904));
#57390=CARTESIAN_POINT('Ctrl Pts',(-1.57189968623559,5.60038993197703,108.028572909634));
#57391=CARTESIAN_POINT('Ctrl Pts',(-5.56093709477762,1.7062281915686,108.306942185364));
#57392=CARTESIAN_POINT('Ctrl Pts',(-4.44237691066319,-3.75506636391214,
108.585311461095));
#57393=CARTESIAN_POINT('Ctrl Pts',(0.756408103882341,-5.76741560789225,
108.863680736825));
#57394=CARTESIAN_POINT('Ctrl Pts',(5.26044902321342,-2.48252131671617,109.142050012555));
#57395=CARTESIAN_POINT('Ctrl Pts',(4.93288399028696,3.08251383648926,109.420419288285));
#57396=CARTESIAN_POINT('Ctrl Pts',(0.0745742349817975,5.81632828314004,
109.698788564016));
#57397=CARTESIAN_POINT('Ctrl Pts',(-4.85223030394992,3.20797398543193,109.977157839746));
#57398=CARTESIAN_POINT('Ctrl Pts',(-5.32236874558934,-2.34683338772717,
110.255527115476));
#57399=CARTESIAN_POINT('Ctrl Pts',(-0.904029340980253,-5.74612625726445,
110.533896391206));
#57400=CARTESIAN_POINT('Ctrl Pts',(4.34464099652475,-3.86772938881385,110.812265666937));
#57401=CARTESIAN_POINT('Ctrl Pts',(5.60285477669039,1.56309128495284,111.090634942667));
#57402=CARTESIAN_POINT('Ctrl Pts',(1.71497050149349,5.55824722307171,111.369004218397));
#57403=CARTESIAN_POINT('Ctrl Pts',(-3.74807620687148,4.44827615613746,111.647373494127));
#57404=CARTESIAN_POINT('Ctrl Pts',(-5.7685979082034,-0.747338067576144,
111.925742769858));
#57405=CARTESIAN_POINT('Ctrl Pts',(-2.49079015772174,-5.25653882359623,
112.204112045588));
#57406=CARTESIAN_POINT('Ctrl Pts',(3.07475320216653,-4.9377250591284,112.482481321318));
#57407=CARTESIAN_POINT('Ctrl Pts',(5.81620382629126,-0.0837201577406925,
112.760850597049));
#57408=CARTESIAN_POINT('Ctrl Pts',(3.21560001691721,4.84717985482067,113.039219872779));
#57409=CARTESIAN_POINT('Ctrl Pts',(-2.3384612089734,5.3260524957894,113.317589148509));
#57410=CARTESIAN_POINT('Ctrl Pts',(-5.7446975920529,0.913063847515321,113.595958424239));
#57411=CARTESIAN_POINT('Ctrl Pts',(-3.87455643450797,-4.33855372786718,
113.87432769997));
#57412=CARTESIAN_POINT('Ctrl Pts',(1.55427901866009,-5.60530576738952,114.1526969757));
#57413=CARTESIAN_POINT('Ctrl Pts',(5.55554360765141,-1.72370857086153,114.43106625143));
#57414=CARTESIAN_POINT('Ctrl Pts',(4.45416440249025,3.74107678207312,114.70943552716));
#57415=CARTESIAN_POINT('Ctrl Pts',(-0.738266183349346,5.76976594467228,
114.987804802891));
#57416=CARTESIAN_POINT('Ctrl Pts',(-5.2526156262901,2.49905283982359,115.266174078621));
#57417=CARTESIAN_POINT('Ctrl Pts',(-4.94255391860234,-3.06698496499194,
115.544543354351));
#57418=CARTESIAN_POINT('Ctrl Pts',(-0.0928658734872262,-5.81606498788651,
115.822912630082));
#57419=CARTESIAN_POINT('Ctrl Pts',(4.84211742021259,-3.22321809728275,116.101281905812));
#57420=CARTESIAN_POINT('Ctrl Pts',(5.329723076416,2.33008324797548,116.379651181542));
#57421=CARTESIAN_POINT('Ctrl Pts',(0.922096096344309,5.74325472209657,116.658020457272));
#57422=CARTESIAN_POINT('Ctrl Pts',(-4.33245573139553,3.88137389970045,116.936389733003));
#57423=CARTESIAN_POINT('Ctrl Pts',(-5.60774289801398,-1.54546290914759,
117.214759008733));
#57424=CARTESIAN_POINT('Ctrl Pts',(-1.73244237806593,-5.5528262552018,117.493128284463));
#57425=CARTESIAN_POINT('Ctrl Pts',(3.7340681068242,-4.46004163516174,117.771497560194));
#57426=CARTESIAN_POINT('Ctrl Pts',(5.77091971441071,0.72919247363337,118.049866835924));
#57427=CARTESIAN_POINT('Ctrl Pts',(2.50730934259094,5.24867944099596,118.328236111654));
#57428=CARTESIAN_POINT('Ctrl Pts',(-3.05920914417388,4.94737055676852,118.606605387384));
#57429=CARTESIAN_POINT('Ctrl Pts',(-5.81591176826883,0.102011359607224,
118.884974663115));
#57430=CARTESIAN_POINT('Ctrl Pts',(-3.23082820769206,-4.83704301264321,
119.163343938845));
#57431=CARTESIAN_POINT('Ctrl Pts',(2.32169952544947,-5.33338047839311,119.441713214575));
#57432=CARTESIAN_POINT('Ctrl Pts',(5.74179765096292,-0.931126065133631,
119.720082490305));
#57433=CARTESIAN_POINT('Ctrl Pts',(3.88818176753445,4.3263470221884,119.998451766036));
#57434=CARTESIAN_POINT('Ctrl Pts',(-1.53664297821521,5.61016616253672,120.276821041766));
#57435=CARTESIAN_POINT('Ctrl Pts',(-5.55009517244032,1.74117190151289,120.555190317496));
#57436=CARTESIAN_POINT('Ctrl Pts',(-4.46590783962299,-3.72705019845838,
120.833559593227));
#57437=CARTESIAN_POINT('Ctrl Pts',(0.720116960871199,-5.77205921455916,
121.111928868956));
#57438=CARTESIAN_POINT('Ctrl Pts',(5.24473027743382,-2.51555964562078,121.390298144687));
#57439=CARTESIAN_POINT('Ctrl Pts',(4.95217496174117,3.05142575896264,121.668667420417));
#57440=CARTESIAN_POINT('Ctrl Pts',(0.111156593441196,5.81574416777347,121.947036696148));
#57441=CARTESIAN_POINT('Ctrl Pts',(-4.83195664457435,3.23843032941005,122.225405971878));
#57442=CARTESIAN_POINT('Ctrl Pts',(-5.33702469283866,-2.31331006228149,
122.503775247608));
#57443=CARTESIAN_POINT('Ctrl Pts',(-0.940153731250069,-5.74032638196031,
122.782144523338));
#57444=CARTESIAN_POINT('Ctrl Pts',(4.3202276147748,-3.89498002173257,123.060513799069));
#57445=CARTESIAN_POINT('Ctrl Pts',(5.61257555605349,1.52781924872262,123.338883074799));
#57446=CARTESIAN_POINT('Ctrl Pts',(1.74989711756287,5.54735036413612,123.617252350529));
#57447=CARTESIAN_POINT('Ctrl Pts',(-3.72002307044978,4.47176300511463,123.895621626259));
#57448=CARTESIAN_POINT('Ctrl Pts',(-5.77318444962431,-0.711039674576537,
124.17399090199));
#57449=CARTESIAN_POINT('Ctrl Pts',(-2.52380371468285,-5.24076813201426,
124.45236017772));
#57450=CARTESIAN_POINT('Ctrl Pts',(3.04363480249081,-4.95696714685634,124.73072945345));
#57451=CARTESIAN_POINT('Ctrl Pts',(5.8155622361216,-0.120301504763635,125.00909872918));
#57452=CARTESIAN_POINT('Ctrl Pts',(3.24602435053818,4.82685823868056,125.287468004911));
#57453=CARTESIAN_POINT('Ctrl Pts',(-2.30491470342209,5.34065588049586,125.565837280641));
#57454=CARTESIAN_POINT('Ctrl Pts',(-5.7388412506611,0.94917875184084,125.844206556371));
#57455=CARTESIAN_POINT('Ctrl Pts',(-3.90176801872524,-4.31409691905904,
126.122575832102));
#57456=CARTESIAN_POINT('Ctrl Pts',(1.51899055903744,-5.61497221539792,126.400945107832));
#57457=CARTESIAN_POINT('Ctrl Pts',(5.54459407167148,-1.75861584681939,126.679314383562));
#57458=CARTESIAN_POINT('Ctrl Pts',(4.4776028977884,3.71298266576747,126.957683659292));
#57459=CARTESIAN_POINT('Ctrl Pts',(-0.701952670164813,5.77430311013206,
127.236052935023));
#57460=CARTESIAN_POINT('Ctrl Pts',(-5.23680805790664,2.5320270028608,127.514422210753));
#57461=CARTESIAN_POINT('Ctrl Pts',(-4.96171869531289,-3.03580886496632,
127.792791486483));
#57462=CARTESIAN_POINT('Ctrl Pts',(-0.129499705332998,-5.81541776548578,
128.071160762213));
#57463=CARTESIAN_POINT('Ctrl Pts',(4.82184908053961,-3.25351245829232,128.349530037944));
#57464=CARTESIAN_POINT('Ctrl Pts',(5.34408280538262,2.29632880892462,128.627899313674));
#57465=CARTESIAN_POINT('Ctrl Pts',(0.958562204898396,5.73769098457033,128.906268589404));
#57466=CARTESIAN_POINT('Ctrl Pts',(-4.30863698407822,3.9078868970393,129.184637865134));
#57467=CARTESIAN_POINT('Ctrl Pts',(-5.61606665580893,-1.50890976540128,
129.463007140865));
#57468=CARTESIAN_POINT('Ctrl Pts',(-1.7697764369988,-5.54420682019011,129.741376416595));
#57469=CARTESIAN_POINT('Ctrl Pts',(3.71066272797163,-4.47872295434702,130.019745692325));
#57470=CARTESIAN_POINT('Ctrl Pts',(5.42310758321798,-0.17792219993292,130.251720088767));
#57471=CARTESIAN_POINT('Ctrl Pts',(4.16455399126958,2.97569362702242,130.437299605921));
#57472=CARTESIAN_POINT('Ctrl Pts',(2.88487055828799,4.0666809675818,130.530089364497));
#57473=CARTESIAN_POINT('Ctrl Pts',(2.14786219406649,4.42446279878132,130.576484243786));
#57474=CARTESIAN_POINT('Ctrl Pts',(-5.91448192755925,-0.0049507822674949,
128.813375192205));
#57475=CARTESIAN_POINT('Ctrl Pts',(-5.90159134039941,1.44883428144936,128.744968001919));
#57476=CARTESIAN_POINT('Ctrl Pts',(-5.3612661550492,2.91089247196232,128.676560811634));
#57477=CARTESIAN_POINT('Ctrl Pts',(-4.38942716623899,3.98206003052305,128.608153621349));
#57478=CARTESIAN_POINT('Ctrl Pts',(-3.07119285825066,5.43502687128293,128.515363862772));
#57479=CARTESIAN_POINT('Ctrl Pts',(-0.959011980812732,6.16879012277187,
128.422574104195));
#57480=CARTESIAN_POINT('Ctrl Pts',(0.976389493773268,5.84566752435974,128.329784345618));
#57481=CARTESIAN_POINT('Ctrl Pts',(2.91179096835905,5.52254492594765,128.236994587042));
#57482=CARTESIAN_POINT('Ctrl Pts',(4.67041304009307,4.14253647763474,128.144204828465));
#57483=CARTESIAN_POINT('Ctrl Pts',(5.44501452847686,2.33977116576748,128.051415069888));
#57484=CARTESIAN_POINT('Ctrl Pts',(6.21961601686079,0.537005853899908,127.958625311311));
#57485=CARTESIAN_POINT('Ctrl Pts',(6.01019692189429,-1.68851632152195,127.865835552735));
#57486=CARTESIAN_POINT('Ctrl Pts',(4.91272596100818,-3.31494769257717,127.773045794158));
#57487=CARTESIAN_POINT('Ctrl Pts',(3.81525500012219,-4.94137906363219,127.680256035581));
#57488=CARTESIAN_POINT('Ctrl Pts',(1.8297321733167,-5.96871963032048,127.587466277004));
#57489=CARTESIAN_POINT('Ctrl Pts',(-0.131904744888432,-5.92506935716104,
127.494676518428));
#57490=CARTESIAN_POINT('Ctrl Pts',(-2.09354166309357,-5.88141908400161,
127.401886759851));
#57491=CARTESIAN_POINT('Ctrl Pts',(-4.03129267269846,-4.76677797099448,
127.309097001274));
#57492=CARTESIAN_POINT('Ctrl Pts',(-5.05532448262752,-3.09308835127519,
127.216307242697));
#57493=CARTESIAN_POINT('Ctrl Pts',(-5.6179127354129,-2.17358750205046,127.165329892533));
#57494=CARTESIAN_POINT('Ctrl Pts',(-5.90471818937535,-1.08535214236168,
127.114352542369));
#57495=CARTESIAN_POINT('Ctrl Pts',(-5.90733548964813,0.0015994485885984,
127.063375192205));
#57496=CARTESIAN_POINT('Origin',(0.,0.,-10.));
#57497=CARTESIAN_POINT('Origin',(-9.00000000000001,-15.5884572681199,169.));
#57498=CARTESIAN_POINT('',(-12.,-15.5884572681199,174.));
#57499=CARTESIAN_POINT('Origin',(-9.00000000000001,-15.5884572681199,174.));
#57500=CARTESIAN_POINT('',(-12.,-15.5884572681199,164.));
#57501=CARTESIAN_POINT('',(-12.,-15.5884572681199,169.));
#57502=CARTESIAN_POINT('Origin',(-9.00000000000001,-15.5884572681199,164.));
#57503=CARTESIAN_POINT('Origin',(-9.,15.5884572681199,169.));
#57504=CARTESIAN_POINT('',(-12.,15.5884572681199,174.));
#57505=CARTESIAN_POINT('Origin',(-9.,15.5884572681199,174.));
#57506=CARTESIAN_POINT('',(-12.,15.5884572681199,164.));
#57507=CARTESIAN_POINT('',(-12.,15.5884572681199,169.));
#57508=CARTESIAN_POINT('Origin',(-9.,15.5884572681199,164.));
#57509=CARTESIAN_POINT('Origin',(18.,0.,169.));
#57510=CARTESIAN_POINT('',(15.,3.67394039744206E-16,174.));
#57511=CARTESIAN_POINT('Origin',(18.,0.,174.));
#57512=CARTESIAN_POINT('',(15.,3.67394039744206E-16,164.));
#57513=CARTESIAN_POINT('',(15.,3.67394039744206E-16,169.));
#57514=CARTESIAN_POINT('Origin',(18.,0.,164.));
#57515=CARTESIAN_POINT('Origin',(9.,15.5884572681199,169.));
#57516=CARTESIAN_POINT('',(6.,15.5884572681199,174.));
#57517=CARTESIAN_POINT('Origin',(9.,15.5884572681199,174.));
#57518=CARTESIAN_POINT('',(6.,15.5884572681199,164.));
#57519=CARTESIAN_POINT('',(6.,15.5884572681199,169.));
#57520=CARTESIAN_POINT('Origin',(9.,15.5884572681199,164.));
#57521=CARTESIAN_POINT('Origin',(-18.,2.20436423846524E-15,169.));
#57522=CARTESIAN_POINT('',(-21.,2.57175827820944E-15,174.));
#57523=CARTESIAN_POINT('Origin',(-18.,2.20436423846524E-15,174.));
#57524=CARTESIAN_POINT('',(-21.,2.57175827820944E-15,164.));
#57525=CARTESIAN_POINT('',(-21.,2.57175827820944E-15,169.));
#57526=CARTESIAN_POINT('Origin',(-18.,2.20436423846524E-15,164.));
#57527=CARTESIAN_POINT('Origin',(9.,-15.5884572681199,169.));
#57528=CARTESIAN_POINT('',(6.,-15.5884572681199,174.));
#57529=CARTESIAN_POINT('Origin',(9.,-15.5884572681199,174.));
#57530=CARTESIAN_POINT('',(6.,-15.5884572681199,164.));
#57531=CARTESIAN_POINT('',(6.,-15.5884572681199,169.));
#57532=CARTESIAN_POINT('Origin',(9.,-15.5884572681199,164.));
#57533=CARTESIAN_POINT('Origin',(0.,0.,164.));
#57534=CARTESIAN_POINT('',(-25.,-3.06161699786838E-15,164.));
#57535=CARTESIAN_POINT('Origin',(0.,0.,164.));
#57536=CARTESIAN_POINT('',(-12.,-1.46957615897682E-15,164.));
#57537=CARTESIAN_POINT('Origin',(0.,0.,164.));
#57538=CARTESIAN_POINT('Origin',(0.,0.,164.));
#57539=CARTESIAN_POINT('',(-25.,-3.06161699786838E-15,174.));
#57540=CARTESIAN_POINT('Origin',(0.,0.,174.));
#57541=CARTESIAN_POINT('',(-25.,-3.06161699786838E-15,164.));
#57542=CARTESIAN_POINT('Origin',(0.,0.,174.));
#57543=CARTESIAN_POINT('Origin',(0.,0.,162.));
#57544=CARTESIAN_POINT('',(-12.,-1.46957615897682E-15,162.));
#57545=CARTESIAN_POINT('Origin',(0.,0.,162.));
#57546=CARTESIAN_POINT('Origin',(0.,0.,162.));
#57547=CARTESIAN_POINT('',(-12.,-1.46957615897682E-15,162.));
#57548=CARTESIAN_POINT('',(0.,0.,0.));
#57549=CARTESIAN_POINT('Origin',(0.,0.,0.));
#57550=CARTESIAN_POINT('',(-6.,-7.34788079488412E-16,10.));
#57551=CARTESIAN_POINT('Origin',(0.,0.,10.));
#57552=CARTESIAN_POINT('',(-6.,-7.34788079488412E-16,0.));
#57553=CARTESIAN_POINT('',(-6.,-7.34788079488412E-16,0.));
#57554=CARTESIAN_POINT('Origin',(0.,0.,0.));
#57555=CARTESIAN_POINT('Origin',(0.,0.,0.));
#57556=CARTESIAN_POINT('',(-8.,-9.79717439317883E-16,10.));
#57557=CARTESIAN_POINT('Origin',(0.,0.,10.));
#57558=CARTESIAN_POINT('',(-8.,-9.79717439317883E-16,0.));
#57559=CARTESIAN_POINT('',(-8.,-9.79717439317883E-16,0.));
#57560=CARTESIAN_POINT('Origin',(0.,0.,0.));
#57561=CARTESIAN_POINT('Origin',(0.,0.,10.));
#57562=CARTESIAN_POINT('Origin',(0.,0.,0.));
#57563=CARTESIAN_POINT('',(0.,0.,0.));
#57564=CARTESIAN_POINT('Origin',(-1.,0.,1.));
#57565=CARTESIAN_POINT('',(-1.,4.89897948556636,0.));
#57566=CARTESIAN_POINT('',(-1.,4.89897948556636,1.));
#57567=CARTESIAN_POINT('',(-1.,4.89897948556636,0.));
#57568=CARTESIAN_POINT('',(-1.,10.9544511501033,0.));
#57569=CARTESIAN_POINT('',(-1.,0.,0.));
#57570=CARTESIAN_POINT('',(-1.,10.9544511501033,1.));
#57571=CARTESIAN_POINT('',(-1.,10.9544511501033,0.));
#57572=CARTESIAN_POINT('',(-1.,0.,1.));
#57573=CARTESIAN_POINT('Origin',(1.,22.,1.));
#57574=CARTESIAN_POINT('',(1.,4.89897948556636,1.));
#57575=CARTESIAN_POINT('',(1.,4.89897948556636,0.));
#57576=CARTESIAN_POINT('',(1.,4.89897948556636,0.));
#57577=CARTESIAN_POINT('',(1.,10.9544511501033,1.));
#57578=CARTESIAN_POINT('',(1.,11.,1.));
#57579=CARTESIAN_POINT('',(1.,10.9544511501033,0.));
#57580=CARTESIAN_POINT('',(1.,10.9544511501033,0.));
#57581=CARTESIAN_POINT('',(1.,11.,0.));
#57582=CARTESIAN_POINT('Origin',(0.,0.,0.));
#57583=CARTESIAN_POINT('Origin',(0.,0.,0.));
#57584=CARTESIAN_POINT('Origin',(0.,0.,0.));
#57585=CARTESIAN_POINT('Origin',(0.,0.,0.));
#57586=CARTESIAN_POINT('Origin',(0.,0.,1.));
#57587=CARTESIAN_POINT('Origin',(0.,0.,0.));
#57588=CARTESIAN_POINT('Origin',(0.,0.,1.));
#57589=CARTESIAN_POINT('Origin',(0.,0.,1.));
#57590=CARTESIAN_POINT('',(0.,0.,0.));
#57591=CARTESIAN_POINT('Origin',(0.,0.,0.));
#57592=CARTESIAN_POINT('',(-2.94501217978886,0.00210964666656384,0.322176117089595));
#57593=CARTESIAN_POINT('',(-2.94453553094506,0.00313791388557197,0.177823882910385));
#57594=CARTESIAN_POINT('',(-2.942,-3.60291088309151E-16,0.));
#57595=CARTESIAN_POINT('',(1.28892185405323,2.64462557919717,0.));
#57596=CARTESIAN_POINT('Ctrl Pts',(-2.94501217978886,0.00210964666656384,
0.322176117089595));
#57597=CARTESIAN_POINT('Ctrl Pts',(-2.94591259769569,0.121087549437314,
0.315720264862594));
#57598=CARTESIAN_POINT('Ctrl Pts',(-2.93932205372645,0.239959279025233,
0.309264412635592));
#57599=CARTESIAN_POINT('Ctrl Pts',(-2.92490373823147,0.357866546097276,
0.302808560408591));
#57600=CARTESIAN_POINT('Ctrl Pts',(-2.80727159362702,1.31981558202748,0.250138347790759));
#57601=CARTESIAN_POINT('Ctrl Pts',(-2.16861137772223,2.21756856383993,0.197468135172927));
#57602=CARTESIAN_POINT('Ctrl Pts',(-1.29846211955926,2.64493763974705,0.144797922555096));
#57603=CARTESIAN_POINT('Ctrl Pts',(-0.501074003123223,3.03657047660083,
0.0965319483700637));
#57604=CARTESIAN_POINT('Ctrl Pts',(0.490707930428614,3.03319661211455,0.048265974185032));
#57605=CARTESIAN_POINT('Ctrl Pts',(1.29200466145509,2.64817921559509,2.28251534084349E-16));
#57606=CARTESIAN_POINT('',(-1.2889218540533,2.64462557919714,0.));
#57607=CARTESIAN_POINT('Origin',(0.,0.,0.));
#57608=CARTESIAN_POINT('Ctrl Pts',(-1.2889218540533,2.64462557919714,3.2612801348364E-15));
#57609=CARTESIAN_POINT('Ctrl Pts',(-2.16412553195878,2.21807402646555,0.0526702126178337));
#57610=CARTESIAN_POINT('Ctrl Pts',(-2.80369899883776,1.32688596224183,0.105340425235664));
#57611=CARTESIAN_POINT('Ctrl Pts',(-2.92359275294276,0.366672953034089,
0.158010637853495));
#57612=CARTESIAN_POINT('Ctrl Pts',(-2.93862645170598,0.246270074362799,
0.164615052872458));
#57613=CARTESIAN_POINT('Ctrl Pts',(-2.94548916698122,0.12478190859667,0.171219467891421));
#57614=CARTESIAN_POINT('Ctrl Pts',(-2.94453553094506,0.00313791388557197,
0.177823882910385));
#57615=CARTESIAN_POINT('Origin',(0.,0.,0.));
#57616=CARTESIAN_POINT('',(-2.9374626214221,0.000758590818191462,1.3221761170896));
#57617=CARTESIAN_POINT('',(-2.93743561631178,0.000732401129134809,1.17782388291039));
#57618=CARTESIAN_POINT('',(-2.942,-3.60291088309151E-16,0.));
#57619=CARTESIAN_POINT('Ctrl Pts',(-2.9374626214221,0.000758590818191462,
1.3221761170896));
#57620=CARTESIAN_POINT('Ctrl Pts',(-2.93848585913829,0.441702582020672,
1.29840820723625));
#57621=CARTESIAN_POINT('Ctrl Pts',(-2.84537551923226,0.882235445407197,
1.2746402973829));
#57622=CARTESIAN_POINT('Ctrl Pts',(-2.65590902315621,1.27645657866303,1.25087238752956));
#57623=CARTESIAN_POINT('Ctrl Pts',(-2.23604708772076,2.15005930751655,1.19820217491173));
#57624=CARTESIAN_POINT('Ctrl Pts',(-1.34300379394444,2.79623653247501,1.1455319622939));
#57625=CARTESIAN_POINT('Ctrl Pts',(-0.381914565919547,2.92186465652728,
1.09286174967606));
#57626=CARTESIAN_POINT('Ctrl Pts',(0.579174662105351,3.04749278057955,1.04019153705823));
#57627=CARTESIAN_POINT('Ctrl Pts',(1.60830982437882,2.65257180372564,0.987521324440401));
#57628=CARTESIAN_POINT('Ctrl Pts',(2.23860403446081,1.91621978819862,0.93485111182257));
#57629=CARTESIAN_POINT('Ctrl Pts',(2.8688982445428,1.17986777267159,0.882180899204738));
#57630=CARTESIAN_POINT('Ctrl Pts',(3.1003515024333,0.102084718471448,0.829510686586907));
#57631=CARTESIAN_POINT('Ctrl Pts',(2.82797713905364,-0.828099512194974,
0.776840473969075));
#57632=CARTESIAN_POINT('Ctrl Pts',(2.55560277567399,-1.7582837428614,0.724170261351243));
#57633=CARTESIAN_POINT('Ctrl Pts',(1.77940079102417,-2.5408691499941,0.671500048733411));
#57634=CARTESIAN_POINT('Ctrl Pts',(0.851475992729512,-2.82098153902745,
0.61882983611558));
#57635=CARTESIAN_POINT('Ctrl Pts',(-0.0764488055651469,-3.1010939280608,
0.566159623497748));
#57636=CARTESIAN_POINT('Ctrl Pts',(-1.15609641750466,-2.8787332989948,0.513489410879917));
#57637=CARTESIAN_POINT('Ctrl Pts',(-1.89761818682235,-2.25448043943784,
0.460819198262086));
#57638=CARTESIAN_POINT('Ctrl Pts',(-2.54825072809468,-1.70674301456925,
0.414604837871256));
#57639=CARTESIAN_POINT('Ctrl Pts',(-2.93856651836649,-0.849596291427123,
0.368390477480426));
#57640=CARTESIAN_POINT('Ctrl Pts',(-2.94501217978886,0.00210964666656384,
0.322176117089595));
#57641=CARTESIAN_POINT('Ctrl Pts',(-2.94453553094506,0.00313791388557197,
0.177823882910385));
#57642=CARTESIAN_POINT('Ctrl Pts',(-2.93788391918254,-0.845329001562565,
0.223889680509253));
#57643=CARTESIAN_POINT('Ctrl Pts',(-2.55096188398631,-1.70137709351185,
0.269955478108122));
#57644=CARTESIAN_POINT('Ctrl Pts',(-1.90410965994752,-2.24960573227557,
0.31602127570699));
#57645=CARTESIAN_POINT('Ctrl Pts',(-1.16451877151628,-2.87643345418565,
0.368691488324821));
#57646=CARTESIAN_POINT('Ctrl Pts',(-0.0851229533228073,-3.10085094381401,
0.421361700942653));
#57647=CARTESIAN_POINT('Ctrl Pts',(0.843672564211012,-2.82310443536429,
0.474031913560484));
#57648=CARTESIAN_POINT('Ctrl Pts',(1.77246808174483,-2.54535792691456,0.526702126178316));
#57649=CARTESIAN_POINT('Ctrl Pts',(2.550663298619,-1.76544742038675,0.579372338796147));
#57650=CARTESIAN_POINT('Ctrl Pts',(2.82559485726556,-0.836148642972677,
0.632042551413979));
#57651=CARTESIAN_POINT('Ctrl Pts',(3.10052641591212,0.0931501344413926,
0.684712764031811));
#57652=CARTESIAN_POINT('Ctrl Pts',(2.87219431633107,1.17183718274172,0.737382976649643));
#57653=CARTESIAN_POINT('Ctrl Pts',(2.24398891012547,1.91001338469769,0.790053189267474));
#57654=CARTESIAN_POINT('Ctrl Pts',(1.61578350391986,2.64818958665366,0.842723401885306));
#57655=CARTESIAN_POINT('Ctrl Pts',(0.587704791089698,3.04585494226529,0.895393614503137));
#57656=CARTESIAN_POINT('Ctrl Pts',(-0.373745257291813,2.92288626672173,
0.948063827120969));
#57657=CARTESIAN_POINT('Ctrl Pts',(-1.33519530567332,2.79991759117817,1.0007340397388));
#57658=CARTESIAN_POINT('Ctrl Pts',(-2.23001668960618,2.15631488447943,1.05340425235663));
#57659=CARTESIAN_POINT('Ctrl Pts',(-2.65231672176365,1.28390825032342,1.10607446497446));
#57660=CARTESIAN_POINT('Ctrl Pts',(-2.84407458005236,0.887766135751567,
1.12999093761977));
#57661=CARTESIAN_POINT('Ctrl Pts',(-2.93840404300437,0.444447318126731,
1.15390741026508));
#57662=CARTESIAN_POINT('Ctrl Pts',(-2.93743561631178,0.000732401129134809,
1.17782388291039));
#57663=CARTESIAN_POINT('Origin',(0.,0.,0.));
#57664=CARTESIAN_POINT('',(-2.94237337112349,-0.00260076937561138,2.32217611708959));
#57665=CARTESIAN_POINT('',(-2.94245565671171,-0.00259425957205793,2.17782388291038));
#57666=CARTESIAN_POINT('',(-2.942,-3.60291088309151E-16,0.));
#57667=CARTESIAN_POINT('Ctrl Pts',(-2.94237337112349,-0.00260076937561138,
2.32217611708959));
#57668=CARTESIAN_POINT('Ctrl Pts',(-2.93547687785472,0.756299906403093,
2.28109614960991));
#57669=CARTESIAN_POINT('Ctrl Pts',(-2.63517458379537,1.52004621893047,2.24001618213022));
#57670=CARTESIAN_POINT('Ctrl Pts',(-2.10656451366312,2.06047930091946,2.19893621465053));
#57671=CARTESIAN_POINT('Ctrl Pts',(-1.4288131303506,2.75338942428174,2.1462660020327));
#57672=CARTESIAN_POINT('Ctrl Pts',(-0.375751290551719,3.07919952181725,
2.09359578941486));
#57673=CARTESIAN_POINT('Ctrl Pts',(0.57488733383408,2.89010251009112,2.04092557679703));
#57674=CARTESIAN_POINT('Ctrl Pts',(1.52552595821988,2.70100549836499,1.9882553641792));
#57675=CARTESIAN_POINT('Ctrl Pts',(2.3737413671926,1.99700137737721,1.93558515156137));
#57676=CARTESIAN_POINT('Ctrl Pts',(2.73473061221906,1.09746893276964,1.88291493894354));
#57677=CARTESIAN_POINT('Ctrl Pts',(3.09571985724552,0.197936488162073,1.83024472632571));
#57678=CARTESIAN_POINT('Ctrl Pts',(2.96948293832572,-0.897124280065286,
1.77757451370788));
#57679=CARTESIAN_POINT('Ctrl Pts',(2.41328900736074,-1.69092464359517,1.72490430109004));
#57680=CARTESIAN_POINT('Ctrl Pts',(1.85709507639575,-2.48472500712505,1.67223408847221));
#57681=CARTESIAN_POINT('Ctrl Pts',(0.870944133385572,-2.97726496595745,
1.61956387585438));
#57682=CARTESIAN_POINT('Ctrl Pts',(-0.0977855553122216,-2.94510122718995,
1.56689366323655));
#57683=CARTESIAN_POINT('Ctrl Pts',(-1.06651524401001,-2.91293748842246,
1.51422345061872));
#57684=CARTESIAN_POINT('Ctrl Pts',(-2.01782367839542,-2.35607005205505,
1.46155323800089));
#57685=CARTESIAN_POINT('Ctrl Pts',(-2.52013760704083,-1.52712221749706,
1.40888302538305));
#57686=CARTESIAN_POINT('Ctrl Pts',(-2.79577783188422,-1.07224459123419,
1.37998072261857));
#57687=CARTESIAN_POINT('Ctrl Pts',(-2.93621834178389,-0.535439030872177,
1.35107841985408));
#57688=CARTESIAN_POINT('Ctrl Pts',(-2.9374626214221,0.000758590818191462,
1.3221761170896));
#57689=CARTESIAN_POINT('Ctrl Pts',(-2.93743561631178,0.000732401129134809,
1.17782388291039));
#57690=CARTESIAN_POINT('Ctrl Pts',(-2.93627131881214,-0.532726839892435,
1.20657762288291));
#57691=CARTESIAN_POINT('Ctrl Pts',(-2.79736142917079,-1.06675861135357,
1.23533136285543));
#57692=CARTESIAN_POINT('Ctrl Pts',(-2.52440827067989,-1.5200691062172,1.26408510282796));
#57693=CARTESIAN_POINT('Ctrl Pts',(-2.02442110705658,-2.35042926698854,
1.31675531544579));
#57694=CARTESIAN_POINT('Ctrl Pts',(-1.07466809942789,-2.90993902691792,
1.36942552806362));
#57695=CARTESIAN_POINT('Ctrl Pts',(-0.10603039660911,-2.94481076457264,
1.42209574068145));
#57696=CARTESIAN_POINT('Ctrl Pts',(0.862607306209672,-2.97968250222737,
1.47476595329928));
#57697=CARTESIAN_POINT('Ctrl Pts',(1.85012970421854,-2.48991621760742,1.52743616591712));
#57698=CARTESIAN_POINT('Ctrl Pts',(2.40854344014417,-1.69767888635459,1.58010637853495));
#57699=CARTESIAN_POINT('Ctrl Pts',(2.96695717606981,-0.905441555101753,
1.63277659115278));
#57700=CARTESIAN_POINT('Ctrl Pts',(3.09626224991221,0.189266822783965,1.68544680377061));
#57701=CARTESIAN_POINT('Ctrl Pts',(2.73779389621599,1.08980795795695,1.73811701638844));
#57702=CARTESIAN_POINT('Ctrl Pts',(2.37932554251976,1.99034909312994,1.79078722900627));
#57703=CARTESIAN_POINT('Ctrl Pts',(1.53308376128489,2.6967229855902,1.8434574416241));
#57704=CARTESIAN_POINT('Ctrl Pts',(0.582978083752645,2.88848071032948,1.89612765424194));
#57705=CARTESIAN_POINT('Ctrl Pts',(-0.367127593779598,3.08023843506875,
1.94879786685977));
#57706=CARTESIAN_POINT('Ctrl Pts',(-1.42109716760921,2.75737999208705,2.0014680794776));
#57707=CARTESIAN_POINT('Ctrl Pts',(-2.10078617833213,2.06637082890199,2.05413829209543));
#57708=CARTESIAN_POINT('Ctrl Pts',(-2.63282464108198,1.5254713187922,2.09536682236708));
#57709=CARTESIAN_POINT('Ctrl Pts',(-2.93553206539509,0.758996677917738,
2.13659535263873));
#57710=CARTESIAN_POINT('Ctrl Pts',(-2.94245565671171,-0.00259425957205793,
2.17782388291038));
#57711=CARTESIAN_POINT('Origin',(0.,0.,0.));
#57712=CARTESIAN_POINT('',(-2.94537017639144,0.00174029209860913,3.3221761170896));
#57713=CARTESIAN_POINT('',(-2.94530715728325,0.00177620926833399,3.17782388291039));
#57714=CARTESIAN_POINT('',(-2.942,-3.60291088309151E-16,0.));
#57715=CARTESIAN_POINT('Ctrl Pts',(-2.94537017639144,0.00174029209860913,
3.3221761170896));
#57716=CARTESIAN_POINT('Ctrl Pts',(-2.94611224026602,0.107164636136391,
3.31645430460139));
#57717=CARTESIAN_POINT('Ctrl Pts',(-2.94093746113258,0.212515376889504,
3.31073249211319));
#57718=CARTESIAN_POINT('Ctrl Pts',(-2.9296029501889,0.317199180230514,3.30501067962499));
#57719=CARTESIAN_POINT('Ctrl Pts',(-2.82526693733401,1.28083058041764,3.25234046700716));
#57720=CARTESIAN_POINT('Ctrl Pts',(-2.19898596937906,2.18794903031096,3.19967025438933));
#57721=CARTESIAN_POINT('Ctrl Pts',(-1.33487969482344,2.62702968627763,3.1470000417715));
#57722=CARTESIAN_POINT('Ctrl Pts',(-0.470773420267829,3.06611034224429,
3.09432982915367));
#57723=CARTESIAN_POINT('Ctrl Pts',(0.631158160888449,3.03715320428431,3.04165961653583));
#57724=CARTESIAN_POINT('Ctrl Pts',(1.47101096812166,2.55329502437494,2.988989403918));
#57725=CARTESIAN_POINT('Ctrl Pts',(2.31086377535488,2.06943684446558,2.93631919130017));
#57726=CARTESIAN_POINT('Ctrl Pts',(2.88863780866502,1.13067762260682,2.88364897868234));
#57727=CARTESIAN_POINT('Ctrl Pts',(2.94221915242109,0.162896383790171,2.83097876606451));
#57728=CARTESIAN_POINT('Ctrl Pts',(2.99580049617715,-0.804884855026484,
2.77830855344668));
#57729=CARTESIAN_POINT('Ctrl Pts',(2.52518915037914,-1.80168811080104,2.72563834082884));
#57730=CARTESIAN_POINT('Ctrl Pts',(1.74388343367472,-2.37530195478797,2.67296812821101));
#57731=CARTESIAN_POINT('Ctrl Pts',(0.962577716970292,-2.94891579877489,
2.62029791559318));
#57732=CARTESIAN_POINT('Ctrl Pts',(-0.129422370640539,-3.09934023097417,
2.56762770297535));
#57733=CARTESIAN_POINT('Ctrl Pts',(-1.03671829650871,-2.75833352334838,
2.51495749035752));
#57734=CARTESIAN_POINT('Ctrl Pts',(-1.94401422237688,-2.4173268157226,2.46228727773969));
#57735=CARTESIAN_POINT('Ctrl Pts',(-2.66660598650239,-1.58488896827175,
2.40961706512185));
#57736=CARTESIAN_POINT('Ctrl Pts',(-2.87668140515208,-0.638664969951807,
2.35694685250402));
#57737=CARTESIAN_POINT('Ctrl Pts',(-2.92290915853737,-0.430445417551361,
2.34535660736588));
#57738=CARTESIAN_POINT('Ctrl Pts',(-2.94431913818423,-0.216715955131923,
2.33376636222774));
#57739=CARTESIAN_POINT('Ctrl Pts',(-2.94237337112349,-0.00260076937561138,
2.32217611708959));
#57740=CARTESIAN_POINT('Ctrl Pts',(-2.94245565671171,-0.00259425957205793,
2.17782388291038));
#57741=CARTESIAN_POINT('Ctrl Pts',(-2.94437708180297,-0.213949879747532,
2.18926556525656));
#57742=CARTESIAN_POINT('Ctrl Pts',(-2.92351825621533,-0.424929373931882,
2.20070724760275));
#57743=CARTESIAN_POINT('Ctrl Pts',(-2.87845884965989,-0.630607025085498,
2.21214892994893));
#57744=CARTESIAN_POINT('Ctrl Pts',(-2.67103406264848,-1.57741583249951,
2.26481914256676));
#57745=CARTESIAN_POINT('Ctrl Pts',(-1.95077604100943,-2.4118735639391,2.31748935518459));
#57746=CARTESIAN_POINT('Ctrl Pts',(-1.04443851765628,-2.75541959458595,
2.37015956780242));
#57747=CARTESIAN_POINT('Ctrl Pts',(-0.138100994303129,-3.0989656252328,
2.42282978042025));
#57748=CARTESIAN_POINT('Ctrl Pts',(0.954316030764116,-2.95159995508691,
2.47549999303808));
#57749=CARTESIAN_POINT('Ctrl Pts',(1.73722502222407,-2.38017629855023,2.52817020565592));
#57750=CARTESIAN_POINT('Ctrl Pts',(2.52013401368403,-1.80875264201355,2.58084041827375));
#57751=CARTESIAN_POINT('Ctrl Pts',(2.9935349715367,-0.81327099908608,2.63351063089158));
#57752=CARTESIAN_POINT('Ctrl Pts',(2.94266396081319,0.154656572499768,2.68618084350941));
#57753=CARTESIAN_POINT('Ctrl Pts',(2.89179295008968,1.12258414408561,2.73885105612724));
#57754=CARTESIAN_POINT('Ctrl Pts',(2.31664997079,2.06295764432982,2.79152126874507));
#57755=CARTESIAN_POINT('Ctrl Pts',(1.47815537025573,2.54916581364531,2.8441914813629));
#57756=CARTESIAN_POINT('Ctrl Pts',(0.639660769721456,3.03537398296079,2.89686169398074));
#57757=CARTESIAN_POINT('Ctrl Pts',(-0.462185452047399,3.06741682134755,
2.94953190659857));
#57758=CARTESIAN_POINT('Ctrl Pts',(-1.32751795973283,2.63075765975438,3.0022021192164));
#57759=CARTESIAN_POINT('Ctrl Pts',(-2.19285046741827,2.19409849816122,3.05487233183423));
#57760=CARTESIAN_POINT('Ctrl Pts',(-2.82166926102029,1.28873733658814,3.10754254445206));
#57761=CARTESIAN_POINT('Ctrl Pts',(-2.92870336695306,0.325401832213201,
3.1602127570699));
#57762=CARTESIAN_POINT('Ctrl Pts',(-2.94063288723355,0.218032967530236,
3.16608313235006));
#57763=CARTESIAN_POINT('Ctrl Pts',(-2.9460806479325,0.109943928873562,3.17195350763022));
#57764=CARTESIAN_POINT('Ctrl Pts',(-2.94530715728325,0.00177620926833399,
3.17782388291039));
#57765=CARTESIAN_POINT('Origin',(0.,0.,0.));
#57766=CARTESIAN_POINT('',(-2.93758307183925,0.000962932756501389,4.32217611708959));
#57767=CARTESIAN_POINT('',(-2.93755662075233,0.00092146372069949,4.17782388291039));
#57768=CARTESIAN_POINT('',(-2.942,-3.60291088309151E-16,0.));
#57769=CARTESIAN_POINT('Ctrl Pts',(-2.93758307183925,0.000962932756501389,
4.32217611708959));
#57770=CARTESIAN_POINT('Ctrl Pts',(-2.93884998778206,0.428244162000401,
4.29914224697505));
#57771=CARTESIAN_POINT('Ctrl Pts',(-2.85162805316606,0.855032782237186,
4.2761083768605));
#57772=CARTESIAN_POINT('Ctrl Pts',(-2.67331627298244,1.23958415202432,4.25307450674596));
#57773=CARTESIAN_POINT('Ctrl Pts',(-2.26558108441747,2.11891542846389,4.20040429412813));
#57774=CARTESIAN_POINT('Ctrl Pts',(-1.38156157854408,2.77739947577446,4.1477340815103));
#57775=CARTESIAN_POINT('Ctrl Pts',(-0.422303489371249,2.91630734463971,
4.09506386889247));
#57776=CARTESIAN_POINT('Ctrl Pts',(0.536954599801574,3.05521521350496,4.04239365627464));
#57777=CARTESIAN_POINT('Ctrl Pts',(1.57145127227383,2.6745469039249,3.9897234436568));
#57778=CARTESIAN_POINT('Ctrl Pts',(2.21187507673207,1.94699702363172,3.93705323103897));
#57779=CARTESIAN_POINT('Ctrl Pts',(2.8522988811903,1.21944714333852,3.88438301842114));
#57780=CARTESIAN_POINT('Ctrl Pts',(3.0986498176345,0.145015692332194,3.83171280580331));
#57781=CARTESIAN_POINT('Ctrl Pts',(2.83916791750172,-0.788869001505497,
3.77904259318548));
#57782=CARTESIAN_POINT('Ctrl Pts',(2.57968601736894,-1.72275369534319,3.72637238056765));
#57783=CARTESIAN_POINT('Ctrl Pts',(1.81437128065917,-2.51609163201224,3.67370216794981));
#57784=CARTESIAN_POINT('Ctrl Pts',(0.890417641887139,-2.80897582571963,
3.62103195533198));
#57785=CARTESIAN_POINT('Ctrl Pts',(-0.0335359968848904,-3.10186001942701,
3.56836174271415));
#57786=CARTESIAN_POINT('Ctrl Pts',(-1.11612853771918,-2.89429047017273,
3.51569153009632));
#57787=CARTESIAN_POINT('Ctrl Pts',(-1.86622927925891,-2.28043352030513,
3.46302131747849));
#57788=CARTESIAN_POINT('Ctrl Pts',(-2.53484305545271,-1.73326273301688,
3.41607291734886));
#57789=CARTESIAN_POINT('Ctrl Pts',(-2.93928142186174,-0.863283561356046,
3.36912451721922));
#57790=CARTESIAN_POINT('Ctrl Pts',(-2.94537017639144,0.00174029209860913,
3.3221761170896));
#57791=CARTESIAN_POINT('Ctrl Pts',(-2.94530715728325,0.00177620926833399,
3.17782388291039));
#57792=CARTESIAN_POINT('Ctrl Pts',(-2.93914073097497,-0.860559065925464,
3.22462372024805));
#57793=CARTESIAN_POINT('Ctrl Pts',(-2.53757609018917,-1.72789499208641,
3.27142355758572));
#57794=CARTESIAN_POINT('Ctrl Pts',(-1.87260805478389,-2.27519863184659,
3.31822339492339));
#57795=CARTESIAN_POINT('Ctrl Pts',(-1.1242292184184,-2.89115374435464,3.37089360754122));
#57796=CARTESIAN_POINT('Ctrl Pts',(-0.0422221274238752,-3.10175412219396,
3.42356382015905));
#57797=CARTESIAN_POINT('Ctrl Pts',(0.882548115976509,-2.81145844473756,
3.47623403277689));
#57798=CARTESIAN_POINT('Ctrl Pts',(1.80731835937689,-2.52116276728116,3.52890424539472));
#57799=CARTESIAN_POINT('Ctrl Pts',(2.57485175518313,-1.72997103452906,3.58157445801255));
#57800=CARTESIAN_POINT('Ctrl Pts',(2.83694784679655,-0.796816585890936,
3.63424467063038));
#57801=CARTESIAN_POINT('Ctrl Pts',(3.09904393840998,0.136337862747188,3.68691488324821));
#57802=CARTESIAN_POINT('Ctrl Pts',(2.85570272583058,1.21145502727133,3.73958509586604));
#57803=CARTESIAN_POINT('Ctrl Pts',(2.21731878219618,1.9407954999751,3.79225530848387));
#57804=CARTESIAN_POINT('Ctrl Pts',(1.57893483856177,2.67013597267886,3.84492552110171));
#57805=CARTESIAN_POINT('Ctrl Pts',(0.545508163872345,3.05369975356224,3.89759573371954));
#57806=CARTESIAN_POINT('Ctrl Pts',(-0.414135207932496,2.91747866955439,
3.95026594633737));
#57807=CARTESIAN_POINT('Ctrl Pts',(-1.37377857973734,2.78125758554654,4.0029361589552));
#57808=CARTESIAN_POINT('Ctrl Pts',(-2.2596386486576,2.12525163664746,4.05560637157303));
#57809=CARTESIAN_POINT('Ctrl Pts',(-2.66983468761848,1.24706555457053,4.10827658419087));
#57810=CARTESIAN_POINT('Ctrl Pts',(-2.85037966131594,0.860537972559507,
4.13145901709737));
#57811=CARTESIAN_POINT('Ctrl Pts',(-2.93877615178763,0.430968325170985,
4.15464145000388));
#57812=CARTESIAN_POINT('Ctrl Pts',(-2.93755662075233,0.00092146372069949,
4.17782388291039));
#57813=CARTESIAN_POINT('Origin',(0.,0.,0.));
#57814=CARTESIAN_POINT('',(-2.94196835289677,-0.002621025841609,5.32217611708959));
#57815=CARTESIAN_POINT('',(-2.94205032665991,-0.00261853614193573,5.17782388291038));
#57816=CARTESIAN_POINT('',(-2.942,-3.60291088309151E-16,0.));
#57817=CARTESIAN_POINT('Ctrl Pts',(-2.94196835289677,-0.002621025841609,
5.32217611708959));
#57818=CARTESIAN_POINT('Ctrl Pts',(-2.93523282994335,0.742982230700457,
5.2818301893487));
#57819=CARTESIAN_POINT('Ctrl Pts',(-2.64664255795984,1.49322716005967,5.24148426160782));
#57820=CARTESIAN_POINT('Ctrl Pts',(-2.13487143198777,2.03113582368275,5.20113833386693));
#57821=CARTESIAN_POINT('Ctrl Pts',(-1.46677193531172,2.73335697135233,5.1484681212491));
#57822=CARTESIAN_POINT('Ctrl Pts',(-0.41831872112528,3.07370618157001,5.09579790863126));
#57823=CARTESIAN_POINT('Ctrl Pts',(0.534845211695748,2.89778007531554,5.04312769601343));
#57824=CARTESIAN_POINT('Ctrl Pts',(1.48800914451678,2.72185396906108,4.9904574833956));
#57825=CARTESIAN_POINT('Ctrl Pts',(2.34588379597239,2.02965254633447,4.93778727077777));
#57826=CARTESIAN_POINT('Ctrl Pts',(2.71928434946264,1.13520103599745,4.88511705815994));
#57827=CARTESIAN_POINT('Ctrl Pts',(3.09268490295289,0.240749525660442,4.83244684554211));
#57828=CARTESIAN_POINT('Ctrl Pts',(2.98161135847777,-0.855952072286972,
4.77977663292428));
#57829=CARTESIAN_POINT('Ctrl Pts',(2.43645352177545,-1.65737231833663,4.72710642030644));
#57830=CARTESIAN_POINT('Ctrl Pts',(1.89129568507313,-2.4587925643863,4.67443620768861));
#57831=CARTESIAN_POINT('Ctrl Pts',(0.912053556143593,-2.9649314585382,4.62176599507078));
#57832=CARTESIAN_POINT('Ctrl Pts',(-0.0570282802002683,-2.94617320275787,
4.56909578245295));
#57833=CARTESIAN_POINT('Ctrl Pts',(-1.02611011654413,-2.92741494697754,
4.51642556983512));
#57834=CARTESIAN_POINT('Ctrl Pts',(-1.98503166030232,-2.38375954126497,
4.46375535721729));
#57835=CARTESIAN_POINT('Ctrl Pts',(-2.49876699655314,-1.5618425856244,4.41108514459945));
#57836=CARTESIAN_POINT('Ctrl Pts',(-2.78783430090679,-1.09936842431115,
4.38144880209617));
#57837=CARTESIAN_POINT('Ctrl Pts',(-2.93595300469825,-0.548795001629907,
4.35181245959288));
#57838=CARTESIAN_POINT('Ctrl Pts',(-2.93758307183925,0.000962932756501389,
4.32217611708959));
#57839=CARTESIAN_POINT('Ctrl Pts',(-2.93755662075233,0.00092146372069949,
4.17782388291039));
#57840=CARTESIAN_POINT('Ctrl Pts',(-2.93600539173918,-0.54609304364936,
4.20731166262171));
#57841=CARTESIAN_POINT('Ctrl Pts',(-2.78945957767235,-1.09387966133746,
4.23679944233303));
#57842=CARTESIAN_POINT('Ctrl Pts',(-2.50313103055653,-1.55483915575367,
4.26628722204436));
#57843=CARTESIAN_POINT('Ctrl Pts',(-1.99169932553219,-2.37819156874617,
4.31895743466219));
#57844=CARTESIAN_POINT('Ctrl Pts',(-1.034303906482,-2.92453017947639,4.37162764728002));
#57845=CARTESIAN_POINT('Ctrl Pts',(-0.065278344036315,-2.94600212060899,
4.42429785989785));
#57846=CARTESIAN_POINT('Ctrl Pts',(0.903747218409357,-2.96747406174159,
4.47696807251569));
#57847=CARTESIAN_POINT('Ctrl Pts',(1.88440292425052,-2.46407933327658,4.52963828513352));
#57848=CARTESIAN_POINT('Ctrl Pts',(2.43180290302967,-1.6641888106397,4.58230849775135));
#57849=CARTESIAN_POINT('Ctrl Pts',(2.97920288180883,-0.864298288002814,
4.63497871036918));
#57850=CARTESIAN_POINT('Ctrl Pts',(3.09334713352597,0.232088028805956,4.68764892298701));
#57851=CARTESIAN_POINT('Ctrl Pts',(2.72245279039328,1.12758173127816,4.74031913560485));
#57852=CARTESIAN_POINT('Ctrl Pts',(2.35155844726061,2.02307543375035,4.79298934822268));
#57853=CARTESIAN_POINT('Ctrl Pts',(1.49562550927813,2.71767652188598,4.8456595608405));
#57854=CARTESIAN_POINT('Ctrl Pts',(0.542957912128918,2.89627113066901,4.89832977345833));
#57855=CARTESIAN_POINT('Ctrl Pts',(-0.409709685020296,3.07486573945205,
4.95099998607617));
#57856=CARTESIAN_POINT('Ctrl Pts',(-1.45911194133625,2.73745386888248,5.003670198694));
#57857=CARTESIAN_POINT('Ctrl Pts',(-2.12917531393477,2.0371063396864,5.05634041131183));
#57858=CARTESIAN_POINT('Ctrl Pts',(-2.64434078507083,1.49865747112924,5.09683490184468));
#57859=CARTESIAN_POINT('Ctrl Pts',(-2.93527864115445,0.745676951205884,
5.13732939237753));
#57860=CARTESIAN_POINT('Ctrl Pts',(-2.94205032665991,-0.00261853614193573,
5.17782388291038));
#57861=CARTESIAN_POINT('Origin',(0.,0.,0.));
#57862=CARTESIAN_POINT('',(-2.94566657928398,0.00155368773417593,6.3221761170896));
#57863=CARTESIAN_POINT('',(-2.94560897709112,0.00159264369063789,6.17782388291039));
#57864=CARTESIAN_POINT('',(-2.942,-3.60291088309151E-16,0.));
#57865=CARTESIAN_POINT('Ctrl Pts',(-2.94566657928398,0.00155368773417593,
6.3221761170896));
#57866=CARTESIAN_POINT('Ctrl Pts',(-2.94625783004801,0.0934289955880153,
6.3171883443402));
#57867=CARTESIAN_POINT('Ctrl Pts',(-2.94232816000304,0.185253079238273,
6.31220057159079));
#57868=CARTESIAN_POINT('Ctrl Pts',(-2.93371125763113,0.276635178916858,
6.30721279884139));
#57869=CARTESIAN_POINT('Ctrl Pts',(-2.8427179219604,1.24161791998335,6.25454258622356));
#57870=CARTESIAN_POINT('Ctrl Pts',(-2.22904768583453,2.15731468667283,6.20187237360573));
#57871=CARTESIAN_POINT('Ctrl Pts',(-1.37109919163641,2.60830898707571,6.1492021609879));
#57872=CARTESIAN_POINT('Ctrl Pts',(-0.513150697438283,3.05930328747859,
6.09653194837006));
#57873=CARTESIAN_POINT('Ctrl Pts',(0.589076054832107,3.04559512159484,6.04386173575223));
#57874=CARTESIAN_POINT('Ctrl Pts',(1.43554307511773,2.57340335836564,5.9911915231344));
#57875=CARTESIAN_POINT('Ctrl Pts',(2.28201009540335,2.10121159513645,5.93852131051657));
#57876=CARTESIAN_POINT('Ctrl Pts',(2.87271738370421,1.17053623456181,5.88585109789874));
#57877=CARTESIAN_POINT('Ctrl Pts',(2.93968370608133,0.203588981936339,5.83318088528091));
#57878=CARTESIAN_POINT('Ctrl Pts',(3.00665002845845,-0.763358270689132,
5.78051067266308));
#57879=CARTESIAN_POINT('Ctrl Pts',(2.54987538491182,-1.76657741536544,5.72784046004524));
#57880=CARTESIAN_POINT('Ctrl Pts',(1.77658090684437,-2.35094641512771,5.67517024742741));
#57881=CARTESIAN_POINT('Ctrl Pts',(1.00328642877692,-2.93531541488997,5.62250003480958));
#57882=CARTESIAN_POINT('Ctrl Pts',(-0.0865278838113344,-3.1008342697382,
5.56982982219175));
#57883=CARTESIAN_POINT('Ctrl Pts',(-0.998455088538058,-2.77241342543621,
5.51715960957392));
#57884=CARTESIAN_POINT('Ctrl Pts',(-1.91038229326477,-2.44399258113422,
5.46448939695609));
#57885=CARTESIAN_POINT('Ctrl Pts',(-2.64442239012996,-1.621632037682,5.41181918433825));
#57886=CARTESIAN_POINT('Ctrl Pts',(-2.86756954897972,-0.67840522339516,
5.35914897172042));
#57887=CARTESIAN_POINT('Ctrl Pts',(-2.91978367568354,-0.457699906574275,
5.34682468684348));
#57888=CARTESIAN_POINT('Ctrl Pts',(-2.94402582209679,-0.230377021386298,
5.33450040196653));
#57889=CARTESIAN_POINT('Ctrl Pts',(-2.94196835289677,-0.002621025841609,
5.32217611708959));
#57890=CARTESIAN_POINT('Ctrl Pts',(-2.94205032665991,-0.00261853614193573,
5.17782388291038));
#57891=CARTESIAN_POINT('Ctrl Pts',(-2.94408641007957,-0.227613042098249,
5.18999960499536));
#57892=CARTESIAN_POINT('Ctrl Pts',(-2.92043214775034,-0.452183992687412,
5.20217532708034));
#57893=CARTESIAN_POINT('Ctrl Pts',(-2.86945823375718,-0.670372434833386,
5.21435104916532));
#57894=CARTESIAN_POINT('Ctrl Pts',(-2.64895329209997,-1.61422049233453,
5.26702126178316));
#57895=CARTESIAN_POINT('Ctrl Pts',(-1.91721891990443,-2.43863341951423,
5.31969147440099));
#57896=CARTESIAN_POINT('Ctrl Pts',(-1.00621492850077,-2.76960670029717,
5.37236168701883));
#57897=CARTESIAN_POINT('Ctrl Pts',(-0.0952109370971131,-3.1005799810801,
5.42503189963666));
#57898=CARTESIAN_POINT('Ctrl Pts',(0.995062673514658,-2.93811361546629,
5.47770211225449));
#57899=CARTESIAN_POINT('Ctrl Pts',(1.76999059505944,-2.35591236043814,5.53037232487231));
#57900=CARTESIAN_POINT('Ctrl Pts',(2.54491851660422,-1.77371110540999,5.58304253749014));
#57901=CARTESIAN_POINT('Ctrl Pts',(3.00450074908201,-0.77177496096749,5.63571275010798));
#57902=CARTESIAN_POINT('Ctrl Pts',(2.94024246570664,0.195356083908528,5.68838296272581));
#57903=CARTESIAN_POINT('Ctrl Pts',(2.87598418233127,1.16248712878457,5.74105317534364));
#57904=CARTESIAN_POINT('Ctrl Pts',(2.28788538310274,2.09481307409411,5.79372338796148));
#57905=CARTESIAN_POINT('Ctrl Pts',(1.44274393054363,2.56937340757336,5.84639360057931));
#57906=CARTESIAN_POINT('Ctrl Pts',(0.597602477984537,3.0439337410526,5.89906381319714));
#57907=CARTESIAN_POINT('Ctrl Pts',(-0.504581627905147,3.06072846270153,
5.95173402581497));
#57908=CARTESIAN_POINT('Ctrl Pts',(-1.36378974409505,2.61213845164572,6.0044042384328));
#57909=CARTESIAN_POINT('Ctrl Pts',(-2.22299786028497,2.1635484405899,6.05707445105063));
#57910=CARTESIAN_POINT('Ctrl Pts',(-2.83922998677511,1.24957369682933,6.10974466366847));
#57911=CARTESIAN_POINT('Ctrl Pts',(-2.93292524981251,0.284849496536871,
6.1624148762863));
#57912=CARTESIAN_POINT('Ctrl Pts',(-2.94206229873784,0.190770757316082,
6.16755121182766));
#57913=CARTESIAN_POINT('Ctrl Pts',(-2.94623006655259,0.0962093950817709,
6.17268754736903));
#57914=CARTESIAN_POINT('Ctrl Pts',(-2.94560897709112,0.00159264369063789,
6.17782388291039));
#57915=CARTESIAN_POINT('Origin',(0.,0.,0.));
#57916=CARTESIAN_POINT('',(-2.93773181355748,0.00116367510156062,7.3221761170896));
#57917=CARTESIAN_POINT('',(-2.93769958596831,0.00112364184895479,7.17782388291039));
#57918=CARTESIAN_POINT('',(-2.942,-3.60291088309151E-16,0.));
#57919=CARTESIAN_POINT('Ctrl Pts',(-2.93773181355748,0.00116367510156062,
7.3221761170896));
#57920=CARTESIAN_POINT('Ctrl Pts',(-2.93921846510379,0.414775956166668,
7.29987628671385));
#57921=CARTESIAN_POINT('Ctrl Pts',(-2.85767291508901,0.827828420512208,
7.2775764563381));
#57922=CARTESIAN_POINT('Ctrl Pts',(-2.69021112169706,1.20247781104825,7.25527662596236));
#57923=CARTESIAN_POINT('Ctrl Pts',(-2.29468128516027,2.08736629334525,7.20260641334453));
#57924=CARTESIAN_POINT('Ctrl Pts',(-1.4198571053233,2.75801849948865,7.14993620072669));
#57925=CARTESIAN_POINT('Ctrl Pts',(-0.462612749536846,2.91018525343868,
7.09726598810886));
#57926=CARTESIAN_POINT('Ctrl Pts',(0.494631606249605,3.0623520073887,7.04459577549103));
#57927=CARTESIAN_POINT('Ctrl Pts',(1.53429613798554,2.69603330914537,6.9919255628732));
#57928=CARTESIAN_POINT('Ctrl Pts',(2.18472493484141,1.97741389811242,6.93925535025537));
#57929=CARTESIAN_POINT('Ctrl Pts',(2.83515373169728,1.25879448707948,6.88658513763754));
#57930=CARTESIAN_POINT('Ctrl Pts',(3.09634679367307,0.187874363256921,6.83391492501971));
#57931=CARTESIAN_POINT('Ctrl Pts',(2.84981084934511,-0.749511099531479,
6.78124471240188));
#57932=CARTESIAN_POINT('Ctrl Pts',(2.60327490501715,-1.68689656231988,6.72857449978404));
#57933=CARTESIAN_POINT('Ctrl Pts',(1.84900995438544,-2.49074736407413,6.67590428716621));
#57934=CARTESIAN_POINT('Ctrl Pts',(0.929197067821797,-2.79638723615263,
6.62323407454838));
#57935=CARTESIAN_POINT('Ctrl Pts',(0.00938418125816035,-3.10202710823113,
6.57056386193055));
#57936=CARTESIAN_POINT('Ctrl Pts',(-1.07597664123741,-2.90945605063389,
6.51789364931272));
#57937=CARTESIAN_POINT('Ctrl Pts',(-1.83449883487741,-2.30603616411352,
6.46522343669488));
#57938=CARTESIAN_POINT('Ctrl Pts',(-2.52119036486117,-1.75975903659949,
6.41754099682645));
#57939=CARTESIAN_POINT('Ctrl Pts',(-2.94001430111904,-0.87676195779301,
6.36985855695803));
#57940=CARTESIAN_POINT('Ctrl Pts',(-2.94566657928398,0.00155368773417593,
6.3221761170896));
#57941=CARTESIAN_POINT('Ctrl Pts',(-2.94560897709112,0.00159264369063789,
6.17782388291039));
#57942=CARTESIAN_POINT('Ctrl Pts',(-2.93986114580615,-0.87403181537772,
6.22535775998686));
#57943=CARTESIAN_POINT('Ctrl Pts',(-2.52397381508728,-1.75440005354465,
6.27289163706332));
#57944=CARTESIAN_POINT('Ctrl Pts',(-1.84094942996504,-2.30089003495964,
6.32042551413979));
#57945=CARTESIAN_POINT('Ctrl Pts',(-1.08411994749553,-2.90643170933934,
6.37309572675762));
#57946=CARTESIAN_POINT('Ctrl Pts',(0.000697417028111963,-3.10204140127437,
6.42576593937545));
#57947=CARTESIAN_POINT('Ctrl Pts',(0.921362644850236,-2.79897849819174,
6.47843615199329));
#57948=CARTESIAN_POINT('Ctrl Pts',(1.84202787267235,-2.49591559510911,6.53110636461112));
#57949=CARTESIAN_POINT('Ctrl Pts',(2.59854096379293,-1.69418009700883,6.58377657722895));
#57950=CARTESIAN_POINT('Ctrl Pts',(2.84770095275134,-0.757488640419289,
6.63644678984678));
#57951=CARTESIAN_POINT('Ctrl Pts',(3.09686094170975,0.179202816170267,6.68911700246461));
#57952=CARTESIAN_POINT('Ctrl Pts',(2.83866782850598,1.25085023124908,6.74178721508244));
#57953=CARTESIAN_POINT('Ctrl Pts',(2.19025392290029,1.9712882868533,6.79445742770027));
#57954=CARTESIAN_POINT('Ctrl Pts',(1.5418400172946,2.69172634245752,6.8471276403181));
#57955=CARTESIAN_POINT('Ctrl Pts',(0.50320531928699,3.06095503858714,6.89979785293594));
#57956=CARTESIAN_POINT('Ctrl Pts',(-0.454461456345466,2.91146948144086,
6.95246806555377));
#57957=CARTESIAN_POINT('Ctrl Pts',(-1.41212823197794,2.76198392429457,7.0051382781716));
#57958=CARTESIAN_POINT('Ctrl Pts',(-2.28882708523526,2.09378411387235,7.05780849078943));
#57959=CARTESIAN_POINT('Ctrl Pts',(-2.68683338135866,1.21000666836259,7.11047870340727));
#57960=CARTESIAN_POINT('Ctrl Pts',(-2.85646629860981,0.833334872607608,
7.13292709657497));
#57961=CARTESIAN_POINT('Ctrl Pts',(-2.93914371675611,0.417502950847913,
7.15537548974268));
#57962=CARTESIAN_POINT('Ctrl Pts',(-2.93769958596831,0.00112364184895479,
7.17782388291039));
#57963=CARTESIAN_POINT('Origin',(0.,0.,0.));
#57964=CARTESIAN_POINT('',(-2.94156648412342,-0.00262140296731356,8.3221761170896));
#57965=CARTESIAN_POINT('',(-2.94164760189786,-0.00262292145090667,8.17782388291039));
#57966=CARTESIAN_POINT('',(-2.942,-3.60291088309151E-16,0.));
#57967=CARTESIAN_POINT('Ctrl Pts',(-2.94156648412342,-0.00262140296731356,
8.3221761170896));
#57968=CARTESIAN_POINT('Ctrl Pts',(-2.93503453701149,0.72967238878934,8.28256422908751));
#57969=CARTESIAN_POINT('Ctrl Pts',(-2.65787464556332,1.46638000617809,8.24295234108542));
#57970=CARTESIAN_POINT('Ctrl Pts',(-2.16276963608865,2.00140357413964,8.20334045308333));
#57971=CARTESIAN_POINT('Ctrl Pts',(-1.50444993883493,2.7128012504786,8.15067024046549));
#57972=CARTESIAN_POINT('Ctrl Pts',(-0.46080611438605,3.06762415690109,8.09800002784767));
#57973=CARTESIAN_POINT('Ctrl Pts',(0.494700673992003,2.90490275371101,8.04532981522984));
#57974=CARTESIAN_POINT('Ctrl Pts',(1.45020746237007,2.74218135052094,7.99265960261201));
#57975=CARTESIAN_POINT('Ctrl Pts',(2.31757721467732,2.06191563771829,7.93998938999417));
#57976=CARTESIAN_POINT('Ctrl Pts',(2.70331755134067,1.17271607048742,7.88731917737634));
#57977=CARTESIAN_POINT('Ctrl Pts',(3.08905788800402,0.283516503256563,7.8346489647585));
#57978=CARTESIAN_POINT('Ctrl Pts',(2.99316880902349,-0.814616918402493,
7.78197875214068));
#57979=CARTESIAN_POINT('Ctrl Pts',(2.45915151070291,-1.62350319148857,7.72930853952285));
#57980=CARTESIAN_POINT('Ctrl Pts',(1.92513421238232,-2.43238946457466,7.67663832690502));
#57981=CARTESIAN_POINT('Ctrl Pts',(0.952988694721666,-2.95202858908774,
7.62396811428717));
#57982=CARTESIAN_POINT('Ctrl Pts',(-0.0162599177366882,-2.9466802304358,
7.57129790166934));
#57983=CARTESIAN_POINT('Ctrl Pts',(-0.985508530195028,-2.94133187178385,
7.51862768905151));
#57984=CARTESIAN_POINT('Ctrl Pts',(-1.95186023745108,-2.41099602996689,
7.46595747643369));
#57985=CARTESIAN_POINT('Ctrl Pts',(-2.47691834446078,-1.59626572983311,
7.41328726381586));
#57986=CARTESIAN_POINT('Ctrl Pts',(-2.77967420240452,-1.12648082847323,
7.38291688157377));
#57987=CARTESIAN_POINT('Ctrl Pts',(-2.93570712659971,-0.562139402290024,
7.35254649933169));
#57988=CARTESIAN_POINT('Ctrl Pts',(-2.93773181355748,0.00116367510156062,
7.3221761170896));
#57989=CARTESIAN_POINT('Ctrl Pts',(-2.93769958596831,0.00112364184895479,
7.17782388291039));
#57990=CARTESIAN_POINT('Ctrl Pts',(-2.93575538178383,-0.559439432992209,
7.20804570236051));
#57991=CARTESIAN_POINT('Ctrl Pts',(-2.78134344073081,-1.12099463047756,
7.23826752181064));
#57992=CARTESIAN_POINT('Ctrl Pts',(-2.48137885938122,-1.58932335063733,
7.26848934126076));
#57993=CARTESIAN_POINT('Ctrl Pts',(-1.95860430229089,-2.40552084353022,
7.32115955387859));
#57994=CARTESIAN_POINT('Ctrl Pts',(-0.993741449120738,-2.93856074871869,
7.37382976649642));
#57995=CARTESIAN_POINT('Ctrl Pts',(-0.0245115589366341,-2.94662331154554,
7.42649997911425));
#57996=CARTESIAN_POINT('Ctrl Pts',(0.944718331247456,-2.95468587437239,
7.47917019173208));
#57997=CARTESIAN_POINT('Ctrl Pts',(1.9183152584455,-2.43777109483764,7.53184040434991));
#57998=CARTESIAN_POINT('Ctrl Pts',(2.45459564929204,-1.63038337673742,7.58451061696775));
#57999=CARTESIAN_POINT('Ctrl Pts',(2.99087604013859,-0.822995658637189,
7.63718082958558));
#58000=CARTESIAN_POINT('Ctrl Pts',(3.08983989463362,0.274864998028533,7.68985104220341));
#58001=CARTESIAN_POINT('Ctrl Pts',(2.7065911087876,1.16514133327123,7.74252125482124));
#58002=CARTESIAN_POINT('Ctrl Pts',(2.32334232294156,2.05541766851393,7.79519146743908));
#58003=CARTESIAN_POINT('Ctrl Pts',(1.45788089675451,2.7381096823336,7.8478616800569));
#58004=CARTESIAN_POINT('Ctrl Pts',(0.502833475452543,2.90350619986069,7.90053189267474));
#58005=CARTESIAN_POINT('Ctrl Pts',(-0.452213945849419,3.06890271738777,
7.95320210529257));
#58006=CARTESIAN_POINT('Ctrl Pts',(-1.49684736226627,2.71700373862224,8.0058723179104));
#58007=CARTESIAN_POINT('Ctrl Pts',(-2.15715667062231,2.0074523294601,8.05854253052823));
#58008=CARTESIAN_POINT('Ctrl Pts',(-2.6556204978759,1.47181591396764,8.09830298132228));
#58009=CARTESIAN_POINT('Ctrl Pts',(-2.93507122923162,0.732365674690379,
8.13806343211634));
#58010=CARTESIAN_POINT('Ctrl Pts',(-2.94164760189786,-0.00262292145090667,
8.17782388291039));
#58011=CARTESIAN_POINT('Origin',(0.,0.,0.));
#58012=CARTESIAN_POINT('',(-2.945934045911,0.00135292032082991,9.3221761170896));
#58013=CARTESIAN_POINT('',(-2.94588259210377,0.00139462648580093,9.1778238829104));
#58014=CARTESIAN_POINT('',(-2.942,-3.60291088309151E-16,0.));
#58015=CARTESIAN_POINT('Ctrl Pts',(-2.945934045911,0.00135292032082991,
9.3221761170896));
#58016=CARTESIAN_POINT('Ctrl Pts',(-2.94638425749025,0.0796883308965953,
9.317922384079));
#58017=CARTESIAN_POINT('Ctrl Pts',(-2.94352772129697,0.15799040718347,9.31366865106839));
#58018=CARTESIAN_POINT('Ctrl Pts',(-2.93725793323127,0.236018217593314,
9.30941491805779));
#58019=CARTESIAN_POINT('Ctrl Pts',(-2.85962469445823,1.20216756315553,9.25674470543996));
#58020=CARTESIAN_POINT('Ctrl Pts',(-2.25868267116007,2.12626734773872,9.20407449282213));
#58021=CARTESIAN_POINT('Ctrl Pts',(-1.40705620388363,2.58908895260061,9.1514042802043));
#58022=CARTESIAN_POINT('Ctrl Pts',(-0.555429736607181,3.05191055746251,
9.09873406758647));
#58023=CARTESIAN_POINT('Ctrl Pts',(0.54688117464756,3.05345398260311,9.04606385496863));
#58024=CARTESIAN_POINT('Ctrl Pts',(1.39980036012117,2.59301903525034,8.9933936423508));
#58025=CARTESIAN_POINT('Ctrl Pts',(2.25271954559477,2.13258408789758,8.94072342973297));
#58026=CARTESIAN_POINT('Ctrl Pts',(2.85624700528725,1.21017076805146,8.88805321711514));
#58027=CARTESIAN_POINT('Ctrl Pts',(2.93658548535115,0.24424261010507,8.83538300449731));
#58028=CARTESIAN_POINT('Ctrl Pts',(3.01692396541504,-0.721685547841337,
8.78271279187948));
#58029=CARTESIAN_POINT('Ctrl Pts',(2.57407346585034,-1.73112854388803,8.73004257926165));
#58030=CARTESIAN_POINT('Ctrl Pts',(1.80893826814173,-2.32614081848421,8.67737236664381));
#58031=CARTESIAN_POINT('Ctrl Pts',(1.04380307043313,-2.92115309308037,8.62470215402598));
#58032=CARTESIAN_POINT('Ctrl Pts',(-0.0436168254193812,-3.10173464622604,
8.57203194140814));
#58033=CARTESIAN_POINT('Ctrl Pts',(-0.960000732043568,-2.78596255535529,
8.51936172879031));
#58034=CARTESIAN_POINT('Ctrl Pts',(-1.87638463866775,-2.47019046448454,
8.46669151617249));
#58035=CARTESIAN_POINT('Ctrl Pts',(-2.62173255606362,-1.65806472959736,
8.41402130355466));
#58036=CARTESIAN_POINT('Ctrl Pts',(-2.85790872973228,-0.718015639026068,
8.36135109093683));
#58037=CARTESIAN_POINT('Ctrl Pts',(-2.91646298628421,-0.484952858959428,
8.34829276632109));
#58038=CARTESIAN_POINT('Ctrl Pts',(-2.94371978430835,-0.244026964003591,
8.33523444170534));
#58039=CARTESIAN_POINT('Ctrl Pts',(-2.94156648412342,-0.00262140296731356,
8.3221761170896));
#58040=CARTESIAN_POINT('Ctrl Pts',(-2.94164760189786,-0.00262292145090667,
8.17782388291039));
#58041=CARTESIAN_POINT('Ctrl Pts',(-2.94378287458944,-0.241265279117494,
8.19073364473417));
#58042=CARTESIAN_POINT('Ctrl Pts',(-2.91715101380018,-0.479437278615387,
8.20364340655795));
#58043=CARTESIAN_POINT('Ctrl Pts',(-2.85990837443616,-0.710009750985903,
8.21655316838173));
#58044=CARTESIAN_POINT('Ctrl Pts',(-2.62636556959873,-1.65071658271101,
8.26922338099956));
#58045=CARTESIAN_POINT('Ctrl Pts',(-1.88329475962863,-2.46492640660245,
8.32189359361739));
#58046=CARTESIAN_POINT('Ctrl Pts',(-0.96779866274798,-2.78326346310376,
8.37456380623522));
#58047=CARTESIAN_POINT('Ctrl Pts',(-0.0523025658673351,-3.10160051960507,
8.42723401885305));
#58048=CARTESIAN_POINT('Ctrl Pts',(1.03561881792387,-2.92406480871623,8.47990423147088));
#58049=CARTESIAN_POINT('Ctrl Pts',(1.80241729541542,-2.33119747122643,8.53257444408871));
#58050=CARTESIAN_POINT('Ctrl Pts',(2.56921577290696,-1.73833013373663,8.58524465670654));
#58051=CARTESIAN_POINT('Ctrl Pts',(3.01489134409887,-0.730131169645851,
8.63791486932438));
#58052=CARTESIAN_POINT('Ctrl Pts',(2.9372581008944,0.236018231065629,8.69058508194221));
#58053=CARTESIAN_POINT('Ctrl Pts',(2.85962485768992,1.20216763177713,8.74325529456004));
#58054=CARTESIAN_POINT('Ctrl Pts',(2.25868280008906,2.12626746910933,8.79592550717788));
#58055=CARTESIAN_POINT('Ctrl Pts',(1.40705628420046,2.58908910038977,8.84859571979571));
#58056=CARTESIAN_POINT('Ctrl Pts',(0.555429768311884,3.0519107316702,8.90126593241354));
#58057=CARTESIAN_POINT('Ctrl Pts',(-0.546881205864421,3.05345415689887,
8.95393614503137));
#58058=CARTESIAN_POINT('Ctrl Pts',(-1.39980044002393,2.59301918326378,9.0066063576492));
#58059=CARTESIAN_POINT('Ctrl Pts',(-2.25271967418346,2.13258420962867,9.05927657026703));
#58060=CARTESIAN_POINT('Ctrl Pts',(-2.85624716832619,1.21017083712978,9.11194678288487));
#58061=CARTESIAN_POINT('Ctrl Pts',(-2.9365856529759,0.244242624046729,9.1646169955027));
#58062=CARTESIAN_POINT('Ctrl Pts',(-2.94330052569389,0.163508153713587,
9.16901929130527));
#58063=CARTESIAN_POINT('Ctrl Pts',(-2.94636040237331,0.0824696889022224,
9.17342158710783));
#58064=CARTESIAN_POINT('Ctrl Pts',(-2.94588259210377,0.00139462648580093,
9.1778238829104));
#58065=CARTESIAN_POINT('Origin',(0.,0.,0.));
#58066=CARTESIAN_POINT('',(-2.937908603757,0.00135649600012097,10.3221761170896));
#58067=CARTESIAN_POINT('',(-2.93787076970937,0.00131817605956517,10.1778238829104));
#58068=CARTESIAN_POINT('',(-2.942,-3.60291088309151E-16,0.));
#58069=CARTESIAN_POINT('Ctrl Pts',(-2.937908603757,0.00135649600012097,
10.3221761170896));
#58070=CARTESIAN_POINT('Ctrl Pts',(-2.93959056192569,0.401293686681912,
10.3006103264527));
#58071=CARTESIAN_POINT('Ctrl Pts',(-2.86351195754617,0.800618114023186,
10.2790445358157));
#58072=CARTESIAN_POINT('Ctrl Pts',(-2.70659095429132,1.16514126676313,10.2574787451788));
#58073=CARTESIAN_POINT('Ctrl Pts',(-2.32334219032173,2.05541755118752,10.2048085325609));
#58074=CARTESIAN_POINT('Ctrl Pts',(-1.45788081353651,2.73810952603814,10.1521383199431));
#58075=CARTESIAN_POINT('Ctrl Pts',(-0.502833446750087,2.90350603412416,
10.0994681073253));
#58076=CARTESIAN_POINT('Ctrl Pts',(0.452213920036317,3.06890254221017,10.0467978947074));
#58077=CARTESIAN_POINT('Ctrl Pts',(1.49684727682391,2.71700358353159,9.99412768208959));
#58078=CARTESIAN_POINT('Ctrl Pts',(2.15715654748851,2.00745221487173,9.94145746947176));
#58079=CARTESIAN_POINT('Ctrl Pts',(2.81746581815312,1.29790084621186,9.88878725685393));
#58080=CARTESIAN_POINT('Ctrl Pts',(3.09345100269472,0.230697067570708,9.83611704423611));
#58081=CARTESIAN_POINT('Ctrl Pts',(2.85990821118827,-0.710009710457437,
9.78344683161828));
#58082=CARTESIAN_POINT('Ctrl Pts',(2.62636541968183,-1.65071648848557,9.73077661900045));
#58083=CARTESIAN_POINT('Ctrl Pts',(1.88329465212736,-2.46492626590069,9.67810640638261));
#58084=CARTESIAN_POINT('Ctrl Pts',(0.967798607504626,-2.78326330423086,
9.62543619376478));
#58085=CARTESIAN_POINT('Ctrl Pts',(0.0523025628818791,-3.10160034256102,
9.57276598114694));
#58086=CARTESIAN_POINT('Ctrl Pts',(-1.03561875880913,-2.92406464180621,
9.52009576852912));
#58087=CARTESIAN_POINT('Ctrl Pts',(-1.80241719253068,-2.33119733815818,
9.46742555591129));
#58088=CARTESIAN_POINT('Ctrl Pts',(-2.50728772340386,-1.78621097318669,
9.41900907630406));
#58089=CARTESIAN_POINT('Ctrl Pts',(-2.94080968580394,-0.890269755388179,
9.37059259669683));
#58090=CARTESIAN_POINT('Ctrl Pts',(-2.945934045911,0.00135292032082991,
9.3221761170896));
#58091=CARTESIAN_POINT('Ctrl Pts',(-2.94588259210377,0.00139462648580093,
9.1778238829104));
#58092=CARTESIAN_POINT('Ctrl Pts',(-2.9406437559651,-0.887533456499498,
9.22609179972566));
#58093=CARTESIAN_POINT('Ctrl Pts',(-2.51012187433051,-1.78086112066889,
9.27435971654092));
#58094=CARTESIAN_POINT('Ctrl Pts',(-1.80893837139867,-2.32614095126385,
9.32262763335619));
#58095=CARTESIAN_POINT('Ctrl Pts',(-1.04380313001497,-2.92115325982423,
9.37529784597402));
#58096=CARTESIAN_POINT('Ctrl Pts',(0.0436168279091599,-3.10173482327776,
9.42796805859185));
#58097=CARTESIAN_POINT('Ctrl Pts',(0.96000078684194,-2.78596271438223,9.48063827120969));
#58098=CARTESIAN_POINT('Ctrl Pts',(1.8763847457747,-2.4701906054867,9.53330848382752));
#58099=CARTESIAN_POINT('Ctrl Pts',(2.62173270571613,-1.65806482424214,9.58597869644535));
#58100=CARTESIAN_POINT('Ctrl Pts',(2.85790889286606,-0.718015680011411,
9.63864890906318));
#58101=CARTESIAN_POINT('Ctrl Pts',(3.09408508001598,0.222033464219328,9.69131912168101));
#58102=CARTESIAN_POINT('Ctrl Pts',(2.82108949437439,1.29000597143625,9.74398933429884));
#58103=CARTESIAN_POINT('Ctrl Pts',(2.16276975954276,2.00140368838285,9.79665954691667));
#58104=CARTESIAN_POINT('Ctrl Pts',(1.50445002471113,2.71280140532944,9.8493297595345));
#58105=CARTESIAN_POINT('Ctrl Pts',(0.460806140689482,3.06762433200573,9.90199997215234));
#58106=CARTESIAN_POINT('Ctrl Pts',(-0.494700702230345,2.90490291952725,
9.95467018477017));
#58107=CARTESIAN_POINT('Ctrl Pts',(-1.45020754515017,2.74218150704877,10.007340397388));
#58108=CARTESIAN_POINT('Ctrl Pts',(-2.31757734696816,2.06191575541552,10.0600106100058));
#58109=CARTESIAN_POINT('Ctrl Pts',(-2.70331770565014,1.1727161374278,10.1126808226237));
#58110=CARTESIAN_POINT('Ctrl Pts',(-2.86234691901197,0.806125728652842,
10.1343951760526));
#58111=CARTESIAN_POINT('Ctrl Pts',(-2.93951519940773,0.404023534891029,
10.1561095294815));
#58112=CARTESIAN_POINT('Ctrl Pts',(-2.93787076970937,0.00131817605956517,
10.1778238829104));
#58113=CARTESIAN_POINT('Origin',(0.,0.,0.));
#58114=CARTESIAN_POINT('',(-2.94117042680329,-0.00260214605593889,11.3221761170896));
#58115=CARTESIAN_POINT('',(-2.94125015913141,-0.00260761204136433,11.1778238829104));
#58116=CARTESIAN_POINT('',(-2.942,-3.60291088309151E-16,0.));
#58117=CARTESIAN_POINT('Ctrl Pts',(-2.94117042680329,-0.00260214605593889,
11.3221761170896));
#58118=CARTESIAN_POINT('Ctrl Pts',(-2.93488023009645,0.716368602336758,
11.2832982688263));
#58119=CARTESIAN_POINT('Ctrl Pts',(-2.66887225681339,1.43950600718068,11.244420420563));
#58120=CARTESIAN_POINT('Ctrl Pts',(-2.19025379787731,1.97128817432916,11.2055425722997));
#58121=CARTESIAN_POINT('Ctrl Pts',(-1.54183992928408,2.69172618880969,11.1528723596819));
#58122=CARTESIAN_POINT('Ctrl Pts',(-0.503205290563314,3.06095486386319,
11.1002021470641));
#58123=CARTESIAN_POINT('Ctrl Pts',(0.454461430404082,2.91146931524978,11.0475319344462));
#58124=CARTESIAN_POINT('Ctrl Pts',(1.41212815137148,2.76198376663637,10.9948617218284));
#58125=CARTESIAN_POINT('Ctrl Pts',(2.28882695458549,2.09378399435604,10.9421915092106));
#58126=CARTESIAN_POINT('Ctrl Pts',(2.68683322799011,1.21000659929365,10.8895212965927));
#58127=CARTESIAN_POINT('Ctrl Pts',(3.08483950139474,0.326229204231253,10.8368510839749));
#58128=CARTESIAN_POINT('Ctrl Pts',(3.00415324498994,-0.77312581361321,10.7841808713571));
#58129=CARTESIAN_POINT('Ctrl Pts',(2.48137871774039,-1.58932325991632,10.7315106587392));
#58130=CARTESIAN_POINT('Ctrl Pts',(1.95860419049084,-2.40552070621941,10.6788404461214));
#58131=CARTESIAN_POINT('Ctrl Pts',(0.993741392396532,-2.93856058098118,
10.6261702335036));
#58132=CARTESIAN_POINT('Ctrl Pts',(0.0245115575375578,-2.94662314334783,
10.5735000208857));
#58133=CARTESIAN_POINT('Ctrl Pts',(-0.944718277321443,-2.95468570571448,
10.5208298082679));
#58134=CARTESIAN_POINT('Ctrl Pts',(-1.91831514894513,-2.43777095568602,
10.4681595956501));
#58135=CARTESIAN_POINT('Ctrl Pts',(-2.45459550917999,-1.6303832836727,10.4154893830323));
#58136=CARTESIAN_POINT('Ctrl Pts',(-2.77129616018816,-1.15358006598522,
10.3843849610514));
#58137=CARTESIAN_POINT('Ctrl Pts',(-2.93548270908362,-0.575474437501757,
10.3532805390705));
#58138=CARTESIAN_POINT('Ctrl Pts',(-2.937908603757,0.00135649600012097,
10.3221761170896));
#58139=CARTESIAN_POINT('Ctrl Pts',(-2.93787076970937,0.00131817605956517,
10.1778238829104));
#58140=CARTESIAN_POINT('Ctrl Pts',(-2.93552648005067,-0.572776301283541,
10.2087797420993));
#58141=CARTESIAN_POINT('Ctrl Pts',(-2.7730096063261,-1.14809660257953,10.2397356012882));
#58142=CARTESIAN_POINT('Ctrl Pts',(-2.45915165107498,-1.62350328416062,
10.2706914604772));
#58143=CARTESIAN_POINT('Ctrl Pts',(-1.92513432227186,-2.43238960341916,
10.323361673095));
#58144=CARTESIAN_POINT('Ctrl Pts',(-0.95298874911967,-2.95202875759402,
10.3760318857128));
#58145=CARTESIAN_POINT('Ctrl Pts',(0.0162599186648668,-2.94668039863677,
10.4287020983307));
#58146=CARTESIAN_POINT('Ctrl Pts',(0.985508586449376,-2.94133203967952,
10.4813723109485));
#58147=CARTESIAN_POINT('Ctrl Pts',(1.95186034886621,-2.41099616759018,10.5340425235663));
#58148=CARTESIAN_POINT('Ctrl Pts',(2.47691848584703,-1.59626582095038,10.5867127361841));
#58149=CARTESIAN_POINT('Ctrl Pts',(3.00197662282786,-0.781535474310547,
10.639382948802));
#58150=CARTESIAN_POINT('Ctrl Pts',(3.08574113437262,0.317589346879808,10.6920531614198));
#58151=CARTESIAN_POINT('Ctrl Pts',(2.69021127525836,1.20247787968758,10.7447233740376));
#58152=CARTESIAN_POINT('Ctrl Pts',(2.2946814161441,2.08736641249534,10.7973935866555));
#58153=CARTESIAN_POINT('Ctrl Pts',(1.41985718637085,2.75801865692054,10.8500637992733));
#58154=CARTESIAN_POINT('Ctrl Pts',(0.462612775943444,2.91018541955646,10.9027340118911));
#58155=CARTESIAN_POINT('Ctrl Pts',(-0.494631634483977,3.06235218219239,
10.955404224509));
#58156=CARTESIAN_POINT('Ctrl Pts',(-1.53429622556554,2.69603346303901,11.0080744371268));
#58157=CARTESIAN_POINT('Ctrl Pts',(-2.18472505954886,1.97741401098616,11.0607446497446));
#58158=CARTESIAN_POINT('Ctrl Pts',(-2.6666654538549,1.44494723832272,11.0997710607999));
#58159=CARTESIAN_POINT('Ctrl Pts',(-2.93490816391246,0.719060797998435,
11.1387974718551));
#58160=CARTESIAN_POINT('Ctrl Pts',(-2.94125015913141,-0.00260761204136433,
11.1778238829104));
#58161=CARTESIAN_POINT('Origin',(0.,0.,0.));
#58162=CARTESIAN_POINT('',(-2.94616893643284,0.00113950433258347,12.3221761170896));
#58163=CARTESIAN_POINT('',(-2.94612437222716,0.00118363909654153,12.1778238829104));
#58164=CARTESIAN_POINT('',(-2.942,-3.60291088309151E-16,0.));
#58165=CARTESIAN_POINT('Ctrl Pts',(-2.94616893643284,0.00113950433258347,
12.3221761170896));
#58166=CARTESIAN_POINT('Ctrl Pts',(-2.94649117204446,0.0659433585993606,
12.3186564238178));
#58167=CARTESIAN_POINT('Ctrl Pts',(-2.94453636511729,0.130727428441818,
12.315136730546));
#58168=CARTESIAN_POINT('Ctrl Pts',(-2.94024229787316,0.195356072757268,
12.3116170372742));
#58169=CARTESIAN_POINT('Ctrl Pts',(-2.87598401816576,1.16248706242799,12.2589468246564));
#58170=CARTESIAN_POINT('Ctrl Pts',(-2.28788525250681,2.09481295451898,12.2062766120385));
#58171=CARTESIAN_POINT('Ctrl Pts',(-1.44274384818968,2.56937326090962,12.1536063994207));
#58172=CARTESIAN_POINT('Ctrl Pts',(-0.597602443872523,3.04393356730027,
12.1009361868029));
#58173=CARTESIAN_POINT('Ctrl Pts',(0.504581599102847,3.06072828799054,12.048265974185));
#58174=CARTESIAN_POINT('Ctrl Pts',(1.36378966624788,2.61213830254091,11.9955957615672));
#58175=CARTESIAN_POINT('Ctrl Pts',(2.22299773339287,2.16354831709129,11.9429255489494));
#58176=CARTESIAN_POINT('Ctrl Pts',(2.83922982470756,1.24957362550181,11.8902553363315));
#58177=CARTESIAN_POINT('Ctrl Pts',(2.9329250823967,0.28484948027729,11.8375851237137));
#58178=CARTESIAN_POINT('Ctrl Pts',(3.02662034008585,-0.679874664947257,
11.7849149110959));
#58179=CARTESIAN_POINT('Ctrl Pts',(2.59777876414943,-1.69534826380686,11.732244698478));
#58180=CARTESIAN_POINT('Ctrl Pts',(1.8409493248809,-2.30088990362134,11.6795744858602));
#58181=CARTESIAN_POINT('Ctrl Pts',(1.08411988561237,-2.90643154343581,11.6269042732424));
#58182=CARTESIAN_POINT('Ctrl Pts',(-0.000697416988240523,-3.10204122420515,
11.5742340606246));
#58183=CARTESIAN_POINT('Ctrl Pts',(-0.921362592257407,-2.79897833842183,
11.5215638480067));
#58184=CARTESIAN_POINT('Ctrl Pts',(-1.84202776752656,-2.49591545263851,
11.4688936353889));
#58185=CARTESIAN_POINT('Ctrl Pts',(-2.59854081546425,-1.69418000030252,
11.4162234227711));
#58186=CARTESIAN_POINT('Ctrl Pts',(-2.84770079020025,-0.75748859718075,
11.3635532101532));
#58187=CARTESIAN_POINT('Ctrl Pts',(-2.91294649518841,-0.512204052511054,
11.3497608457987));
#58188=CARTESIAN_POINT('Ctrl Pts',(-2.94340194651742,-0.2576652980836,11.3359684814441));
#58189=CARTESIAN_POINT('Ctrl Pts',(-2.94117042680329,-0.00260214605593889,
11.3221761170896));
#58190=CARTESIAN_POINT('Ctrl Pts',(-2.94125015913141,-0.00260761204136433,
11.1778238829104));
#58191=CARTESIAN_POINT('Ctrl Pts',(-2.94346734800271,-0.25490599957757,
11.191467684473));
#58192=CARTESIAN_POINT('Ctrl Pts',(-2.91367420009343,-0.506688846062122,
11.2051114860356));
#58193=CARTESIAN_POINT('Ctrl Pts',(-2.84981101201662,-0.749511142314743,
11.2187552875981));
#58194=CARTESIAN_POINT('Ctrl Pts',(-2.603275053616,-1.68689665861052,11.271425500216));
#58195=CARTESIAN_POINT('Ctrl Pts',(-1.84901005992971,-2.49074750624977,
11.3240957128338));
#58196=CARTESIAN_POINT('Ctrl Pts',(-0.929197120861756,-2.79638739577465,
11.3767659254516));
#58197=CARTESIAN_POINT('Ctrl Pts',(-0.00938418179379202,-3.10202728529954,
11.4294361380694));
#58198=CARTESIAN_POINT('Ctrl Pts',(1.07597670265583,-2.90945621671003,11.4821063506873));
#58199=CARTESIAN_POINT('Ctrl Pts',(1.83449893959343,-2.30603629574552,11.5347765633051));
#58200=CARTESIAN_POINT('Ctrl Pts',(2.59302117653101,-1.70261637478102,11.587446775923));
#58201=CARTESIAN_POINT('Ctrl Pts',(3.02470476595658,-0.688347601441517,
11.6401169885408));
#58202=CARTESIAN_POINT('Ctrl Pts',(2.93371142509181,0.27663519470765,11.6927872011586));
#58203=CARTESIAN_POINT('Ctrl Pts',(2.84271808422703,1.24161799085682,11.7454574137764));
#58204=CARTESIAN_POINT('Ctrl Pts',(2.22904781307192,2.15731480981565,11.7981276263943));
#58205=CARTESIAN_POINT('Ctrl Pts',(1.3710992699008,2.60830913596195,11.8507978390121));
#58206=CARTESIAN_POINT('Ctrl Pts',(0.513150726729663,3.05930346210826,11.9034680516299));
#58207=CARTESIAN_POINT('Ctrl Pts',(-0.5890760884575,3.04559529544201,11.9561382642478));
#58208=CARTESIAN_POINT('Ctrl Pts',(-1.43554315706074,2.57340350525938,12.0088084768656));
#58209=CARTESIAN_POINT('Ctrl Pts',(-2.28201022566397,2.10121171507676,12.0614786894834));
#58210=CARTESIAN_POINT('Ctrl Pts',(-2.87271754768328,1.17053630137777,12.1141489021013));
#58211=CARTESIAN_POINT('Ctrl Pts',(-2.93968387388293,0.203588993557491,
12.1668191147191));
#58212=CARTESIAN_POINT('Ctrl Pts',(-2.94434779339152,0.136245230376003,
12.1704873707829));
#58213=CARTESIAN_POINT('Ctrl Pts',(-2.94647129177883,0.0687255293040883,
12.1741556268466));
#58214=CARTESIAN_POINT('Ctrl Pts',(-2.94612437222716,0.00118363909654153,
12.1778238829104));
#58215=CARTESIAN_POINT('Origin',(0.,0.,0.));
#58216=CARTESIAN_POINT('',(-2.93811251051794,0.00154004898993351,13.3221761170896));
#58217=CARTESIAN_POINT('',(-2.93806927092397,0.00150371129981597,13.1778238829104));
#58218=CARTESIAN_POINT('',(-2.942,-3.60291088309151E-16,0.));
#58219=CARTESIAN_POINT('Ctrl Pts',(-2.93811251051794,0.00154004898993351,
13.3221761170896));
#58220=CARTESIAN_POINT('Ctrl Pts',(-2.93996482549542,0.387797276424435,
13.3013443661915));
#58221=CARTESIAN_POINT('Ctrl Pts',(-2.86914614049725,0.773402335775176,
13.2805126152933));
#58222=CARTESIAN_POINT('Ctrl Pts',(-2.72245263499158,1.12758166691397,13.2596808643952));
#58223=CARTESIAN_POINT('Ctrl Pts',(-2.35155831303012,2.02307531827001,13.2070106517773));
#58224=CARTESIAN_POINT('Ctrl Pts',(-1.49562542390561,2.71767636675688,13.1543404391595));
#58225=CARTESIAN_POINT('Ctrl Pts',(-0.542957881136105,2.8962709653455,13.1016702265417));
#58226=CARTESIAN_POINT('Ctrl Pts',(0.40970966163339,3.07486556393412,13.0490000139238));
#58227=CARTESIAN_POINT('Ctrl Pts',(1.45911185804788,2.7374537126245,12.996329801306));
#58228=CARTESIAN_POINT('Ctrl Pts',(2.12917519239819,2.03710622340532,12.9436595886882));
#58229=CARTESIAN_POINT('Ctrl Pts',(2.7992385267485,1.33675873418614,12.8909893760703));
#58230=CARTESIAN_POINT('Ctrl Pts',(3.08996299903463,0.273475607057396,12.8383191634525));
#58231=CARTESIAN_POINT('Ctrl Pts',(2.86945806996418,-0.67037239656747,12.7856489508347));
#58232=CARTESIAN_POINT('Ctrl Pts',(2.64895314089373,-1.61422040019232,12.7329787382168));
#58233=CARTESIAN_POINT('Ctrl Pts',(1.91721881046673,-2.4386332803133,12.680308525599));
#58234=CARTESIAN_POINT('Ctrl Pts',(1.00621487106457,-2.76960654220381,12.6276383129812));
#58235=CARTESIAN_POINT('Ctrl Pts',(0.095210931662416,-3.10057980409432,
12.5749681003633));
#58236=CARTESIAN_POINT('Ctrl Pts',(-0.9950626167149,-2.93811344775435,12.5222978877455));
#58237=CARTESIAN_POINT('Ctrl Pts',(-1.76999049402564,-2.35591222595915,
12.4696276751277));
#58238=CARTESIAN_POINT('Ctrl Pts',(-2.49313372304392,-1.81261667059929,
12.4204771557817));
#58239=CARTESIAN_POINT('Ctrl Pts',(-2.94166909896414,-0.903809548572848,
12.3713266364356));
#58240=CARTESIAN_POINT('Ctrl Pts',(-2.94616893643284,0.00113950433258347,
12.3221761170896));
#58241=CARTESIAN_POINT('Ctrl Pts',(-2.94612437222716,0.00118363909654153,
12.1778238829104));
#58242=CARTESIAN_POINT('Ctrl Pts',(-2.94149008920459,-0.901066561542921,
12.2268258394645));
#58243=CARTESIAN_POINT('Ctrl Pts',(-2.49601885931619,-1.80727633139181,
12.2758277960185));
#58244=CARTESIAN_POINT('Ctrl Pts',(-1.77658100825427,-2.35094654932331,
12.3248297525726));
#58245=CARTESIAN_POINT('Ctrl Pts',(-1.003286486046,-2.93531558244223,12.3774999651904));
#58246=CARTESIAN_POINT('Ctrl Pts',(0.0865278887505246,-3.10083444673851,
12.4301701778083));
#58247=CARTESIAN_POINT('Ctrl Pts',(0.998455145531424,-2.77241358368975,
12.4828403904261));
#58248=CARTESIAN_POINT('Ctrl Pts',(1.91038240231234,-2.44399272064099,12.5355106030439));
#58249=CARTESIAN_POINT('Ctrl Pts',(2.64442254107762,-1.62163213024718,12.5881808156617));
#58250=CARTESIAN_POINT('Ctrl Pts',(2.86756971266494,-0.678405262119501,
12.6408510282796));
#58251=CARTESIAN_POINT('Ctrl Pts',(3.09071688425225,0.264821606008148,12.6935212408974));
#58252=CARTESIAN_POINT('Ctrl Pts',(2.80297108866163,1.32891475186965,12.7461914535152));
#58253=CARTESIAN_POINT('Ctrl Pts',(2.13487155384946,2.03113593962306,12.7988616661331));
#58254=CARTESIAN_POINT('Ctrl Pts',(1.46677201903727,2.73335712737651,12.8515318787509));
#58255=CARTESIAN_POINT('Ctrl Pts',(0.418318745003505,3.07370635702182,12.9042020913687));
#58256=CARTESIAN_POINT('Ctrl Pts',(-0.534845242225581,2.8977802407252,12.9568723039866));
#58257=CARTESIAN_POINT('Ctrl Pts',(-1.48800922945464,2.7218541244286,13.0095425166044));
#58258=CARTESIAN_POINT('Ctrl Pts',(-2.34588392987902,2.02965266219009,13.0622127292222));
#58259=CARTESIAN_POINT('Ctrl Pts',(-2.71928450468353,1.13520110079642,13.1148829418401));
#58260=CARTESIAN_POINT('Ctrl Pts',(-2.86802248773115,0.778911019440369,
13.1358632555302));
#58261=CARTESIAN_POINT('Ctrl Pts',(-2.93988914006044,0.390529989491183,
13.1568435692203));
#58262=CARTESIAN_POINT('Ctrl Pts',(-2.93806927092397,0.00150371129981597,
13.1778238829104));
#58263=CARTESIAN_POINT('Origin',(0.,0.,0.));
#58264=CARTESIAN_POINT('',(-2.94078272534365,-0.002563628642199,14.3221761170896));
#58265=CARTESIAN_POINT('',(-2.94086056680551,-0.00257295723724145,14.1778238829104));
#58266=CARTESIAN_POINT('',(-2.942,-3.60291088309151E-16,0.));
#58267=CARTESIAN_POINT('Ctrl Pts',(-2.94078272534365,-0.002563628642199,
14.3221761170896));
#58268=CARTESIAN_POINT('Ctrl Pts',(-2.93476812227256,0.703069216740828,
14.2840323085651));
#58269=CARTESIAN_POINT('Ctrl Pts',(-2.67963677265994,1.41260648754648,14.2458885000406));
#58270=CARTESIAN_POINT('Ctrl Pts',(-2.21731865562784,1.9407953891895,14.2077446915161));
#58271=CARTESIAN_POINT('Ctrl Pts',(-1.578934748433,2.67013582025984,14.1550744788983));
#58272=CARTESIAN_POINT('Ctrl Pts',(-0.545508132734048,3.05369957925265,
14.1024042662805));
#58273=CARTESIAN_POINT('Ctrl Pts',(0.414135184292706,2.91747850302139,14.0497340536626));
#58274=CARTESIAN_POINT('Ctrl Pts',(1.37377850131946,2.78125742679014,13.9970638410448));
#58275=CARTESIAN_POINT('Ctrl Pts',(2.25963851967401,2.1252515153348,13.944393628427));
#58276=CARTESIAN_POINT('Ctrl Pts',(2.66983453522042,1.24706548338559,13.8917234158091));
#58277=CARTESIAN_POINT('Ctrl Pts',(3.08003055076681,0.368879451436385,13.8390532031913));
#58278=CARTESIAN_POINT('Ctrl Pts',(3.01456256350507,-0.73148670100669,13.7863829905735));
#58279=CARTESIAN_POINT('Ctrl Pts',(2.50313088767398,-1.55483906700073,13.7337127779556));
#58280=CARTESIAN_POINT('Ctrl Pts',(1.99169921184288,-2.37819143299479,13.6810425653378));
#58281=CARTESIAN_POINT('Ctrl Pts',(1.03430384744242,-2.9245300125398,13.62837235272));
#58282=CARTESIAN_POINT('Ctrl Pts',(0.0652783403102106,-2.94600195244691,
13.5757021401021));
#58283=CARTESIAN_POINT('Ctrl Pts',(-0.903747166821985,-2.96747389235401,
13.5230319274843));
#58284=CARTESIAN_POINT('Ctrl Pts',(-1.88440281668593,-2.46407919262322,
13.4703617148665));
#58285=CARTESIAN_POINT('Ctrl Pts',(-2.43180276421869,-1.66418871564523,
13.4176915022487));
#58286=CARTESIAN_POINT('Ctrl Pts',(-2.76269894649418,-1.18066527677114,
13.385853040529));
#58287=CARTESIAN_POINT('Ctrl Pts',(-2.9352815022272,-0.588800917055224,
13.3540145788093));
#58288=CARTESIAN_POINT('Ctrl Pts',(-2.93811251051794,0.00154004898993351,
13.3221761170896));
#58289=CARTESIAN_POINT('Ctrl Pts',(-2.93806927092397,0.00150371129981597,
13.1778238829104));
#58290=CARTESIAN_POINT('Ctrl Pts',(-2.93532043361636,-0.586104444526946,
13.2095137818381));
#58291=CARTESIAN_POINT('Ctrl Pts',(-2.76445685036328,-1.17518472499942,
13.2412036807658));
#58292=CARTESIAN_POINT('Ctrl Pts',(-2.43645366085186,-1.65737241294204,
13.2728935796936));
#58293=CARTESIAN_POINT('Ctrl Pts',(-1.89129579303109,-2.45879270473794,
13.3255637923114));
#58294=CARTESIAN_POINT('Ctrl Pts',(-0.912053608204924,-2.96493162778095,
13.3782340049292));
#58295=CARTESIAN_POINT('Ctrl Pts',(0.0570282834555854,-2.94617337092987,
13.4309042175471));
#58296=CARTESIAN_POINT('Ctrl Pts',(1.02611017511611,-2.9274151140788,13.4835744301649));
#58297=CARTESIAN_POINT('Ctrl Pts',(1.98503177361097,-2.38375967733365,13.5362446427827));
#58298=CARTESIAN_POINT('Ctrl Pts',(2.49876713918657,-1.56184267477676,13.5889148554006));
#58299=CARTESIAN_POINT('Ctrl Pts',(3.01250250476216,-0.739925672219871,
13.6415850680184));
#58300=CARTESIAN_POINT('Ctrl Pts',(3.08105163741847,0.360252896148758,13.6942552806362));
#58301=CARTESIAN_POINT('Ctrl Pts',(2.67331642557935,1.23958422278181,13.746925493254));
#58302=CARTESIAN_POINT('Ctrl Pts',(2.26558121374023,2.11891554941484,13.7995957058719));
#58303=CARTESIAN_POINT('Ctrl Pts',(1.38156165740569,2.77739963431232,13.8522659184897));
#58304=CARTESIAN_POINT('Ctrl Pts',(0.422303513476949,2.91630751110678,13.9049361311075));
#58305=CARTESIAN_POINT('Ctrl Pts',(-0.536954630451802,3.05521538790123,
13.9576063437254));
#58306=CARTESIAN_POINT('Ctrl Pts',(-1.57145136197473,2.67454705659267,14.0102765563432));
#58307=CARTESIAN_POINT('Ctrl Pts',(-2.2118752029893,1.94699713476955,14.062946768961));
#58308=CARTESIAN_POINT('Ctrl Pts',(-2.67747703562242,1.41805277755094,14.1012391402775));
#58309=CARTESIAN_POINT('Ctrl Pts',(-2.9347876598567,0.70576065041498,14.1395315115939));
#58310=CARTESIAN_POINT('Ctrl Pts',(-2.94086056680551,-0.00257295723724145,
14.1778238829104));
#58311=CARTESIAN_POINT('Origin',(0.,0.,0.));
#58312=CARTESIAN_POINT('',(-2.94636756759144,0.000915173715594336,15.3221761170896));
#58313=CARTESIAN_POINT('',(-2.94633063485147,0.000961351460667442,15.1778238829104));
#58314=CARTESIAN_POINT('',(-2.942,-3.60291088309151E-16,0.));
#58315=CARTESIAN_POINT('Ctrl Pts',(-2.94636756759144,0.000915173715594336,
15.3221761170896));
#58316=CARTESIAN_POINT('Ctrl Pts',(-2.94657828982524,0.0521948370493097,
15.3193904635566));
#58317=CARTESIAN_POINT('Ctrl Pts',(-2.94535428898749,0.10346423759929,15.3166048100236));
#58318=CARTESIAN_POINT('Ctrl Pts',(-2.94266379286899,0.154656563808966,
15.3138191564906));
#58319=CARTESIAN_POINT('Ctrl Pts',(-2.89179278506782,1.12258408024949,15.2611489438728));
#58320=CARTESIAN_POINT('Ctrl Pts',(-2.31664983854732,2.06295752655595,15.2084787312549));
#58321=CARTESIAN_POINT('Ctrl Pts',(-1.47815528586474,2.54916566805956,15.1558085186371));
#58322=CARTESIAN_POINT('Ctrl Pts',(-0.63966073318215,3.03537380956318,15.1031383060193));
#58323=CARTESIAN_POINT('Ctrl Pts',(0.462185425662502,3.06741664626393,15.0504680934014));
#58324=CARTESIAN_POINT('Ctrl Pts',(1.32751788394718,2.63075750962818,14.9977978807836));
#58325=CARTESIAN_POINT('Ctrl Pts',(2.19285034223184,2.19409837299243,14.9451276681658));
#58326=CARTESIAN_POINT('Ctrl Pts',(2.82166909995653,1.28873726302021,14.8924574555479));
#58327=CARTESIAN_POINT('Ctrl Pts',(2.92870319978326,0.325401813616169,14.8397872429301));
#58328=CARTESIAN_POINT('Ctrl Pts',(3.03573729960999,-0.637933635787871,
14.7871170303123));
#58329=CARTESIAN_POINT('Ctrl Pts',(2.62098674153875,-1.65924342462374,14.7344468176944));
#58330=CARTESIAN_POINT('Ctrl Pts',(1.87260794788981,-2.27519850196241,14.6817766050766));
#58331=CARTESIAN_POINT('Ctrl Pts',(1.12422915424088,-2.89115357930107,14.6291063924588));
#58332=CARTESIAN_POINT('Ctrl Pts',(0.0422221250142511,-3.10175394514255,
14.576436179841));
#58333=CARTESIAN_POINT('Ctrl Pts',(-0.882548065597691,-2.81145828426204,
14.5237659672231));
#58334=CARTESIAN_POINT('Ctrl Pts',(-1.80731825620963,-2.52116262338152,
14.4710957546053));
#58335=CARTESIAN_POINT('Ctrl Pts',(-2.57485160820688,-1.72997093577902,
14.4184255419874));
#58336=CARTESIAN_POINT('Ctrl Pts',(-2.83694768486014,-0.796816540403842,
14.3657553293696));
#58337=CARTESIAN_POINT('Ctrl Pts',(-2.90923358103393,-0.539453276521613,
14.3512289252763));
#58338=CARTESIAN_POINT('Ctrl Pts',(-2.94307328200413,-0.271291588698562,
14.3367025211829));
#58339=CARTESIAN_POINT('Ctrl Pts',(-2.94078272534365,-0.002563628642199,
14.3221761170896));
#58340=CARTESIAN_POINT('Ctrl Pts',(-2.94086056680551,-0.00257295723724145,
14.1778238829104));
#58341=CARTESIAN_POINT('Ctrl Pts',(-2.94314079363258,-0.268534762399236,
14.1922017242118));
#58342=CARTESIAN_POINT('Ctrl Pts',(-2.91000109139948,-0.533938488619848,
14.2065795655132));
#58343=CARTESIAN_POINT('Ctrl Pts',(-2.83916807956566,-0.788869046535997,
14.2209574068145));
#58344=CARTESIAN_POINT('Ctrl Pts',(-2.57968616462127,-1.72275379368075,
14.2736276194324));
#58345=CARTESIAN_POINT('Ctrl Pts',(-1.81437138422634,-2.51609177563258,
14.3262978320502));
#58346=CARTESIAN_POINT('Ctrl Pts',(-0.890417692713573,-2.80897598605912,
14.378968044668));
#58347=CARTESIAN_POINT('Ctrl Pts',(0.0335359987991893,-3.10186019648566,
14.4316382572858));
#58348=CARTESIAN_POINT('Ctrl Pts',(1.11612860142979,-2.89429063538687,14.4843084699037));
#58349=CARTESIAN_POINT('Ctrl Pts',(1.86622938578629,-2.28043365047774,14.5369786825215));
#58350=CARTESIAN_POINT('Ctrl Pts',(2.61633017014279,-1.66657666556861,14.5896488951393));
#58351=CARTESIAN_POINT('Ctrl Pts',(3.03393913622522,-0.646432256849133,
14.6423191077572));
#58352=CARTESIAN_POINT('Ctrl Pts',(2.92960311741482,0.317199198340533,14.694989320375));
#58353=CARTESIAN_POINT('Ctrl Pts',(2.82526709860441,1.28083065353021,14.7476595329928));
#58354=CARTESIAN_POINT('Ctrl Pts',(2.19898609490117,2.18794915519006,14.8003297456107));
#58355=CARTESIAN_POINT('Ctrl Pts',(1.33487977102078,2.62702983622557,14.8529999582285));
#58356=CARTESIAN_POINT('Ctrl Pts',(0.470773447140396,3.06611051726107,14.9056701708463));
#58357=CARTESIAN_POINT('Ctrl Pts',(-0.631158196917155,3.03715337767223,
14.9583403834642));
#58358=CARTESIAN_POINT('Ctrl Pts',(-1.47101105209001,2.55329517013352,15.011010596082));
#58359=CARTESIAN_POINT('Ctrl Pts',(-2.31086390726285,2.06943696259481,15.0636808086998));
#58360=CARTESIAN_POINT('Ctrl Pts',(-2.88863797355103,1.13067768710628,15.1163510213177));
#58361=CARTESIAN_POINT('Ctrl Pts',(-2.94221932036621,0.162896393065324,
15.1690212339355));
#58362=CARTESIAN_POINT('Ctrl Pts',(-2.94520429526425,0.108982054564796,
15.1719554502605));
#58363=CARTESIAN_POINT('Ctrl Pts',(-2.94656242919711,0.0549776457391388,
15.1748896665854));
#58364=CARTESIAN_POINT('Ctrl Pts',(-2.94633063485147,0.000961351460667442,
15.1778238829104));
#58365=CARTESIAN_POINT('Origin',(0.,0.,0.));
#58366=CARTESIAN_POINT('',(-2.93834196467696,0.0017116903336982,16.3221761170896));
#58367=CARTESIAN_POINT('',(-2.93829399889148,0.00167873273706156,16.1778238829104));
#58368=CARTESIAN_POINT('',(-2.942,-3.60291088309151E-16,0.));
#58369=CARTESIAN_POINT('Ctrl Pts',(-2.93834196467696,0.0017116903336982,
16.3221761170896));
#58370=CARTESIAN_POINT('Ctrl Pts',(-2.9403397843927,0.374286552436328,16.3020784059303));
#58371=CARTESIAN_POINT('Ctrl Pts',(-2.87457680364825,0.746182656532499,
16.2819806947709));
#58372=CARTESIAN_POINT('Ctrl Pts',(-2.73779374054997,1.08980790041183,16.2618829836116));
#58373=CARTESIAN_POINT('Ctrl Pts',(-2.37932540757495,1.99034898752761,16.2092127709937));
#58374=CARTESIAN_POINT('Ctrl Pts',(-1.53308367358257,2.69672283094819,16.1565425583759));
#58375=CARTESIAN_POINT('Ctrl Pts',(-0.582978050092166,2.88848054283463,
16.1038723457581));
#58376=CARTESIAN_POINT('Ctrl Pts',(0.367127573398249,3.08023825472107,16.0512021331402));
#58377=CARTESIAN_POINT('Ctrl Pts',(1.4210970863867,2.75737983507336,15.9985319205224));
#58378=CARTESIAN_POINT('Ctrl Pts',(2.10078605818236,2.06637071241156,15.9458617079046));
#58379=CARTESIAN_POINT('Ctrl Pts',(2.78047502997801,1.37536158974976,15.8931914952867));
#58380=CARTESIAN_POINT('Ctrl Pts',(3.08588346058089,0.316201764073922,15.8405212826689));
#58381=CARTESIAN_POINT('Ctrl Pts',(2.87845868549279,-0.630606989902349,
15.7878510700511));
#58382=CARTESIAN_POINT('Ctrl Pts',(2.67103391040469,-1.57741574387861,15.7351808574333));
#58383=CARTESIAN_POINT('Ctrl Pts',(1.95077592962559,-2.41187342615528,15.6825106448154));
#58384=CARTESIAN_POINT('Ctrl Pts',(1.04443845795601,-2.75541943685174,15.6298404321976));
#58385=CARTESIAN_POINT('Ctrl Pts',(0.138100986286415,-3.0989654475482,15.5771702195797));
#58386=CARTESIAN_POINT('Ctrl Pts',(-0.954315976273691,-2.95159978666445,
15.5245000069619));
#58387=CARTESIAN_POINT('Ctrl Pts',(-1.73722492301283,-2.38017616293528,
15.4718297943441));
#58388=CARTESIAN_POINT('Ctrl Pts',(-2.47872691570511,-1.83897433169884,
15.4219452352593));
#58389=CARTESIAN_POINT('Ctrl Pts',(-2.94259402375403,-0.917384020750813,
15.3720606761744));
#58390=CARTESIAN_POINT('Ctrl Pts',(-2.94636756759144,0.000915173715594336,
15.3221761170896));
#58391=CARTESIAN_POINT('Ctrl Pts',(-2.94633063485147,0.000961351460667442,
15.1778238829104));
#58392=CARTESIAN_POINT('Ctrl Pts',(-2.94240163935874,-0.914633790291091,
15.2275598792033));
#58393=CARTESIAN_POINT('Ctrl Pts',(-2.48166336201514,-1.83364379373038,
15.2772958754961));
#58394=CARTESIAN_POINT('Ctrl Pts',(-1.74388353322011,-2.37530209033153,
15.327031871789));
#58395=CARTESIAN_POINT('Ctrl Pts',(-0.962577771916698,-2.94891596709401,
15.3797020844068));
#58396=CARTESIAN_POINT('Ctrl Pts',(0.129422378032284,-3.09934040802562,
15.4323722970246));
#58397=CARTESIAN_POINT('Ctrl Pts',(1.03671835568921,-2.75833368087526,15.4850425096425));
#58398=CARTESIAN_POINT('Ctrl Pts',(1.94401433334615,-2.4173269537249,15.5377127222603));
#58399=CARTESIAN_POINT('Ctrl Pts',(2.66660613871103,-1.58488905849257,15.5903829348781));
#58400=CARTESIAN_POINT('Ctrl Pts',(2.87668156935298,-0.638665006267767,
15.643053147496));
#58401=CARTESIAN_POINT('Ctrl Pts',(3.08675699999493,0.307559045957031,15.6957233601138));
#58402=CARTESIAN_POINT('Ctrl Pts',(2.78431605591395,1.36756925517429,15.7483935727317));
#58403=CARTESIAN_POINT('Ctrl Pts',(2.10656463391492,2.06047941828124,15.8010637853495));
#58404=CARTESIAN_POINT('Ctrl Pts',(1.42881321191589,2.75338958138818,15.8537339979673));
#58405=CARTESIAN_POINT('Ctrl Pts',(0.375751311998833,3.07919969838482,15.9064042105851));
#58406=CARTESIAN_POINT('Ctrl Pts',(-0.574887366656207,2.8901026755206,15.959074423203));
#58407=CARTESIAN_POINT('Ctrl Pts',(-1.52552604531125,2.70100565265638,16.0117446358208));
#58408=CARTESIAN_POINT('Ctrl Pts',(-2.37374150270427,1.9970014899313,16.0644148484386));
#58409=CARTESIAN_POINT('Ctrl Pts',(-2.73473076831818,1.09746899458998,16.1170850610565));
#58410=CARTESIAN_POINT('Ctrl Pts',(-2.87349397434761,0.751691363864775,
16.1373313350078));
#58411=CARTESIAN_POINT('Ctrl Pts',(-2.94026410906292,0.377022254332635,
16.1575776089591));
#58412=CARTESIAN_POINT('Ctrl Pts',(-2.93829399889148,0.00167873273706156,
16.1778238829104));
#58413=CARTESIAN_POINT('Origin',(0.,0.,0.));
#58414=CARTESIAN_POINT('',(-2.94033980469539,-0.00268911818531531,17.3221761170896));
#58415=CARTESIAN_POINT('',(-2.94047623996122,-0.00254690177668123,17.1778238829104));
#58416=CARTESIAN_POINT('',(-2.942,-3.60291088309151E-16,0.));
#58417=CARTESIAN_POINT('Ctrl Pts',(-2.94033980469539,-0.00268911818531531,
17.3221761170896));
#58418=CARTESIAN_POINT('Ctrl Pts',(-2.9346462523403,0.689633572098389,17.2847663483039));
#58419=CARTESIAN_POINT('Ctrl Pts',(-2.69018060245738,1.38571321721952,17.2473565795182));
#58420=CARTESIAN_POINT('Ctrl Pts',(-2.24398877650981,1.91001340457724,17.2099468107325));
#58421=CARTESIAN_POINT('Ctrl Pts',(-1.61578338781506,2.64818964142855,17.1572765981147));
#58422=CARTESIAN_POINT('Ctrl Pts',(-0.587704750385148,3.04585473995439,
17.1046063854969));
#58423=CARTESIAN_POINT('Ctrl Pts',(0.373745236161002,2.92288602380855,17.051936172879));
#58424=CARTESIAN_POINT('Ctrl Pts',(1.33519522270717,2.79991730766271,16.9992659602612));
#58425=CARTESIAN_POINT('Ctrl Pts',(2.23001655836957,2.15631477684517,16.9465957476434));
#58426=CARTESIAN_POINT('Ctrl Pts',(2.65231656865006,1.28390822131956,16.8939255350255));
#58427=CARTESIAN_POINT('Ctrl Pts',(3.07461657893055,0.411501665793941,16.8412553224077));
#58428=CARTESIAN_POINT('Ctrl Pts',(3.02439526382914,-0.689708914439747,
16.7885851097899));
#58429=CARTESIAN_POINT('Ctrl Pts',(2.52440812832174,-1.52006904496187,16.735914897172));
#58430=CARTESIAN_POINT('Ctrl Pts',(2.02442099281435,-2.35042917548398,16.6832446845542));
#58431=CARTESIAN_POINT('Ctrl Pts',(1.074668036901,-2.90993885629453,16.6305744719364));
#58432=CARTESIAN_POINT('Ctrl Pts',(0.106030389206343,-2.94481058190328,
16.5779042593186));
#58433=CARTESIAN_POINT('Ctrl Pts',(-0.862607258488317,-2.97968230751204,
16.5252340467007));
#58434=CARTESIAN_POINT('Ctrl Pts',(-1.85012959796428,-2.489916077919,16.4725638340829));
#58435=CARTESIAN_POINT('Ctrl Pts',(-2.40854330172345,-1.69767879771699,
16.4198936214651));
#58436=CARTESIAN_POINT('Ctrl Pts',(-2.75387950365051,-1.20774058250446,
16.3873211200066));
#58437=CARTESIAN_POINT('Ctrl Pts',(-2.93510408424925,-0.602123002234626,
16.3547486185481));
#58438=CARTESIAN_POINT('Ctrl Pts',(-2.93834196467696,0.0017116903336982,
16.3221761170896));
#58439=CARTESIAN_POINT('Ctrl Pts',(-2.93829399889148,0.00167873273706156,
16.1778238829104));
#58440=CARTESIAN_POINT('Ctrl Pts',(-2.93513891309551,-0.599425221124181,
16.2102478215769));
#58441=CARTESIAN_POINT('Ctrl Pts',(-2.75568379353507,-1.20225885851725,
16.2426717602434));
#58442=CARTESIAN_POINT('Ctrl Pts',(-2.41328914510403,-1.69092473863608,
16.27509569891));
#58443=CARTESIAN_POINT('Ctrl Pts',(-1.85709518244114,-2.48472514856328,
16.3277659115278));
#58444=CARTESIAN_POINT('Ctrl Pts',(-0.870944183280553,-2.97726514046012,
16.3804361241456));
#58445=CARTESIAN_POINT('Ctrl Pts',(0.0977855608398415,-2.94510139794416,
16.4331063367635));
#58446=CARTESIAN_POINT('Ctrl Pts',(1.06651530496021,-2.9129376554282,16.4857765493813));
#58447=CARTESIAN_POINT('Ctrl Pts',(2.01782379404038,-2.35607017849948,16.5384467619991));
#58448=CARTESIAN_POINT('Ctrl Pts',(2.52013775106141,-1.5271222999678,16.591116974617));
#58449=CARTESIAN_POINT('Ctrl Pts',(3.02245170808247,-0.698174421436078,
16.6437871872348));
#58450=CARTESIAN_POINT('Ctrl Pts',(3.07577113304434,0.40285385869867,16.6964573998526));
#58451=CARTESIAN_POINT('Ctrl Pts',(2.65590917431802,1.27645664321552,16.7491276124704));
#58452=CARTESIAN_POINT('Ctrl Pts',(2.23604721559172,2.15005942773234,16.8017978250883));
#58453=CARTESIAN_POINT('Ctrl Pts',(1.34300387317732,2.79623671663129,16.8544680377061));
#58454=CARTESIAN_POINT('Ctrl Pts',(0.38191458879571,2.92186483790969,16.9071382503239));
#58455=CARTESIAN_POINT('Ctrl Pts',(-0.579174695585912,3.04749295918809,
16.9598084629418));
#58456=CARTESIAN_POINT('Ctrl Pts',(-1.60830992193471,2.65257191284588,17.0124786755596));
#58457=CARTESIAN_POINT('Ctrl Pts',(-2.2386041647435,1.91621987213004,17.0651488881774));
#58458=CARTESIAN_POINT('Ctrl Pts',(-2.68805745126554,1.39113837485648,17.1027072197551));
#58459=CARTESIAN_POINT('Ctrl Pts',(-2.93470407488486,0.69244262168104,17.1402655513327));
#58460=CARTESIAN_POINT('Ctrl Pts',(-2.94047623996122,-0.00254690177668123,
17.1778238829104));
#58461=CARTESIAN_POINT('Origin',(0.,0.,-1.848589891905));
#58462=CARTESIAN_POINT('',(-2.3704116015589,-0.00216788445160201,17.651410108095));
#58463=CARTESIAN_POINT('',(-2.37524114860369,0.000101641450047634,17.848589891905));
#58464=CARTESIAN_POINT('',(-2.37175,-3.45929798001232E-13,-1.848589891905));
#58465=CARTESIAN_POINT('',(1.37994918219948,-1.93347698736443,18.));
#58466=CARTESIAN_POINT('Ctrl Pts',(-2.3704116015589,-0.00216788445160182,
17.651410108095));
#58467=CARTESIAN_POINT('Ctrl Pts',(-2.37228397167149,-0.229843724195573,
17.6666705519271));
#58468=CARTESIAN_POINT('Ctrl Pts',(-2.23803403881605,-1.24108118812309,
17.7346012083771));
#58469=CARTESIAN_POINT('Ctrl Pts',(-0.854011012564108,-2.62815348477828,
17.8507978390121));
#58470=CARTESIAN_POINT('Ctrl Pts',(0.794121156913562,-2.34631857250555,
17.951734025815));
#58471=CARTESIAN_POINT('Ctrl Pts',(1.37994918219948,-1.93347698736443,18.));
#58472=CARTESIAN_POINT('',(-1.37702479013092,-1.93106208855772,18.));
#58473=CARTESIAN_POINT('Origin',(0.,0.,18.));
#58474=CARTESIAN_POINT('Ctrl Pts',(-2.37524114860369,0.000101641450047495,
17.848589891905));
#58475=CARTESIAN_POINT('Ctrl Pts',(-2.37291161402036,-0.747323183496906,
17.8990599279367));
#58476=CARTESIAN_POINT('Ctrl Pts',(-1.98938888825758,-1.49439019245295,
17.9495299639683));
#58477=CARTESIAN_POINT('Ctrl Pts',(-1.37702479013086,-1.93106208855776,
18.));
#58478=CARTESIAN_POINT('Origin',(0.,0.,-1.848589891905));
#58479=CARTESIAN_POINT('',(-2.36880100432447,0.00137991215103788,16.651410108095));
#58480=CARTESIAN_POINT('',(-2.37052159147792,-0.00205323395313789,16.848589891905));
#58481=CARTESIAN_POINT('',(-2.37175,-3.45929798001232E-13,-1.848589891905));
#58482=CARTESIAN_POINT('Ctrl Pts',(-2.36880100432447,0.00137991215103789,
16.651410108095));
#58483=CARTESIAN_POINT('Ctrl Pts',(-2.36619072461524,-0.485413062729584,
16.6839826095535));
#58484=CARTESIAN_POINT('Ctrl Pts',(-1.98385093138572,-1.76311887753393,
16.7692253236298));
#58485=CARTESIAN_POINT('Ctrl Pts',(0.100702699977133,-2.79696280349387,
16.9071382503239));
#58486=CARTESIAN_POINT('Ctrl Pts',(2.39768764884266,-1.44378426631252,17.0651488881774));
#58487=CARTESIAN_POINT('Ctrl Pts',(2.51914829203609,1.21950213103884,17.2231595260309));
#58488=CARTESIAN_POINT('Ctrl Pts',(0.35501589619246,2.77605988338393,17.3811701638844));
#58489=CARTESIAN_POINT('Ctrl Pts',(-1.89126576511015,1.90718878185824,17.5239203579058));
#58490=CARTESIAN_POINT('Ctrl Pts',(-2.36582163459831,0.555961395181473,
17.6140003393093));
#58491=CARTESIAN_POINT('Ctrl Pts',(-2.3704116015589,-0.00216788445160182,
17.651410108095));
#58492=CARTESIAN_POINT('Ctrl Pts',(-2.37052159147792,-0.0020532339531374,
16.848589891905));
#58493=CARTESIAN_POINT('Ctrl Pts',(-2.37239389915549,-0.227485840854584,
16.8637017729452));
#58494=CARTESIAN_POINT('Ctrl Pts',(-2.23978575228814,-1.23646065412646,
16.9314838666032));
#58495=CARTESIAN_POINT('Ctrl Pts',(-0.80874814078054,-2.6792673034923,17.051936172879));
#58496=CARTESIAN_POINT('Ctrl Pts',(1.80238833174315,-2.14148580062739,17.2099468107325));
#58497=CARTESIAN_POINT('Ctrl Pts',(2.77800430721521,0.340253358304015,17.367957448586));
#58498=CARTESIAN_POINT('Ctrl Pts',(1.23340008456365,2.51147754111133,17.5259680864395));
#58499=CARTESIAN_POINT('Ctrl Pts',(-1.43092211742628,2.4074435208734,17.683978724293));
#58500=CARTESIAN_POINT('Ctrl Pts',(-2.35980886491538,0.845292509076889,
17.7915193261149));
#58501=CARTESIAN_POINT('Ctrl Pts',(-2.37534270168053,0.0326846695014218,
17.8463897153189));
#58502=CARTESIAN_POINT('Ctrl Pts',(-2.37524114860369,0.000101641450047495,
17.848589891905));
#58503=CARTESIAN_POINT('Origin',(0.,0.,-1.848589891905));
#58504=CARTESIAN_POINT('',(-2.37527099878824,0.000737784928405548,15.651410108095));
#58505=CARTESIAN_POINT('',(-2.36876233578207,0.00135334274909457,15.848589891905));
#58506=CARTESIAN_POINT('',(-2.37175,-3.45929798001232E-13,-1.848589891905));
#58507=CARTESIAN_POINT('Ctrl Pts',(-2.37527099878824,0.000737784928405679,
15.651410108095));
#58508=CARTESIAN_POINT('Ctrl Pts',(-2.37222888369763,-0.739566808707072,
15.7012946671798));
#58509=CARTESIAN_POINT('Ctrl Pts',(-1.60343564769808,-2.26697063865214,
15.8038494388825));
#58510=CARTESIAN_POINT('Ctrl Pts',(0.992005759747417,-2.61709238831523,
15.959074423203));
#58511=CARTESIAN_POINT('Ctrl Pts',(2.73395531710238,-0.598949960096589,
16.1170850610565));
#58512=CARTESIAN_POINT('Ctrl Pts',(1.99532264006382,1.96263635861182,16.2750956989099));
#58513=CARTESIAN_POINT('Ctrl Pts',(-0.553710866833194,2.74347197057582,
16.4331063367635));
#58514=CARTESIAN_POINT('Ctrl Pts',(-2.17845584047471,1.38726687514169,16.5585444731585));
#58515=CARTESIAN_POINT('Ctrl Pts',(-2.37041158519152,0.301738317722773,
16.6313123969356));
#58516=CARTESIAN_POINT('Ctrl Pts',(-2.36880100432447,0.00137991215103789,
16.651410108095));
#58517=CARTESIAN_POINT('Ctrl Pts',(-2.36876233578207,0.00135334274909471,
15.848589891905));
#58518=CARTESIAN_POINT('Ctrl Pts',(-2.36621880256085,-0.483238194494291,
15.8810138305715));
#58519=CARTESIAN_POINT('Ctrl Pts',(-1.98654027620114,-1.75867122558308,
15.9661079818559));
#58520=CARTESIAN_POINT('Ctrl Pts',(0.0928761949570627,-2.79725027962867,
16.1038723457581));
#58521=CARTESIAN_POINT('Ctrl Pts',(2.39362321294746,-1.45046193319176,16.2618829836116));
#58522=CARTESIAN_POINT('Ctrl Pts',(2.52257665905884,1.21238356994498,16.4198936214651));
#58523=CARTESIAN_POINT('Ctrl Pts',(0.362744353785385,2.77516839483905,16.5779042593186));
#58524=CARTESIAN_POINT('Ctrl Pts',(-1.88818603203603,1.91139484938775,16.7208030161319));
#58525=CARTESIAN_POINT('Ctrl Pts',(-2.36586824935706,0.558225964640069,
16.8110315603274));
#58526=CARTESIAN_POINT('Ctrl Pts',(-2.37052159147792,-0.0020532339531374,
16.848589891905));
#58527=CARTESIAN_POINT('Origin',(0.,0.,-1.848589891905));
#58528=CARTESIAN_POINT('',(-2.37076867057573,-0.00206671863790898,14.651410108095));
#58529=CARTESIAN_POINT('',(-2.37524122474812,0.000775012007393425,14.848589891905));
#58530=CARTESIAN_POINT('',(-2.37175,-3.45929798001232E-13,-1.848589891905));
#58531=CARTESIAN_POINT('Ctrl Pts',(-2.37076867057573,-0.00206671863790864,
14.651410108095));
#58532=CARTESIAN_POINT('Ctrl Pts',(-2.37261524697255,-0.218706942724769,
14.6659365121883));
#58533=CARTESIAN_POINT('Ctrl Pts',(-2.24642027727927,-1.21873516689608,
14.7331331288995));
#58534=CARTESIAN_POINT('Ctrl Pts',(-0.838242639893101,-2.67031826549166,
14.8529999582285));
#58535=CARTESIAN_POINT('Ctrl Pts',(1.77859981921798,-2.16097963427009,15.011010596082));
#58536=CARTESIAN_POINT('Ctrl Pts',(2.78167728635466,0.309066074436347,15.1690212339355));
#58537=CARTESIAN_POINT('Ctrl Pts',(1.26087420481122,2.49868899684622,15.327031871789));
#58538=CARTESIAN_POINT('Ctrl Pts',(-1.40394934437959,2.42119314578055,15.4850425096425));
#58539=CARTESIAN_POINT('Ctrl Pts',(-2.35579694789029,0.86489793832459,15.5931685884112));
#58540=CARTESIAN_POINT('Ctrl Pts',(-2.37544087657819,0.0420778738175528,
15.648624454562));
#58541=CARTESIAN_POINT('Ctrl Pts',(-2.37527099878824,0.000737784928405679,
15.651410108095));
#58542=CARTESIAN_POINT('Ctrl Pts',(-2.37524122474812,0.000775012007393572,
14.848589891905));
#58543=CARTESIAN_POINT('Ctrl Pts',(-2.37207378930956,-0.737349657417977,
14.8983258881979));
#58544=CARTESIAN_POINT('Ctrl Pts',(-1.60729470532651,-2.26281359901547,
15.0007320971086));
#58545=CARTESIAN_POINT('Ctrl Pts',(0.984673310924482,-2.61986056441679,
15.1558085186371));
#58546=CARTESIAN_POINT('Ctrl Pts',(2.73226724128555,-0.606603006955222,
15.3138191564906));
#58547=CARTESIAN_POINT('Ctrl Pts',(2.0008114535995,1.95703997099618,15.4718297943441));
#58548=CARTESIAN_POINT('Ctrl Pts',(-0.546026983988871,2.74501428607443,
15.6298404321976));
#58549=CARTESIAN_POINT('Ctrl Pts',(-2.17649017174337,1.39175803337991,15.7554271313846));
#58550=CARTESIAN_POINT('Ctrl Pts',(-2.37035057806599,0.303943756530424,
15.8283436179537));
#58551=CARTESIAN_POINT('Ctrl Pts',(-2.36876233578207,0.00135334274909471,
15.848589891905));
#58552=CARTESIAN_POINT('Origin',(0.,0.,-1.848589891905));
#58553=CARTESIAN_POINT('',(-2.36861602543199,0.00124154017382057,13.651410108095));
#58554=CARTESIAN_POINT('',(-2.37083142397042,-0.00207423906479154,13.848589891905));
#58555=CARTESIAN_POINT('',(-2.37175,-3.45929798001232E-13,-1.848589891905));
#58556=CARTESIAN_POINT('Ctrl Pts',(-2.36861602543199,0.00124154017382031,
13.651410108095));
#58557=CARTESIAN_POINT('Ctrl Pts',(-2.36633375353748,-0.474673207010919,
13.6832485698147));
#58558=CARTESIAN_POINT('Ctrl Pts',(-1.99703967034429,-1.74115118427591,
13.7677572441522));
#58559=CARTESIAN_POINT('Ctrl Pts',(0.0620012558310767,-2.79810760818394,
13.9049361311075));
#58560=CARTESIAN_POINT('Ctrl Pts',(2.37746942936956,-1.4767834823825,14.062946768961));
#58561=CARTESIAN_POINT('Ctrl Pts',(2.53580426837836,1.18446065975573,14.2209574068145));
#58562=CARTESIAN_POINT('Ctrl Pts',(0.393344888501637,2.77101608514062,14.378968044668));
#58563=CARTESIAN_POINT('Ctrl Pts',(-1.87623249328146,1.9286460332593,14.5224522784282));
#58564=CARTESIAN_POINT('Ctrl Pts',(-2.36591988239296,0.56679279904984,14.6132662995705));
#58565=CARTESIAN_POINT('Ctrl Pts',(-2.37076867057573,-0.00206671863790864,
14.651410108095));
#58566=CARTESIAN_POINT('Ctrl Pts',(-2.37083142397042,-0.00207423906479159,
13.848589891905));
#58567=CARTESIAN_POINT('Ctrl Pts',(-2.37266967277294,-0.216484474072482,
13.8629677332064));
#58568=CARTESIAN_POINT('Ctrl Pts',(-2.24808422025942,-1.21424369041544,
13.9300157871256));
#58569=CARTESIAN_POINT('Ctrl Pts',(-0.845717199230744,-2.66796058040481,
14.0497340536626));
#58570=CARTESIAN_POINT('Ctrl Pts',(1.77254147373567,-2.16595197414774,14.2077446915161));
#58571=CARTESIAN_POINT('Ctrl Pts',(2.78253202299393,0.301275253636565,14.3657553293696));
#58572=CARTESIAN_POINT('Ctrl Pts',(1.26786651939106,2.49514844158187,14.5237659672231));
#58573=CARTESIAN_POINT('Ctrl Pts',(-1.3971637764554,2.42511537310475,14.6817766050766));
#58574=CARTESIAN_POINT('Ctrl Pts',(-2.3546796192857,0.86935693510682,14.7900512466373));
#58575=CARTESIAN_POINT('Ctrl Pts',(-2.37542809022715,0.0443212886747152,
14.8456556755801));
#58576=CARTESIAN_POINT('Ctrl Pts',(-2.37524122474812,0.000775012007393572,
14.848589891905));
#58577=CARTESIAN_POINT('Origin',(0.,0.,-1.848589891905));
#58578=CARTESIAN_POINT('',(-2.37511086845159,0.000918633378760274,12.651410108095));
#58579=CARTESIAN_POINT('',(-2.36858116699997,0.0012122458443739,12.848589891905));
#58580=CARTESIAN_POINT('',(-2.37175,-3.45929798001232E-13,-1.848589891905));
#58581=CARTESIAN_POINT('Ctrl Pts',(-2.37511086845159,0.000918633378760338,
12.651410108095));
#58582=CARTESIAN_POINT('Ctrl Pts',(-2.37148323775257,-0.728623486345359,
12.700560627441));
#58583=CARTESIAN_POINT('Ctrl Pts',(-1.62239833212739,-2.24639384244693,
12.8023813594049));
#58584=CARTESIAN_POINT('Ctrl Pts',(0.955701160956647,-2.63056754962948,
12.9568723039866));
#58585=CARTESIAN_POINT('Ctrl Pts',(2.725406359655,-0.636718553952737,13.1148829418401));
#58586=CARTESIAN_POINT('Ctrl Pts',(2.02228695060197,1.93484000155462,13.2728935796935));
#58587=CARTESIAN_POINT('Ctrl Pts',(-0.515700465454569,2.75087320176898,
13.4309042175471));
#58588=CARTESIAN_POINT('Ctrl Pts',(-2.16866858426475,1.4094673473738,13.5570763936809));
#58589=CARTESIAN_POINT('Ctrl Pts',(-2.37010930485004,0.312630248252637,
13.6305783571968));
#58590=CARTESIAN_POINT('Ctrl Pts',(-2.36861602543199,0.00124154017382031,
13.651410108095));
#58591=CARTESIAN_POINT('Ctrl Pts',(-2.36858116699997,0.00121224584437404,
12.848589891905));
#58592=CARTESIAN_POINT('Ctrl Pts',(-2.36636513882711,-0.472499393714349,
12.8802797908327));
#58593=CARTESIAN_POINT('Ctrl Pts',(-1.9996810697703,-1.73670297725242,12.9646399023783));
#58594=CARTESIAN_POINT('Ctrl Pts',(0.0541653659420804,-2.79827042111378,
13.1016702265417));
#58595=CARTESIAN_POINT('Ctrl Pts',(2.37332474856975,-1.48343549715007,13.2596808643952));
#58596=CARTESIAN_POINT('Ctrl Pts',(2.53911136180312,1.17735497143754,13.4176915022487));
#58597=CARTESIAN_POINT('Ctrl Pts',(0.401103153710141,2.76990387866618,13.5757021401021));
#58598=CARTESIAN_POINT('Ctrl Pts',(-1.87317672244244,1.93302706793983,13.7193349366543));
#58599=CARTESIAN_POINT('Ctrl Pts',(-2.365935632993,0.568962550177037,13.8102975205886));
#58600=CARTESIAN_POINT('Ctrl Pts',(-2.37083142397042,-0.00207423906479159,
13.848589891905));
#58601=CARTESIAN_POINT('Origin',(0.,0.,-1.848589891905));
#58602=CARTESIAN_POINT('',(-2.37108122357944,-0.00209777019329237,11.651410108095));
#58603=CARTESIAN_POINT('',(-2.37507494215832,0.000954213469080735,11.848589891905));
#58604=CARTESIAN_POINT('',(-2.37175,-3.45929798001232E-13,-1.848589891905));
#58605=CARTESIAN_POINT('Ctrl Pts',(-2.37108122357943,-0.00209777019329208,
11.651410108095));
#58606=CARTESIAN_POINT('Ctrl Pts',(-2.37288020620416,-0.207721845931398,
11.6652024724495));
#58607=CARTESIAN_POINT('Ctrl Pts',(-2.25456795023167,-1.19654496148464,
11.7316650494219));
#58608=CARTESIAN_POINT('Ctrl Pts',(-0.875108611891469,-2.65846483136416,
11.8507978390121));
#58609=CARTESIAN_POINT('Ctrl Pts',(1.7485305153448,-2.18538128918389,12.0088084768656));
#58610=CARTESIAN_POINT('Ctrl Pts',(2.78568721934935,0.270549548438745,12.1668191147191));
#58611=CARTESIAN_POINT('Ctrl Pts',(1.29532508891864,2.48100448532931,12.3248297525726));
#58612=CARTESIAN_POINT('Ctrl Pts',(-1.37031563568376,2.44038632204184,12.4828403904261));
#58613=CARTESIAN_POINT('Ctrl Pts',(-2.35021221135085,0.886934755038215,
12.5917005089335));
#58614=CARTESIAN_POINT('Ctrl Pts',(-2.37537064490022,0.0531615094349561,
12.6478904148232));
#58615=CARTESIAN_POINT('Ctrl Pts',(-2.37511086845159,0.000918633378760338,
12.651410108095));
#58616=CARTESIAN_POINT('Ctrl Pts',(-2.37507494215832,0.000954213469080692,
11.848589891905));
#58617=CARTESIAN_POINT('Ctrl Pts',(-2.37133892558484,-0.72641217448684,
11.8975918484591));
#58618=CARTESIAN_POINT('Ctrl Pts',(-1.62620459990655,-2.24221827031134,
11.999264017631));
#58619=CARTESIAN_POINT('Ctrl Pts',(0.948330986936765,-2.63323367282349,
12.1536063994207));
#58620=CARTESIAN_POINT('Ctrl Pts',(2.72361280112762,-0.644348155896335,
12.3116170372742));
#58621=CARTESIAN_POINT('Ctrl Pts',(2.02769734494933,1.92916943624887,12.4696276751277));
#58622=CARTESIAN_POINT('Ctrl Pts',(-0.507995094910846,2.75230670893191,
12.6276383129812));
#58623=CARTESIAN_POINT('Ctrl Pts',(-2.16666393885777,1.41396091253342,12.753959051907));
#58624=CARTESIAN_POINT('Ctrl Pts',(-2.37004828957801,0.314833277557734,
12.8276095782149));
#58625=CARTESIAN_POINT('Ctrl Pts',(-2.36858116699997,0.00121224584437404,
12.848589891905));
#58626=CARTESIAN_POINT('Origin',(0.,0.,-1.848589891905));
#58627=CARTESIAN_POINT('',(-2.36845164206684,0.00109356539350533,10.651410108095));
#58628=CARTESIAN_POINT('',(-2.3711455013324,-0.00210217670305768,10.848589891905));
#58629=CARTESIAN_POINT('',(-2.37175,-3.45929798001232E-13,-1.848589891905));
#58630=CARTESIAN_POINT('Ctrl Pts',(-2.36845164206685,0.00109356539350527,
10.651410108095));
#58631=CARTESIAN_POINT('Ctrl Pts',(-2.36649596032256,-0.463929808682954,
10.6825145300759));
#58632=CARTESIAN_POINT('Ctrl Pts',(-2.0100003207014,-1.71916135585423,10.7662891646746));
#58633=CARTESIAN_POINT('Ctrl Pts',(0.0232810353625256,-2.79869761417686,
10.9027340118911));
#58634=CARTESIAN_POINT('Ctrl Pts',(2.35680925566857,-1.50953650986048,11.0607446497446));
#58635=CARTESIAN_POINT('Ctrl Pts',(2.5519495975734,1.1492621953461,11.2187552875981));
#58636=CARTESIAN_POINT('Ctrl Pts',(0.431646688134689,2.76530856846557,11.3767659254516));
#58637=CARTESIAN_POINT('Ctrl Pts',(-1.86103764780764,1.95027239682527,11.5209841989506));
#58638=CARTESIAN_POINT('Ctrl Pts',(-2.36601026027579,0.577514355061797,
11.6125322598317));
#58639=CARTESIAN_POINT('Ctrl Pts',(-2.37108122357943,-0.00209777019329208,
11.651410108095));
#58640=CARTESIAN_POINT('Ctrl Pts',(-2.3711455013324,-0.00210217670305756,
10.848589891905));
#58641=CARTESIAN_POINT('Ctrl Pts',(-2.37293293087196,-0.205497384262076,
10.8622336934676));
#58642=CARTESIAN_POINT('Ctrl Pts',(-2.25619484795045,-1.19205465912958,
10.928547707648));
#58643=CARTESIAN_POINT('Ctrl Pts',(-0.882549833739827,-2.656003958476,11.0475319344462));
#58644=CARTESIAN_POINT('Ctrl Pts',(1.74240395044783,-2.190269323608,11.2055425722998));
#58645=CARTESIAN_POINT('Ctrl Pts',(2.78643408629422,0.262747634075224,11.3635532101532));
#58646=CARTESIAN_POINT('Ctrl Pts',(1.3022677379473,2.47736754947181,11.5215638480067));
#58647=CARTESIAN_POINT('Ctrl Pts',(-1.36347643158376,2.44421424122154,11.6795744858602));
#58648=CARTESIAN_POINT('Ctrl Pts',(-2.34906262124821,0.891396457168339,
11.7885831671597));
#58649=CARTESIAN_POINT('Ctrl Pts',(-2.37535461804095,0.0554044099680877,
11.8449216358413));
#58650=CARTESIAN_POINT('Ctrl Pts',(-2.37507494215832,0.000954213469080692,
11.848589891905));
#58651=CARTESIAN_POINT('Origin',(0.,0.,-1.848589891905));
#58652=CARTESIAN_POINT('',(-2.37492150693046,0.00109068279076694,9.65141010809499));
#58653=CARTESIAN_POINT('',(-2.36842114142019,0.00106267303466426,9.84858989190503));
#58654=CARTESIAN_POINT('',(-2.37175,-3.45929798001232E-13,-1.848589891905));
#58655=CARTESIAN_POINT('Ctrl Pts',(-2.37492150693046,0.00109068279076715,
9.65141010809499));
#58656=CARTESIAN_POINT('Ctrl Pts',(-2.37079040527034,-0.71770812112247,
9.69982658770222));
#58657=CARTESIAN_POINT('Ctrl Pts',(-1.64110086305732,-2.22572615427059,
9.80091327992728));
#58658=CARTESIAN_POINT('Ctrl Pts',(0.919213459631522,-2.64353871880838,
9.95467018477016));
#58659=CARTESIAN_POINT('Ctrl Pts',(2.71633592014881,-0.674366006791661,
10.1126808226237));
#58660=CARTESIAN_POINT('Ctrl Pts',(2.04886359373486,1.90667467504938,10.2706914604772));
#58661=CARTESIAN_POINT('Ctrl Pts',(-0.477590346402141,2.75774505769302,
10.4287020983307));
#58662=CARTESIAN_POINT('Ctrl Pts',(-2.15868340525892,1.43166769474736,10.5556083142033));
#58663=CARTESIAN_POINT('Ctrl Pts',(-2.36980758506028,0.323510639492646,
10.629844317458));
#58664=CARTESIAN_POINT('Ctrl Pts',(-2.36845164206685,0.00109356539350527,
10.651410108095));
#58665=CARTESIAN_POINT('Ctrl Pts',(-2.36842114142019,0.00106267303466433,
9.84858989190503));
#58666=CARTESIAN_POINT('Ctrl Pts',(-2.36653124713118,-0.461754654170688,
9.87954575109394));
#58667=CARTESIAN_POINT('Ctrl Pts',(-2.01259622806101,-1.71470763772158,
9.96317182290069));
#58668=CARTESIAN_POINT('Ctrl Pts',(0.0154436428957695,-2.79875199515222,
10.0994681073253));
#58669=CARTESIAN_POINT('Ctrl Pts',(2.35257293505637,-1.51613054243843,10.2574787451788));
#58670=CARTESIAN_POINT('Ctrl Pts',(2.5551580610824,1.14211143036047,10.4154893830323));
#58671=CARTESIAN_POINT('Ctrl Pts',(0.439388822165221,2.7640891265353,10.5735000208858));
#58672=CARTESIAN_POINT('Ctrl Pts',(-1.85793312538704,1.9546434259417,10.7178668571767));
#58673=CARTESIAN_POINT('Ctrl Pts',(-2.36603277965999,0.579684720479897,
10.8095634808498));
#58674=CARTESIAN_POINT('Ctrl Pts',(-2.3711455013324,-0.00210217670305756,
10.848589891905));
#58675=CARTESIAN_POINT('Origin',(0.,0.,-1.848589891905));
#58676=CARTESIAN_POINT('',(-2.37140051282111,-0.00211329452352801,8.65141010809499));
#58677=CARTESIAN_POINT('',(-2.37488002645211,0.00112430501927618,8.84858989190502));
#58678=CARTESIAN_POINT('',(-2.37175,-3.45929798001232E-13,-1.848589891905));
#58679=CARTESIAN_POINT('Ctrl Pts',(-2.37140051282111,-0.00211329452352778,
8.65141010809499));
#58680=CARTESIAN_POINT('Ctrl Pts',(-2.37313643726488,-0.196727040066591,
8.66446843271073));
#58681=CARTESIAN_POINT('Ctrl Pts',(-2.2625332649159,-1.17436088610827,8.7301969699443));
#58682=CARTESIAN_POINT('Ctrl Pts',(-0.911807050875725,-2.64610246290276,
8.8485957197957));
#58683=CARTESIAN_POINT('Ctrl Pts',(1.7181264684868,-2.20936456486744,9.0066063576492));
#58684=CARTESIAN_POINT('Ctrl Pts',(2.78916386380546,0.231981212706065,9.16461699550269));
#58685=CARTESIAN_POINT('Ctrl Pts',(1.32952798427551,2.46284503800688,9.32262763335619));
#58686=CARTESIAN_POINT('Ctrl Pts',(-1.33641957225244,2.45911225223807,9.48063827120967));
#58687=CARTESIAN_POINT('Ctrl Pts',(-2.3444674266217,0.908984670945501,9.59023242945595));
#58688=CARTESIAN_POINT('Ctrl Pts',(-2.37528445367183,0.0642422837537755,
9.64715637508439));
#58689=CARTESIAN_POINT('Ctrl Pts',(-2.37492150693046,0.00109068279076715,
9.65141010809499));
#58690=CARTESIAN_POINT('Ctrl Pts',(-2.37488002645211,0.00112430501927616,
8.84858989190502));
#58691=CARTESIAN_POINT('Ctrl Pts',(-2.3706566377328,-0.715502201037878,
8.89685780872028));
#58692=CARTESIAN_POINT('Ctrl Pts',(-1.64485462669885,-2.22153253962258,
8.99779593815339));
#58693=CARTESIAN_POINT('Ctrl Pts',(0.911807102923268,-2.64610261394623,
9.1514042802043));
#58694=CARTESIAN_POINT('Ctrl Pts',(2.71443697103106,-0.681970062960328,
9.30941491805779));
#58695=CARTESIAN_POINT('Ctrl Pts',(2.05419501292893,1.90092979495096,9.46742555591129));
#58696=CARTESIAN_POINT('Ctrl Pts',(-0.469865879588134,2.75907181705611,
9.62543619376478));
#58697=CARTESIAN_POINT('Ctrl Pts',(-2.15663822083001,1.4361603528293,9.75249097242936));
#58698=CARTESIAN_POINT('Ctrl Pts',(-2.36974683011402,0.325711359237552,
9.82687553847611));
#58699=CARTESIAN_POINT('Ctrl Pts',(-2.36842114142019,0.00106267303466433,
9.84858989190503));
#58700=CARTESIAN_POINT('Origin',(0.,0.,-1.848589891905));
#58701=CARTESIAN_POINT('',(-2.36830911924029,0.000938119109969627,7.65141010809499));
#58702=CARTESIAN_POINT('',(-2.37146590747834,-0.00211451867861201,7.84858989190503));
#58703=CARTESIAN_POINT('',(-2.37175,-3.45929798001232E-13,-1.848589891905));
#58704=CARTESIAN_POINT('Ctrl Pts',(-2.36830911924029,0.000938119109969611,
7.65141010809499));
#58705=CARTESIAN_POINT('Ctrl Pts',(-2.36667687882826,-0.453179513046169,
7.68178049033708));
#58706=CARTESIAN_POINT('Ctrl Pts',(-2.02273688266497,-1.69714509888228,
7.764821085197));
#58707=CARTESIAN_POINT('Ctrl Pts',(-0.0154436420140344,-2.79875183539522,
7.90053189267472));
#58708=CARTESIAN_POINT('Ctrl Pts',(2.33569789249813,-1.54200055031981,8.05854253052824));
#58709=CARTESIAN_POINT('Ctrl Pts',(2.56760637965517,1.11384371496224,8.21655316838172));
#58710=CARTESIAN_POINT('Ctrl Pts',(0.469865852767273,2.75907165956415,8.37456380623522));
#58711=CARTESIAN_POINT('Ctrl Pts',(-1.84560131583056,1.97184830688283,8.51951611947298));
#58712=CARTESIAN_POINT('Ctrl Pts',(-2.36613465776925,0.588239458909152,
8.6117982200929));
#58713=CARTESIAN_POINT('Ctrl Pts',(-2.37140051282111,-0.00211329452352778,
8.65141010809499));
#58714=CARTESIAN_POINT('Ctrl Pts',(-2.37146590747834,-0.00211451867861227,
7.84858989190503));
#58715=CARTESIAN_POINT('Ctrl Pts',(-2.37318729871088,-0.194500654570986,
7.8614996537288));
#58716=CARTESIAN_POINT('Ctrl Pts',(-2.26412346336896,-1.16987191915567,
7.92707962817041));
#58717=CARTESIAN_POINT('Ctrl Pts',(-0.919213512101427,-2.64353886970564,
8.04532981522984));
#58718=CARTESIAN_POINT('Ctrl Pts',(1.71193285976134,-2.21416736498029,8.20334045308334));
#58719=CARTESIAN_POINT('Ctrl Pts',(2.78980271289629,0.224169711582251,8.36135109093682));
#58720=CARTESIAN_POINT('Ctrl Pts',(1.33641964853712,2.45911239260802,8.51936172879032));
#58721=CARTESIAN_POINT('Ctrl Pts',(-1.32952806016717,2.4628451785897,8.67737236664382));
#58722=CARTESIAN_POINT('Ctrl Pts',(-2.34328526325323,0.913448987581096,
8.78711508768204));
#58723=CARTESIAN_POINT('Ctrl Pts',(-2.37526522240956,0.0664845291139092,
8.84418759610245));
#58724=CARTESIAN_POINT('Ctrl Pts',(-2.37488002645211,0.00112430501927616,
8.84858989190502));
#58725=CARTESIAN_POINT('Origin',(0.,0.,-1.848589891905));
#58726=CARTESIAN_POINT('',(-2.37470588355431,0.00125253531034594,6.65141010809499));
#58727=CARTESIAN_POINT('',(-2.36828313834817,0.000905845531651017,6.84858989190503));
#58728=CARTESIAN_POINT('',(-2.37175,-3.45929798001232E-13,-1.848589891905));
#58729=CARTESIAN_POINT('Ctrl Pts',(-2.37470588355431,0.00125253531034581,
6.65141010809499));
#58730=CARTESIAN_POINT('Ctrl Pts',(-2.37014919057747,-0.706818549760696,
6.69909254796341));
#58731=CARTESIAN_POINT('Ctrl Pts',(-1.65954441580295,-2.20497060362383,
6.79944520044968));
#58732=CARTESIAN_POINT('Ctrl Pts',(0.882549783362729,-2.65600380686722,
6.95246806555376));
#58733=CARTESIAN_POINT('Ctrl Pts',(2.70674546316629,-0.711884358470874,
7.11047870340726));
#58734=CARTESIAN_POINT('Ctrl Pts',(2.07504800081977,1.87814433324509,7.26848934126075));
#58735=CARTESIAN_POINT('Ctrl Pts',(-0.439388797084447,2.76408896875688,
7.42649997911426));
#58736=CARTESIAN_POINT('Ctrl Pts',(-2.1484972136029,1.45386303251217,7.55414023472565));
#58737=CARTESIAN_POINT('Ctrl Pts',(-2.36950761203602,0.334379630876223,
7.62911027771924));
#58738=CARTESIAN_POINT('Ctrl Pts',(-2.36830911924029,0.000938119109969611,
7.65141010809499));
#58739=CARTESIAN_POINT('Ctrl Pts',(-2.36828313834817,0.000905845531651017,
6.84858989190503));
#58740=CARTESIAN_POINT('Ctrl Pts',(-2.36671578067491,-0.451002880761427,
6.87881171135515));
#58741=CARTESIAN_POINT('Ctrl Pts',(-2.02528764799729,-1.69268627108249,
6.96170374342309));
#58742=CARTESIAN_POINT('Ctrl Pts',(-0.0232810366912258,-2.79869777393076,
7.09726598810887));
#58743=CARTESIAN_POINT('Ctrl Pts',(2.331370743134,-1.54853533848382,7.25527662596236));
#58744=CARTESIAN_POINT('Ctrl Pts',(2.57071559891088,1.1066492425293,7.41328726381586));
#58745=CARTESIAN_POINT('Ctrl Pts',(0.477590373663518,2.75774521510932,7.57129790166936));
#58746=CARTESIAN_POINT('Ctrl Pts',(-1.84244773179659,1.9762088147049,7.71639877769907));
#58747=CARTESIAN_POINT('Ctrl Pts',(-2.36616423790973,0.590410703244725,
7.80882944111097));
#58748=CARTESIAN_POINT('Ctrl Pts',(-2.37146590747834,-0.00211451867861227,
7.84858989190503));
#58749=CARTESIAN_POINT('Origin',(0.,0.,-1.848589891905));
#58750=CARTESIAN_POINT('',(-2.37172448707781,-0.00211299049637275,5.65141010809499));
#58751=CARTESIAN_POINT('',(-2.37465944643639,0.00128394040524511,5.84858989190503));
#58752=CARTESIAN_POINT('',(-2.37175,-3.45929798001232E-13,-1.848589891905));
#58753=CARTESIAN_POINT('Ctrl Pts',(-2.37172448707781,-0.00211299049637291,
5.65141010809499));
#58754=CARTESIAN_POINT('Ctrl Pts',(-2.37338315552618,-0.185722875755726,
5.66373439297193));
#58755=CARTESIAN_POINT('Ctrl Pts',(-2.27031792652184,-1.15218371715246,
5.7287288904667));
#58756=CARTESIAN_POINT('Ctrl Pts',(-0.948330932804408,-2.6332335225146,
5.84639360057931));
#58757=CARTESIAN_POINT('Ctrl Pts',(1.68739350215265,-2.23292487806895,6.00440423843279));
#58758=CARTESIAN_POINT('Ctrl Pts',(2.79210654854793,0.193368466308401,6.1624148762863));
#58759=CARTESIAN_POINT('Ctrl Pts',(1.3634763537543,2.4442141017022,6.32042551413978));
#58760=CARTESIAN_POINT('Ctrl Pts',(-1.30226766361206,2.47736740805983,6.47843615199329));
#58761=CARTESIAN_POINT('Ctrl Pts',(-2.33856111575396,0.931047401636643,
6.58876434997835));
#58762=CARTESIAN_POINT('Ctrl Pts',(-2.37518253175268,0.0753195854131474,
6.64642233534558));
#58763=CARTESIAN_POINT('Ctrl Pts',(-2.37470588355431,0.00125253531034581,
6.65141010809499));
#58764=CARTESIAN_POINT('Ctrl Pts',(-2.37465944643639,0.00128394040524508,
5.84858989190503));
#58765=CARTESIAN_POINT('Ctrl Pts',(-2.37002572147023,-0.704617592835783,
5.89612376898149));
#58766=CARTESIAN_POINT('Ctrl Pts',(-1.66324590363498,-2.20075959342016,
5.99632785867577));
#58767=CARTESIAN_POINT('Ctrl Pts',(0.875108661844196,-2.6584649831133,6.14920216098791));
#58768=CARTESIAN_POINT('Ctrl Pts',(2.70474148699564,-0.719461413141105,
6.30721279884139));
#58769=CARTESIAN_POINT('Ctrl Pts',(2.0802994242073,1.87232623816396,6.4652234366949));
#58770=CARTESIAN_POINT('Ctrl Pts',(-0.431646712773937,2.76530872631355,
6.62323407454837));
#58771=CARTESIAN_POINT('Ctrl Pts',(-2.14641112738202,1.45835451677764,6.75102289295177));
#58772=CARTESIAN_POINT('Ctrl Pts',(-2.36944735221498,0.336578050194668,
6.82614149873732));
#58773=CARTESIAN_POINT('Ctrl Pts',(-2.36828313834817,0.000905845531651017,
6.84858989190503));
#58774=CARTESIAN_POINT('Origin',(0.,0.,-1.848589891905));
#58775=CARTESIAN_POINT('',(-2.36818920823751,0.000776286799690231,4.65141010809499));
#58776=CARTESIAN_POINT('',(-2.37179057180682,-0.00211098337720095,4.84858989190502));
#58777=CARTESIAN_POINT('',(-2.37175,-3.45929798001232E-13,-1.848589891905));
#58778=CARTESIAN_POINT('Ctrl Pts',(-2.36818920823751,0.00077628679969001,
4.65141010809499));
#58779=CARTESIAN_POINT('Ctrl Pts',(-2.36687509819612,-0.442421667272658,
4.68104645059827));
#58780=CARTESIAN_POINT('Ctrl Pts',(-2.03525109051103,-1.67510437567302,
4.76335300571939));
#58781=CARTESIAN_POINT('Ctrl Pts',(-0.054165362850041,-2.79827026138436,
4.89832977345834));
#58782=CARTESIAN_POINT('Ctrl Pts',(2.3141393814959,-1.57416938897968,5.05634041131182));
#58783=CARTESIAN_POINT('Ctrl Pts',(2.58277161716087,1.07821199946199,5.21435104916533));
#58784=CARTESIAN_POINT('Ctrl Pts',(0.50799506591352,2.75230655182614,5.37236168701881));
#58785=CARTESIAN_POINT('Ctrl Pts',(-1.82992197413507,1.99337119126977,5.51804803999537));
#58786=CARTESIAN_POINT('Ctrl Pts',(-2.36629451543789,0.598969444481106,
5.61106418035409));
#58787=CARTESIAN_POINT('Ctrl Pts',(-2.37172448707781,-0.00211299049637291,
5.65141010809499));
#58788=CARTESIAN_POINT('Ctrl Pts',(-2.37179057180682,-0.00211098337720095,
4.84858989190503));
#58789=CARTESIAN_POINT('Ctrl Pts',(-2.37343199969618,-0.183494640583722,
4.86076561399));
#58790=CARTESIAN_POINT('Ctrl Pts',(-2.27187176921823,-1.14769623702431,
4.9256115486928));
#58791=CARTESIAN_POINT('Ctrl Pts',(-0.955701215509313,-2.63056769978633,
5.04312769601343));
#58792=CARTESIAN_POINT('Ctrl Pts',(1.68113403530831,-2.23764152441791,5.20113833386694));
#58793=CARTESIAN_POINT('Ctrl Pts',(2.79263725748281,0.185548873863724,5.35914897172042));
#58794=CARTESIAN_POINT('Ctrl Pts',(1.37031571390328,2.44038646134289,5.51715960957393));
#58795=CARTESIAN_POINT('Ctrl Pts',(-1.29532516285794,2.48100462694871,5.67517024742741));
#58796=CARTESIAN_POINT('Ctrl Pts',(-2.33734608113232,0.935514281942727,
5.78564700820446));
#58797=CARTESIAN_POINT('Ctrl Pts',(-2.37516014967577,0.0775610580504524,
5.84345355636366));
#58798=CARTESIAN_POINT('Ctrl Pts',(-2.37465944643639,0.00128394040524508,
5.84858989190503));
#58799=CARTESIAN_POINT('Origin',(0.,0.,-1.848589891905));
#58800=CARTESIAN_POINT('',(-2.37446693265003,0.00140297001510288,3.65141010809499));
#58801=CARTESIAN_POINT('',(-2.36816788418401,0.000742855737058956,3.84858989190502));
#58802=CARTESIAN_POINT('',(-2.37175,-3.45929798001232E-13,-1.848589891905));
#58803=CARTESIAN_POINT('Ctrl Pts',(-2.37446693265003,0.00140297001510294,
3.65141010809499));
#58804=CARTESIAN_POINT('Ctrl Pts',(-2.36955836583972,-0.695952680709234,
3.69835850822461));
#58805=CARTESIAN_POINT('Ctrl Pts',(-1.67773013376393,-2.18413036676016,
3.79797712097207));
#58806=CARTESIAN_POINT('Ctrl Pts',(0.845717150955885,-2.66796042811686,
3.95026594633737));
#58807=CARTESIAN_POINT('Ctrl Pts',(2.69663682477438,-0.749266426116641,
4.10827658419086));
#58808=CARTESIAN_POINT('Ctrl Pts',(2.10083515905894,1.84925443784418,4.26628722204435));
#58809=CARTESIAN_POINT('Ctrl Pts',(-0.401103130814736,2.76990372055638,
4.42429785989785));
#58810=CARTESIAN_POINT('Ctrl Pts',(-2.13810821622223,1.47605202244459,4.55267215524806));
#58811=CARTESIAN_POINT('Ctrl Pts',(-2.36921055694159,0.345237284576487,
4.62837623798044));
#58812=CARTESIAN_POINT('Ctrl Pts',(-2.36818920823751,0.00077628679969001,
4.65141010809499));
#58813=CARTESIAN_POINT('Ctrl Pts',(-2.36816788418401,0.000742855737058887,
3.84858989190502));
#58814=CARTESIAN_POINT('Ctrl Pts',(-2.36691733101876,-0.440243431773009,
3.87807767161634));
#58815=CARTESIAN_POINT('Ctrl Pts',(-2.03775706613953,-1.67064082881644,
3.96023566394549));
#58816=CARTESIAN_POINT('Ctrl Pts',(-0.0620012593698648,-2.79810776790365,
4.09506386889247));
#58817=CARTESIAN_POINT('Ctrl Pts',(2.30972223178794,-1.58064368166609,4.25307450674597));
#58818=CARTESIAN_POINT('Ctrl Pts',(2.58578099692394,1.07097519687693,4.41108514459946));
#58819=CARTESIAN_POINT('Ctrl Pts',(0.515700494891298,2.75087335879294,4.56909578245295));
#58820=CARTESIAN_POINT('Ctrl Pts',(-1.8267190231715,1.99772065067605,4.71493069822147));
#58821=CARTESIAN_POINT('Ctrl Pts',(-2.36633144702867,0.6011418453507,4.80809540137217));
#58822=CARTESIAN_POINT('Ctrl Pts',(-2.37179057180682,-0.00211098337720095,
4.84858989190503));
#58823=CARTESIAN_POINT('Origin',(0.,0.,-1.848589891905));
#58824=CARTESIAN_POINT('',(-2.37205100032703,-0.00209666035588911,2.65141010809498));
#58825=CARTESIAN_POINT('',(-2.37441612858142,0.0014319253334924,2.84858989190502));
#58826=CARTESIAN_POINT('',(-2.37175,-3.45929798001232E-13,-1.848589891905));
#58827=CARTESIAN_POINT('Ctrl Pts',(-2.37205100032703,-0.00209666035588935,
2.65141010809498));
#58828=CARTESIAN_POINT('Ctrl Pts',(-2.37361961794304,-0.17470974391043,
2.66300035323312));
#58829=CARTESIAN_POINT('Ctrl Pts',(-2.27792363918998,-1.13001425292593,
2.7272608109891));
#58830=CARTESIAN_POINT('Ctrl Pts',(-0.984673254710223,-2.61986041464368,
2.8441914813629));
#58831=CARTESIAN_POINT('Ctrl Pts',(1.65633749422688,-2.25605774937986,3.0022021192164));
#58832=CARTESIAN_POINT('Ctrl Pts',(2.79451471318987,0.154718717530414,3.16021275706989));
#58833=CARTESIAN_POINT('Ctrl Pts',(1.39716369670102,2.42511523463794,3.31822339492339));
#58834=CARTESIAN_POINT('Ctrl Pts',(-1.2678664470183,2.49514829917553,3.47623403277688));
#58835=CARTESIAN_POINT('Ctrl Pts',(-2.33249179703478,0.953122680262559,
3.58729627050075));
#58836=CARTESIAN_POINT('Ctrl Pts',(-2.37506516174403,0.0863928367627885,
3.64568829560678));
#58837=CARTESIAN_POINT('Ctrl Pts',(-2.37446693265003,0.00140297001510294,
3.65141010809499));
#58838=CARTESIAN_POINT('Ctrl Pts',(-2.37441612858142,0.00143192533349229,
2.84858989190502));
#58839=CARTESIAN_POINT('Ctrl Pts',(-2.36944494516981,-0.693756276209885,
2.89538972924268));
#58840=CARTESIAN_POINT('Ctrl Pts',(-1.68137957932541,-2.17990259172208,
2.99485977919817));
#58841=CARTESIAN_POINT('Ctrl Pts',(0.838242687746051,-2.6703184178973,3.1470000417715));
#58842=CARTESIAN_POINT('Ctrl Pts',(2.69452820593443,-0.756815026848842,
3.305010679625));
#58843=CARTESIAN_POINT('Ctrl Pts',(2.10600558091548,1.8433642406156,3.46302131747849));
#58844=CARTESIAN_POINT('Ctrl Pts',(-0.393344910955346,2.77101624331114,
3.62103195533199));
#58845=CARTESIAN_POINT('Ctrl Pts',(-2.13598086517564,1.48054205574855,3.74955481347416));
#58846=CARTESIAN_POINT('Ctrl Pts',(-2.36915103263171,0.347433421218035,
3.82540745899851));
#58847=CARTESIAN_POINT('Ctrl Pts',(-2.36816788418401,0.000742855737058887,
3.84858989190502));
#58848=CARTESIAN_POINT('Origin',(0.,0.,-1.848589891905));
#58849=CARTESIAN_POINT('',(-2.36809210481233,0.000611552607929038,1.65141010809499));
#58850=CARTESIAN_POINT('',(-2.37211733643984,-0.00209141235254701,1.84858989190502));
#58851=CARTESIAN_POINT('',(-2.37175,-3.45929798001232E-13,-1.848589891905));
#58852=CARTESIAN_POINT('Ctrl Pts',(-2.36809210481233,0.000611552607929014,
1.65141010809499));
#58853=CARTESIAN_POINT('Ctrl Pts',(-2.36708900480144,-0.431654494041978,
1.68031241085947));
#58854=CARTESIAN_POINT('Ctrl Pts',(-2.04754546137161,-1.65304532360689,
1.76188492624178));
#58855=CARTESIAN_POINT('Ctrl Pts',(-0.0928761899139844,-2.79725011229448,
1.89612765424193));
#58856=CARTESIAN_POINT('Ctrl Pts',(2.29213757529781,-1.60603837127393,2.05413829209543));
#58857=CARTESIAN_POINT('Ctrl Pts',(2.59744255060163,1.04237465766208,2.21214892994892));
#58858=CARTESIAN_POINT('Ctrl Pts',(0.546026952813309,2.74501412804214,2.37015956780242));
#58859=CARTESIAN_POINT('Ctrl Pts',(-1.81399809354475,2.0148385946783,2.51657996051777));
#58860=CARTESIAN_POINT('Ctrl Pts',(-2.36649125936507,0.609705745415088,
2.61033014061529));
#58861=CARTESIAN_POINT('Ctrl Pts',(-2.37205100032703,-0.00209666035588935,
2.65141010809498));
#58862=CARTESIAN_POINT('Ctrl Pts',(-2.37211733643984,-0.00209141235254718,
1.84858989190502));
#58863=CARTESIAN_POINT('Ctrl Pts',(-2.37366633030799,-0.172479818929997,
1.8600315742512));
#58864=CARTESIAN_POINT('Ctrl Pts',(-2.27944161784295,-1.12552878575702,
1.9241434692152));
#58865=CARTESIAN_POINT('Ctrl Pts',(-0.992005816601449,-2.617092539026,2.04092557679704));
#58866=CARTESIAN_POINT('Ctrl Pts',(1.65001329883352,-2.26068751370113,2.19893621465053));
#58867=CARTESIAN_POINT('Ctrl Pts',(2.79493721635935,0.146892622206337,2.35694685250402));
#58868=CARTESIAN_POINT('Ctrl Pts',(1.40394942456389,2.42119328420925,2.51495749035753));
#58869=CARTESIAN_POINT('Ctrl Pts',(-1.26087427680964,2.49868913935238,2.67296812821101));
#58870=CARTESIAN_POINT('Ctrl Pts',(-2.33124358910813,0.957592063764426,
2.78417892872685));
#58871=CARTESIAN_POINT('Ctrl Pts',(-2.3750396929755,0.0886334171669318,
2.84271951662485));
#58872=CARTESIAN_POINT('Ctrl Pts',(-2.37441612858142,0.00143192533349229,
2.84858989190502));
#58873=CARTESIAN_POINT('Origin',(0.,0.,-1.848589891905));
#58874=CARTESIAN_POINT('',(-2.37417832678934,0.00170073231846648,0.651410108094986));
#58875=CARTESIAN_POINT('',(-2.36807033412218,0.000590439285148986,0.848589891905023));
#58876=CARTESIAN_POINT('',(-2.37175,-3.45929798001232E-13,-1.848589891905));
#58877=CARTESIAN_POINT('Ctrl Pts',(-2.37417832678934,0.00170073231846661,
0.651410108094986));
#58878=CARTESIAN_POINT('Ctrl Pts',(-2.36898203260896,-0.684918424266715,
0.697624468485814));
#58879=CARTESIAN_POINT('Ctrl Pts',(-1.69570475500353,-2.16345817758698,
0.796509041494473));
#58880=CARTESIAN_POINT('Ctrl Pts',(0.80874805201177,-2.67926694285025,0.948063827120964));
#58881=CARTESIAN_POINT('Ctrl Pts',(2.68599862008771,-0.786578017594937,
1.10607446497446));
#58882=CARTESIAN_POINT('Ctrl Pts',(2.12622710642163,1.82004872489232,1.26408510282796));
#58883=CARTESIAN_POINT('Ctrl Pts',(-0.362744329120993,2.775168194831,1.42209574068145));
#58884=CARTESIAN_POINT('Ctrl Pts',(-2.12751372443616,1.49823817530827,1.55120407577046));
#58885=CARTESIAN_POINT('Ctrl Pts',(-2.36891700761771,0.356087049254629,
1.62764219824164));
#58886=CARTESIAN_POINT('Ctrl Pts',(-2.36809210481233,0.000611552607929014,
1.65141010809499));
#58887=CARTESIAN_POINT('Ctrl Pts',(-2.36807033412218,0.000590439285148986,
0.848589891905023));
#58888=CARTESIAN_POINT('Ctrl Pts',(-2.36713171325374,-0.429468009012812,
0.87734363187754));
#58889=CARTESIAN_POINT('Ctrl Pts',(-2.05001637623951,-1.64860125877915,
0.958767584467889));
#58890=CARTESIAN_POINT('Ctrl Pts',(-0.1007027086929,-2.79696300482839,1.09286174967607));
#58891=CARTESIAN_POINT('Ctrl Pts',(2.28762793115499,-1.61245941657473,1.25087238752956));
#58892=CARTESIAN_POINT('Ctrl Pts',(2.6003532631254,1.03510135356512,1.40888302538306));
#58893=CARTESIAN_POINT('Ctrl Pts',(0.553710899450507,2.74347213477777,1.56689366323655));
#58894=CARTESIAN_POINT('Ctrl Pts',(-1.81074509731807,2.0191774297212,1.71346261874387));
#58895=CARTESIAN_POINT('Ctrl Pts',(-2.36653574986442,0.611879799745258,
1.80736136163337));
#58896=CARTESIAN_POINT('Ctrl Pts',(-2.37211733643984,-0.00209141235254718,
1.84858989190502));
#58897=CARTESIAN_POINT('Origin',(-0.866025403784439,-1.5,0.));
#58898=CARTESIAN_POINT('',(-0.866025403784439,-1.5,0.));
#58899=CARTESIAN_POINT('',(0.866025403784439,-1.5,0.));
#58900=CARTESIAN_POINT('',(-0.43301270189222,-1.5,0.));
#58901=CARTESIAN_POINT('',(-0.866025403784439,-1.5,3.));
#58902=CARTESIAN_POINT('',(-0.866025403784439,-1.5,0.));
#58903=CARTESIAN_POINT('',(0.866025403784439,-1.5,3.));
#58904=CARTESIAN_POINT('',(-0.866025403784439,-1.5,3.));
#58905=CARTESIAN_POINT('',(0.866025403784439,-1.5,0.));
#58906=CARTESIAN_POINT('Origin',(-1.73205080756888,2.12115047744981E-16,
0.));
#58907=CARTESIAN_POINT('',(-1.73205080756888,2.12115047744981E-16,0.));
#58908=CARTESIAN_POINT('',(-1.51554445662277,-0.375,0.));
#58909=CARTESIAN_POINT('',(-1.73205080756888,2.77555756156289E-16,3.));
#58910=CARTESIAN_POINT('',(-1.73205080756888,2.12115047744981E-16,0.));
#58911=CARTESIAN_POINT('',(-1.73205080756888,2.12115047744981E-16,3.));
#58912=CARTESIAN_POINT('Origin',(-0.866025403784438,1.5,0.));
#58913=CARTESIAN_POINT('',(-0.866025403784438,1.5,0.));
#58914=CARTESIAN_POINT('',(-1.08253175473055,1.125,0.));
#58915=CARTESIAN_POINT('',(-0.866025403784438,1.5,3.));
#58916=CARTESIAN_POINT('',(-0.866025403784438,1.5,0.));
#58917=CARTESIAN_POINT('',(-0.866025403784438,1.5,3.));
#58918=CARTESIAN_POINT('Origin',(0.866025403784439,1.5,0.));
#58919=CARTESIAN_POINT('',(0.866025403784439,1.5,0.));
#58920=CARTESIAN_POINT('',(0.43301270189222,1.5,0.));
#58921=CARTESIAN_POINT('',(0.866025403784439,1.5,3.));
#58922=CARTESIAN_POINT('',(0.866025403784439,1.5,0.));
#58923=CARTESIAN_POINT('',(0.866025403784439,1.5,3.));
#58924=CARTESIAN_POINT('Origin',(1.73205080756888,0.,0.));
#58925=CARTESIAN_POINT('',(1.73205080756888,0.,0.));
#58926=CARTESIAN_POINT('',(1.51554445662277,0.375,0.));
#58927=CARTESIAN_POINT('',(1.73205080756888,0.,3.));
#58928=CARTESIAN_POINT('',(1.73205080756888,0.,0.));
#58929=CARTESIAN_POINT('',(1.73205080756888,0.,3.));
#58930=CARTESIAN_POINT('Origin',(0.866025403784439,-1.5,0.));
#58931=CARTESIAN_POINT('',(1.08253175473055,-1.125,0.));
#58932=CARTESIAN_POINT('',(0.866025403784439,-1.5,3.));
#58933=CARTESIAN_POINT('Origin',(0.,2.77555756156289E-16,3.));
#58934=CARTESIAN_POINT('Ctrl Pts',(-1.03908919352512,2.13201587949042,-0.329233991005384));
#58935=CARTESIAN_POINT('Ctrl Pts',(-1.74465150592227,1.78814312449682,-0.276563778387552));
#58936=CARTESIAN_POINT('Ctrl Pts',(-2.77586045906315,0.351246257520133,
-0.171223353151889));
#58937=CARTESIAN_POINT('Ctrl Pts',(-1.80897499257101,-2.13797378108051,
-0.0132127152983944));
#58938=CARTESIAN_POINT('Ctrl Pts',(0.801552232242426,-2.68072923420017,
0.1447979225551));
#58939=CARTESIAN_POINT('Ctrl Pts',(2.68362344803569,-0.794509576969642,
0.302808560408595));
#58940=CARTESIAN_POINT('Ctrl Pts',(2.13140048014165,1.81430348231616,0.46081919826209));
#58941=CARTESIAN_POINT('Ctrl Pts',(-0.355015924163216,2.7760602537354,0.618829836115584));
#58942=CARTESIAN_POINT('Ctrl Pts',(-2.51914843674926,1.2195020760201,0.77684047396908));
#58943=CARTESIAN_POINT('Ctrl Pts',(-2.39768778263246,-1.44378427629767,
0.934851111822574));
#58944=CARTESIAN_POINT('Ctrl Pts',(-0.1007027086929,-2.79696300482839,1.09286174967607));
#58945=CARTESIAN_POINT('Ctrl Pts',(2.28762793115499,-1.61245941657473,1.25087238752956));
#58946=CARTESIAN_POINT('Ctrl Pts',(2.6003532631254,1.03510135356512,1.40888302538306));
#58947=CARTESIAN_POINT('Ctrl Pts',(0.553710899450507,2.74347213477777,1.56689366323655));
#58948=CARTESIAN_POINT('Ctrl Pts',(-1.99532275459133,1.96263646638017,1.72490430109005));
#58949=CARTESIAN_POINT('Ctrl Pts',(-2.73395547277665,-0.598949991906553,
1.88291493894354));
#58950=CARTESIAN_POINT('Ctrl Pts',(-0.992005816601449,-2.617092539026,2.04092557679704));
#58951=CARTESIAN_POINT('Ctrl Pts',(1.65001329883352,-2.26068751370113,2.19893621465053));
#58952=CARTESIAN_POINT('Ctrl Pts',(2.79493721635935,0.146892622206337,2.35694685250402));
#58953=CARTESIAN_POINT('Ctrl Pts',(1.40394942456389,2.42119328420925,2.51495749035753));
#58954=CARTESIAN_POINT('Ctrl Pts',(-1.26087427680964,2.49868913935238,2.67296812821101));
#58955=CARTESIAN_POINT('Ctrl Pts',(-2.78167744512252,0.309066092145391,
2.83097876606452));
#58956=CARTESIAN_POINT('Ctrl Pts',(-1.77859992075117,-2.16097975765903,
2.988989403918));
#58957=CARTESIAN_POINT('Ctrl Pts',(0.838242687746051,-2.6703184178973,3.1470000417715));
#58958=CARTESIAN_POINT('Ctrl Pts',(2.69452820593443,-0.756815026848842,
3.305010679625));
#58959=CARTESIAN_POINT('Ctrl Pts',(2.10600558091548,1.8433642406156,3.46302131747849));
#58960=CARTESIAN_POINT('Ctrl Pts',(-0.393344910955346,2.77101624331114,
3.62103195533199));
#58961=CARTESIAN_POINT('Ctrl Pts',(-2.53580441312556,1.18446072736811,3.77904259318548));
#58962=CARTESIAN_POINT('Ctrl Pts',(-2.37746956507925,-1.47678356668067,
3.93705323103898));
#58963=CARTESIAN_POINT('Ctrl Pts',(-0.0620012593698648,-2.79810776790365,
4.09506386889247));
#58964=CARTESIAN_POINT('Ctrl Pts',(2.30972223178794,-1.58064368166609,4.25307450674597));
#58965=CARTESIAN_POINT('Ctrl Pts',(2.58578099692394,1.07097519687693,4.41108514459946));
#58966=CARTESIAN_POINT('Ctrl Pts',(0.515700494891298,2.75087335879294,4.56909578245295));
#58967=CARTESIAN_POINT('Ctrl Pts',(-2.0222870660373,1.93484011199812,4.72710642030645));
#58968=CARTESIAN_POINT('Ctrl Pts',(-2.72540651522529,-0.63671859029782,
4.88511705815995));
#58969=CARTESIAN_POINT('Ctrl Pts',(-0.955701215509313,-2.63056769978633,
5.04312769601343));
#58970=CARTESIAN_POINT('Ctrl Pts',(1.68113403530831,-2.23764152441791,5.20113833386694));
#58971=CARTESIAN_POINT('Ctrl Pts',(2.79263725748281,0.185548873863724,5.35914897172042));
#58972=CARTESIAN_POINT('Ctrl Pts',(1.37031571390328,2.44038646134289,5.51715960957393));
#58973=CARTESIAN_POINT('Ctrl Pts',(-1.29532516285794,2.48100462694871,5.67517024742741));
#58974=CARTESIAN_POINT('Ctrl Pts',(-2.78568737836061,0.27054956388192,5.83318088528093));
#58975=CARTESIAN_POINT('Ctrl Pts',(-1.74853061515341,-2.18538141392889,
5.99119152313439));
#58976=CARTESIAN_POINT('Ctrl Pts',(0.875108661844196,-2.6584649831133,6.14920216098791));
#58977=CARTESIAN_POINT('Ctrl Pts',(2.70474148699564,-0.719461413141105,
6.30721279884139));
#58978=CARTESIAN_POINT('Ctrl Pts',(2.0802994242073,1.87232623816396,6.4652234366949));
#58979=CARTESIAN_POINT('Ctrl Pts',(-0.431646712773937,2.76530872631355,
6.62323407454837));
#58980=CARTESIAN_POINT('Ctrl Pts',(-2.55194974324264,1.14926226094754,6.78124471240189));
#58981=CARTESIAN_POINT('Ctrl Pts',(-2.3568093901987,-1.50953659602729,6.93925535025537));
#58982=CARTESIAN_POINT('Ctrl Pts',(-0.0232810366912258,-2.79869777393076,
7.09726598810887));
#58983=CARTESIAN_POINT('Ctrl Pts',(2.331370743134,-1.54853533848382,7.25527662596236));
#58984=CARTESIAN_POINT('Ctrl Pts',(2.57071559891088,1.1066492425293,7.41328726381586));
#58985=CARTESIAN_POINT('Ctrl Pts',(0.477590373663518,2.75774521510932,7.57129790166936));
#58986=CARTESIAN_POINT('Ctrl Pts',(-2.04886371068724,1.90667478388511,7.72930853952283));
#58987=CARTESIAN_POINT('Ctrl Pts',(-2.71633607520133,-0.674366045285695,
7.88731917737635));
#58988=CARTESIAN_POINT('Ctrl Pts',(-0.919213512101427,-2.64353886970564,
8.04532981522984));
#58989=CARTESIAN_POINT('Ctrl Pts',(1.71193285976134,-2.21416736498029,8.20334045308334));
#58990=CARTESIAN_POINT('Ctrl Pts',(2.78980271289629,0.224169711582251,8.36135109093682));
#58991=CARTESIAN_POINT('Ctrl Pts',(1.33641964853712,2.45911239260802,8.51936172879032));
#58992=CARTESIAN_POINT('Ctrl Pts',(-1.32952806016717,2.4628451785897,8.67737236664382));
#58993=CARTESIAN_POINT('Ctrl Pts',(-2.78916402301518,0.231981225947694,
8.8353830044973));
#58994=CARTESIAN_POINT('Ctrl Pts',(-1.71812656655989,-2.20936469098144,
8.99339364235082));
#58995=CARTESIAN_POINT('Ctrl Pts',(0.911807102923268,-2.64610261394623,
9.1514042802043));
#58996=CARTESIAN_POINT('Ctrl Pts',(2.71443697103106,-0.681970062960328,
9.30941491805779));
#58997=CARTESIAN_POINT('Ctrl Pts',(2.05419501292893,1.90092979495096,9.46742555591129));
#58998=CARTESIAN_POINT('Ctrl Pts',(-0.469865879588134,2.75907181705611,
9.62543619376478));
#58999=CARTESIAN_POINT('Ctrl Pts',(-2.5676065262181,1.11384377854193,9.78344683161828));
#59000=CARTESIAN_POINT('Ctrl Pts',(-2.3356980258232,-1.54200063833969,9.94145746947177));
#59001=CARTESIAN_POINT('Ctrl Pts',(0.0154436428957695,-2.79875199515222,
10.0994681073253));
#59002=CARTESIAN_POINT('Ctrl Pts',(2.35257293505637,-1.51613054243843,10.2574787451788));
#59003=CARTESIAN_POINT('Ctrl Pts',(2.5551580610824,1.14211143036047,10.4154893830323));
#59004=CARTESIAN_POINT('Ctrl Pts',(0.439388822165221,2.7640891265353,10.5735000208858));
#59005=CARTESIAN_POINT('Ctrl Pts',(-2.07504811926679,1.87814444045227,10.7315106587392));
#59006=CARTESIAN_POINT('Ctrl Pts',(-2.70674561767137,-0.711884399106498,
10.8895212965927));
#59007=CARTESIAN_POINT('Ctrl Pts',(-0.882549833739827,-2.656003958476,11.0475319344462));
#59008=CARTESIAN_POINT('Ctrl Pts',(1.74240395044783,-2.190269323608,11.2055425722998));
#59009=CARTESIAN_POINT('Ctrl Pts',(2.78643408629422,0.262747634075224,11.3635532101532));
#59010=CARTESIAN_POINT('Ctrl Pts',(1.3022677379473,2.47736754947181,11.5215638480067));
#59011=CARTESIAN_POINT('Ctrl Pts',(-1.36347643158376,2.44421424122154,11.6795744858602));
#59012=CARTESIAN_POINT('Ctrl Pts',(-2.79210670792561,0.193368477345981,
11.8375851237137));
#59013=CARTESIAN_POINT('Ctrl Pts',(-1.68739359847148,-2.2329250055278,11.9955957615672));
#59014=CARTESIAN_POINT('Ctrl Pts',(0.948330986936765,-2.63323367282349,
12.1536063994207));
#59015=CARTESIAN_POINT('Ctrl Pts',(2.72361280112762,-0.644348155896335,
12.3116170372742));
#59016=CARTESIAN_POINT('Ctrl Pts',(2.02769734494933,1.92916943624887,12.4696276751277));
#59017=CARTESIAN_POINT('Ctrl Pts',(-0.507995094910846,2.75230670893191,
12.6276383129812));
#59018=CARTESIAN_POINT('Ctrl Pts',(-2.58277176458946,1.0782120610078,12.7856489508347));
#59019=CARTESIAN_POINT('Ctrl Pts',(-2.31413951359037,-1.57416947883587,
12.9436595886882));
#59020=CARTESIAN_POINT('Ctrl Pts',(0.0541653659420804,-2.79827042111378,
13.1016702265417));
#59021=CARTESIAN_POINT('Ctrl Pts',(2.37332474856975,-1.48343549715007,13.2596808643952));
#59022=CARTESIAN_POINT('Ctrl Pts',(2.53911136180312,1.17735497143754,13.4176915022487));
#59023=CARTESIAN_POINT('Ctrl Pts',(0.401103153710141,2.76990387866618,13.5757021401021));
#59024=CARTESIAN_POINT('Ctrl Pts',(-2.10083527897802,1.84925454340324,13.7337127779557));
#59025=CARTESIAN_POINT('Ctrl Pts',(-2.6966369787023,-0.749266468887916,
13.8917234158091));
#59026=CARTESIAN_POINT('Ctrl Pts',(-0.845717199230744,-2.66796058040481,
14.0497340536626));
#59027=CARTESIAN_POINT('Ctrl Pts',(1.77254147373567,-2.16595197414774,14.2077446915161));
#59028=CARTESIAN_POINT('Ctrl Pts',(2.78253202299393,0.301275253636565,14.3657553293696));
#59029=CARTESIAN_POINT('Ctrl Pts',(1.26786651939106,2.49514844158187,14.5237659672231));
#59030=CARTESIAN_POINT('Ctrl Pts',(-1.3971637764554,2.42511537310475,14.6817766050766));
#59031=CARTESIAN_POINT('Ctrl Pts',(-2.79451487270181,0.154718726293029,
14.8397872429301));
#59032=CARTESIAN_POINT('Ctrl Pts',(-1.65633758877797,-2.25605787803393,
14.9977978807836));
#59033=CARTESIAN_POINT('Ctrl Pts',(0.984673310924482,-2.61986056441679,
15.1558085186371));
#59034=CARTESIAN_POINT('Ctrl Pts',(2.73226724128555,-0.606603006955222,
15.3138191564906));
#59035=CARTESIAN_POINT('Ctrl Pts',(2.0008114535995,1.95703997099618,15.4718297943441));
#59036=CARTESIAN_POINT('Ctrl Pts',(-0.546026983988871,2.74501428607443,
15.6298404321976));
#59037=CARTESIAN_POINT('Ctrl Pts',(-2.59744269888199,1.04237471475225,15.7878510700511));
#59038=CARTESIAN_POINT('Ctrl Pts',(-2.29213770605498,-1.60603845864169,
15.9458617079046));
#59039=CARTESIAN_POINT('Ctrl Pts',(0.0928761949570627,-2.79725027962867,
16.1038723457581));
#59040=CARTESIAN_POINT('Ctrl Pts',(2.39362321294746,-1.45046193319176,16.2618829836116));
#59041=CARTESIAN_POINT('Ctrl Pts',(2.52257665905884,1.21238356994498,16.4198936214651));
#59042=CARTESIAN_POINT('Ctrl Pts',(0.362744353785385,2.77516839483905,16.5779042593186));
#59043=CARTESIAN_POINT('Ctrl Pts',(-2.12622723672383,1.82004875684226,16.735914897172));
#59044=CARTESIAN_POINT('Ctrl Pts',(-2.68599875372316,-0.786577939425693,
16.8939255350255));
#59045=CARTESIAN_POINT('Ctrl Pts',(-0.80874814078054,-2.6792673034923,17.051936172879));
#59046=CARTESIAN_POINT('Ctrl Pts',(1.80238833174315,-2.14148580062739,17.2099468107325));
#59047=CARTESIAN_POINT('Ctrl Pts',(2.77800430721521,0.340253358304015,17.367957448586));
#59048=CARTESIAN_POINT('Ctrl Pts',(1.23340008456365,2.51147754111133,17.5259680864395));
#59049=CARTESIAN_POINT('Ctrl Pts',(-1.43092211742628,2.4074435208734,17.683978724293));
#59050=CARTESIAN_POINT('Ctrl Pts',(-2.7957460534832,0.112157148881699,17.8419893621465));
#59051=CARTESIAN_POINT('Ctrl Pts',(-2.01608411688922,-1.47535404036764,
17.9473297873822));
#59052=CARTESIAN_POINT('Ctrl Pts',(-1.37702479013086,-1.93106208855776,
18.));
#59053=CARTESIAN_POINT('Ctrl Pts',(-1.12236674703449,2.30288577939267,-0.219489327336923));
#59054=CARTESIAN_POINT('Ctrl Pts',(-1.88447618126776,1.93145342515308,-0.166819114719091));
#59055=CARTESIAN_POINT('Ctrl Pts',(-2.99833112794769,0.379396804352793,
-0.061478689483428));
#59056=CARTESIAN_POINT('Ctrl Pts',(-1.95395485828392,-2.30932117557277,
0.096531948370067));
#59057=CARTESIAN_POINT('Ctrl Pts',(0.865792443118504,-2.89557563394757,
0.254542586223561));
#59058=CARTESIAN_POINT('Ctrl Pts',(2.89870180385485,-0.858185355932735,
0.412553224077057));
#59059=CARTESIAN_POINT('Ctrl Pts',(2.30222105901111,1.95971039855811,0.570563861930551));
#59060=CARTESIAN_POINT('Ctrl Pts',(-0.383468590022299,2.9985469351159,0.728574499784046));
#59061=CARTESIAN_POINT('Ctrl Pts',(-2.72104498234585,1.31723877660696,0.88658513763754));
#59062=CARTESIAN_POINT('Ctrl Pts',(-2.58984989331673,-1.55949601988483,
1.04459577549104));
#59063=CARTESIAN_POINT('Ctrl Pts',(-0.108773503061664,-3.02112493216803,
1.20260641334453));
#59064=CARTESIAN_POINT('Ctrl Pts',(2.47096932151246,-1.74168958871231,1.36061705119803));
#59065=CARTESIAN_POINT('Ctrl Pts',(2.80875795000181,1.11805930259998,1.51862768905152));
#59066=CARTESIAN_POINT('Ctrl Pts',(0.598087926317007,2.963347049202,1.67663832690502));
#59067=CARTESIAN_POINT('Ctrl Pts',(-2.15523741687382,2.11993149395523,1.83464896475851));
#59068=CARTESIAN_POINT('Ctrl Pts',(-2.95306767661361,-0.646952694957672,
1.992659602612));
#59069=CARTESIAN_POINT('Ctrl Pts',(-1.07150988419109,-2.82683879114357,
2.1506702404655));
#59070=CARTESIAN_POINT('Ctrl Pts',(1.7822532178328,-2.4418697707811,2.30868087831899));
#59071=CARTESIAN_POINT('Ctrl Pts',(3.01893678736936,0.158665296084686,2.46669151617249));
#59072=CARTESIAN_POINT('Ctrl Pts',(1.51646861353936,2.61523923766418,2.62470215402598));
#59073=CARTESIAN_POINT('Ctrl Pts',(-1.36192674247852,2.69894597947969,2.78271279187948));
#59074=CARTESIAN_POINT('Ctrl Pts',(-3.00461431495578,0.333836119768613,
2.94072342973297));
#59075=CARTESIAN_POINT('Ctrl Pts',(-1.92114538363842,-2.33417096061113,
3.09873406758647));
#59076=CARTESIAN_POINT('Ctrl Pts',(0.905423446354246,-2.88433044527596,
3.25674470543996));
#59077=CARTESIAN_POINT('Ctrl Pts',(2.91048052095275,-0.817469785158218,
3.41475534329346));
#59078=CARTESIAN_POINT('Ctrl Pts',(2.27479089169405,1.99110022434223,3.57276598114695));
#59079=CARTESIAN_POINT('Ctrl Pts',(-0.424869444242589,2.99309867368931,
3.73077661900045));
#59080=CARTESIAN_POINT('Ctrl Pts',(-2.73903584794299,1.27938904749487,3.88878725685394));
#59081=CARTESIAN_POINT('Ctrl Pts',(-2.56801129158029,-1.5951400304591,4.04679789470744));
#59082=CARTESIAN_POINT('Ctrl Pts',(-0.066970335390515,-3.02236144200463,
4.20480853256093));
#59083=CARTESIAN_POINT('Ctrl Pts',(2.49483436455587,-1.70732398938125,4.36281917041442));
#59084=CARTESIAN_POINT('Ctrl Pts',(2.79301779303032,1.15680824645619,4.52082980826793));
#59085=CARTESIAN_POINT('Ctrl Pts',(0.557031187026083,2.97134144253583,4.67884044612141));
#59086=CARTESIAN_POINT('Ctrl Pts',(-2.1843627765756,2.08990740743638,4.83685108397491));
#59087=CARTESIAN_POINT('Ctrl Pts',(-2.94383356491536,-0.68774824858349,
4.9948617218284));
#59088=CARTESIAN_POINT('Ctrl Pts',(-1.03229565957585,-2.84139391542219,
5.15287235968191));
#59089=CARTESIAN_POINT('Ctrl Pts',(1.81586811824769,-2.41697676622944,5.31088299753539));
#59090=CARTESIAN_POINT('Ctrl Pts',(3.0164524988418,0.200419643734152,5.46889363538889));
#59091=CARTESIAN_POINT('Ctrl Pts',(1.48013933722692,2.63597064736315,5.62690427324239));
#59092=CARTESIAN_POINT('Ctrl Pts',(-1.39913868650357,2.67984414608263,5.78491491109587));
#59093=CARTESIAN_POINT('Ctrl Pts',(-3.00894562332883,0.292232693610869,
5.94292554894938));
#59094=CARTESIAN_POINT('Ctrl Pts',(-1.88866618077534,-2.36052828175403,
6.10093618680286));
#59095=CARTESIAN_POINT('Ctrl Pts',(0.945244035080052,-2.87152701981199,
6.25894682465637));
#59096=CARTESIAN_POINT('Ctrl Pts',(2.92151234296826,-0.777122475063588,
6.41695746250985));
#59097=CARTESIAN_POINT('Ctrl Pts',(2.24702452123894,2.02238337421861,6.57496810036335));
#59098=CARTESIAN_POINT('Ctrl Pts',(-0.466240934756171,2.98693372911462,
6.73297873821685));
#59099=CARTESIAN_POINT('Ctrl Pts',(-2.75647514165928,1.2413696084484,6.89098937607034));
#59100=CARTESIAN_POINT('Ctrl Pts',(-2.54569531195281,-1.63051804346545,
7.04900001392383));
#59101=CARTESIAN_POINT('Ctrl Pts',(-0.0251468897776794,-3.02299873392289,
7.20701065177733));
#59102=CARTESIAN_POINT('Ctrl Pts',(2.51821789063718,-1.67264233075684,7.36502128963082));
#59103=CARTESIAN_POINT('Ctrl Pts',(2.77674498231681,1.19534137991761,7.52303192748432));
#59104=CARTESIAN_POINT('Ctrl Pts',(0.515866739298153,2.97876404212398,7.68104256533782));
#59105=CARTESIAN_POINT('Ctrl Pts',(-2.2130694000192,2.05948477587565,7.8390532031913));
#59106=CARTESIAN_POINT('Ctrl Pts',(-2.93403617665716,-0.728412949796985,
7.99706384104482));
#59107=CARTESIAN_POINT('Ctrl Pts',(-0.992883657953795,-2.85540465663506,
8.15507447889828));
#59108=CARTESIAN_POINT('Ctrl Pts',(1.84913530707925,-2.39162127592933,8.31308511675181));
#59109=CARTESIAN_POINT('Ctrl Pts',(3.01339078036112,0.242135739203144,8.47109575460528));
#59110=CARTESIAN_POINT('Ctrl Pts',(1.44352667985415,2.65619736388585,8.62910639245879));
#59111=CARTESIAN_POINT('Ctrl Pts',(-1.43608276679169,2.66022931310232,8.78711703031227));
#59112=CARTESIAN_POINT('Ctrl Pts',(-3.01270090283309,0.250573305508763,
8.94512766816578));
#59113=CARTESIAN_POINT('Ctrl Pts',(-1.8558254070196,-2.38643369277787,9.10313830601926));
#59114=CARTESIAN_POINT('Ctrl Pts',(0.984883663893263,-2.85817387154125,
9.26114894387277));
#59115=CARTESIAN_POINT('Ctrl Pts',(2.93198486923989,-0.736626389639412,
9.41915958172626));
#59116=CARTESIAN_POINT('Ctrl Pts',(2.21882797819689,2.05327935618502,9.57717021957975));
#59117=CARTESIAN_POINT('Ctrl Pts',(-0.507523167502811,2.98019696426475,
9.73518085743326));
#59118=CARTESIAN_POINT('Ctrl Pts',(-2.77338673374079,1.20311252028871,9.89319149528673));
#59119=CARTESIAN_POINT('Ctrl Pts',(-2.52289198235681,-1.66558390864122,
10.0512021331402));
#59120=CARTESIAN_POINT('Ctrl Pts',(0.0166813699413495,-3.0230573006911,
10.2092127709937));
#59121=CARTESIAN_POINT('Ctrl Pts',(2.54111932713196,-1.63764046012589,10.3672234088472));
#59122=CARTESIAN_POINT('Ctrl Pts',(2.75994058936072,1.23364567626368,10.5252340467007));
#59123=CARTESIAN_POINT('Ctrl Pts',(0.474603533642675,2.98561638480545,10.6832446845542));
#59124=CARTESIAN_POINT('Ctrl Pts',(-2.24135235172689,2.02866787493005,10.8412553224077));
#59125=CARTESIAN_POINT('Ctrl Pts',(-2.92367709421501,-0.768938203061419,
10.9992659602612));
#59126=CARTESIAN_POINT('Ctrl Pts',(-0.953281577907687,-2.86886875694702,
11.1572765981147));
#59127=CARTESIAN_POINT('Ctrl Pts',(1.88204849600037,-2.36580793177884,11.3152872359682));
#59128=CARTESIAN_POINT('Ctrl Pts',(3.00975217599019,0.283805480016149,11.4732978738217));
#59129=CARTESIAN_POINT('Ctrl Pts',(1.4066376726038,2.67591557590604,11.6313085116752));
#59130=CARTESIAN_POINT('Ctrl Pts',(-1.47275192227073,2.64010520373961,11.7893191495287));
#59131=CARTESIAN_POINT('Ctrl Pts',(-3.01587942851794,0.208865947456909,
11.9473297873822));
#59132=CARTESIAN_POINT('Ctrl Pts',(-1.82262935259517,-2.41188224306718,
12.1053404252356));
#59133=CARTESIAN_POINT('Ctrl Pts',(1.02433474580686,-2.84427355222726,12.2633510630892));
#59134=CARTESIAN_POINT('Ctrl Pts',(2.94189609403271,-0.695989283882013,
12.4213617009427));
#59135=CARTESIAN_POINT('Ctrl Pts',(2.19020666098988,2.08378225674299,12.5793723387962));
#59136=CARTESIAN_POINT('Ctrl Pts',(-0.548708239617311,2.97288966817698,
12.7373829766496));
#59137=CARTESIAN_POINT('Ctrl Pts',(-2.78976738649411,1.16462510732239,12.8953936145031));
#59138=CARTESIAN_POINT('Ctrl Pts',(-2.499605668346,-1.70033091312222,13.0534042523566));
#59139=CARTESIAN_POINT('Ctrl Pts',(0.0585064361684609,-3.02253713101717,
13.2114148902101));
#59140=CARTESIAN_POINT('Ctrl Pts',(2.56353428974845,-1.60232507829621,13.3694255280636));
#59141=CARTESIAN_POINT('Ctrl Pts',(2.74260783122701,1.27171380246415,13.5274361659171));
#59142=CARTESIAN_POINT('Ctrl Pts',(0.433249469497138,2.99189715884739,13.6854468037706));
#59143=CARTESIAN_POINT('Ctrl Pts',(-2.26920621715125,1.99746260403018,13.8434574416241));
#59144=CARTESIAN_POINT('Ctrl Pts',(-2.91275830080694,-0.809316249834913,
14.0014680794776));
#59145=CARTESIAN_POINT('Ctrl Pts',(-0.913497000764287,-2.88178363946469,
14.1594787173311));
#59146=CARTESIAN_POINT('Ctrl Pts',(1.9146013838439,-2.33954167419453,14.3174893551846));
#59147=CARTESIAN_POINT('Ctrl Pts',(3.00553738276517,0.325420886381165,14.4754999930381));
#59148=CARTESIAN_POINT('Ctrl Pts',(1.36947937666002,2.69512151333788,14.6335106308916));
#59149=CARTESIAN_POINT('Ctrl Pts',(-1.50913913129515,2.61947566143097,14.7915212687451));
#59150=CARTESIAN_POINT('Ctrl Pts',(-3.01848059508095,0.16711862140126,14.9495319065986));
#59151=CARTESIAN_POINT('Ctrl Pts',(-1.78908436647388,-2.43686909407676,
15.1075425444521));
#59152=CARTESIAN_POINT('Ctrl Pts',(1.06358971661008,-2.8298286592636,15.2655531823056));
#59153=CARTESIAN_POINT('Ctrl Pts',(2.95124414221567,-0.655219059056894,
15.423563820159));
#59154=CARTESIAN_POINT('Ctrl Pts',(2.16116600634399,2.11388646879463,15.5815744580126));
#59155=CARTESIAN_POINT('Ctrl Pts',(-0.589788185298654,2.96501279584345,
15.739585095866));
#59156=CARTESIAN_POINT('Ctrl Pts',(-2.80561411928709,1.12591558557024,15.8975957337196));
#59157=CARTESIAN_POINT('Ctrl Pts',(-2.47584053123723,-1.73475402464994,
16.055606371573));
#59158=CARTESIAN_POINT('Ctrl Pts',(0.100319735264717,-3.0214352305381,16.2136170094265));
#59159=CARTESIAN_POINT('Ctrl Pts',(2.58545956967184,-1.56670885598474,16.37162764728));
#59160=CARTESIAN_POINT('Ctrl Pts',(2.72474795870796,1.30954975957442,16.5296382851335));
#59161=CARTESIAN_POINT('Ctrl Pts',(0.391816412777878,2.9975835984028,16.687648922987));
#59162=CARTESIAN_POINT('Ctrl Pts',(-2.29663320724372,1.9659161267294,16.8456595608405));
#59163=CARTESIAN_POINT('Ctrl Pts',(-2.90126747784539,-0.84961803920536,
17.003670198694));
#59164=CARTESIAN_POINT('Ctrl Pts',(-0.87356506601582,-2.89399653715471,
17.1616808365475));
#59165=CARTESIAN_POINT('Ctrl Pts',(1.94684031110808,-2.31311466508161,17.319691474401));
#59166=CARTESIAN_POINT('Ctrl Pts',(3.0006467942943,0.367522881872776,17.4777021122545));
#59167=CARTESIAN_POINT('Ctrl Pts',(1.3322506377027,2.71275930462191,17.635712750108));
#59168=CARTESIAN_POINT('Ctrl Pts',(-1.5456030263841,2.6003875028527,17.7937233879614));
#59169=CARTESIAN_POINT('Ctrl Pts',(-3.01981044854997,0.12114595660455,17.951734025815));
#59170=CARTESIAN_POINT('Ctrl Pts',(-2.17766269355992,-1.59359593510352,
18.0570744510506));
#59171=CARTESIAN_POINT('Ctrl Pts',(-1.4873861107552,-2.08582659521598,18.1097446636685));
#59172=CARTESIAN_POINT('Ctrl Pts',(-1.20564430054386,2.47375567929492,-0.109744663668461));
#59173=CARTESIAN_POINT('Ctrl Pts',(-2.02430085661326,2.07476372580934,-0.0570744510506297));
#59174=CARTESIAN_POINT('Ctrl Pts',(-3.22080179683223,0.407547351185454,
0.0482659741850331));
#59175=CARTESIAN_POINT('Ctrl Pts',(-2.09893472399684,-2.48066857006502,
0.206276612038529));
#59176=CARTESIAN_POINT('Ctrl Pts',(0.930032653994585,-3.11042203369498,
0.364287249892023));
#59177=CARTESIAN_POINT('Ctrl Pts',(3.11378015967401,-0.921861134895831,
0.522297887745518));
#59178=CARTESIAN_POINT('Ctrl Pts',(2.47304163788057,2.10511731480007,0.680308525599012));
#59179=CARTESIAN_POINT('Ctrl Pts',(-0.411921255881383,3.22103361649641,
0.838319163452508));
#59180=CARTESIAN_POINT('Ctrl Pts',(-2.92294152794244,1.41497547719382,0.996329801306002));
#59181=CARTESIAN_POINT('Ctrl Pts',(-2.782012004001,-1.67520776347199,1.1543404391595));
#59182=CARTESIAN_POINT('Ctrl Pts',(-0.11684429743043,-3.24528685950767,
1.31235107701299));
#59183=CARTESIAN_POINT('Ctrl Pts',(2.65431071186993,-1.8709197608499,1.47036171486649));
#59184=CARTESIAN_POINT('Ctrl Pts',(3.01716263687821,1.20101725163484,1.62837235271998));
#59185=CARTESIAN_POINT('Ctrl Pts',(0.64246495318351,3.18322196362623,1.78638299057348));
#59186=CARTESIAN_POINT('Ctrl Pts',(-2.31515207915632,2.27722652153029,1.94439362842697));
#59187=CARTESIAN_POINT('Ctrl Pts',(-3.17217988045057,-0.69495539800879,
2.10240426628047));
#59188=CARTESIAN_POINT('Ctrl Pts',(-1.15101395178073,-3.03658504326113,
2.26041490413396));
#59189=CARTESIAN_POINT('Ctrl Pts',(1.91449313683208,-2.62305202786106,2.41842554198746));
#59190=CARTESIAN_POINT('Ctrl Pts',(3.24293635837937,0.170437969963035,2.57643617984095));
#59191=CARTESIAN_POINT('Ctrl Pts',(1.62898780251483,2.80928519111911,2.73444681769445));
#59192=CARTESIAN_POINT('Ctrl Pts',(-1.46297920814739,2.89920281960699,2.89245745554793));
#59193=CARTESIAN_POINT('Ctrl Pts',(-3.22755118478904,0.358606147391836,
3.05046809340144));
#59194=CARTESIAN_POINT('Ctrl Pts',(-2.06369084652567,-2.50736216356323,
3.20847873125493));
#59195=CARTESIAN_POINT('Ctrl Pts',(0.97260420496244,-3.09834247265461,3.36648936910842));
#59196=CARTESIAN_POINT('Ctrl Pts',(3.12643283597106,-0.878124543467593,
3.52450000696191));
#59197=CARTESIAN_POINT('Ctrl Pts',(2.44357620247262,2.13883620806886,3.68251064481542));
#59198=CARTESIAN_POINT('Ctrl Pts',(-0.456393977529832,3.21518110406747,
3.84052128266891));
#59199=CARTESIAN_POINT('Ctrl Pts',(-2.94226728276043,1.37431736762162,3.9985319205224));
#59200=CARTESIAN_POINT('Ctrl Pts',(-2.75855301808134,-1.71349649423752,
4.1565425583759));
#59201=CARTESIAN_POINT('Ctrl Pts',(-0.0719394114111575,-3.24661511610562,
4.31455319622939));
#59202=CARTESIAN_POINT('Ctrl Pts',(2.67994649732378,-1.8340042970964,4.47256383408289));
#59203=CARTESIAN_POINT('Ctrl Pts',(3.00025458913671,1.24264129603545,4.63057447193638));
#59204=CARTESIAN_POINT('Ctrl Pts',(0.598361879160862,3.19180952627872,4.78858510978988));
#59205=CARTESIAN_POINT('Ctrl Pts',(-2.3464384871139,2.24497470287464,4.94659574764337));
#59206=CARTESIAN_POINT('Ctrl Pts',(-3.16226061460543,-0.738777906869158,
5.10460638549687));
#59207=CARTESIAN_POINT('Ctrl Pts',(-1.10889010364238,-3.05222013105805,
5.26261702335036));
#59208=CARTESIAN_POINT('Ctrl Pts',(1.95060220118706,-2.59631200804096,5.42062766120385));
#59209=CARTESIAN_POINT('Ctrl Pts',(3.2402677402008,0.215290413604578,5.57863829905735));
#59210=CARTESIAN_POINT('Ctrl Pts',(1.58996296055057,2.83155483338342,5.73664893691084));
#59211=CARTESIAN_POINT('Ctrl Pts',(-1.50295221014919,2.87868366521655,5.89465957476434));
#59212=CARTESIAN_POINT('Ctrl Pts',(-3.23220386829704,0.313915823339817,
6.05267021261783));
#59213=CARTESIAN_POINT('Ctrl Pts',(-2.02880174639727,-2.53567514957916,
6.21068085047134));
#59214=CARTESIAN_POINT('Ctrl Pts',(1.01537940831591,-3.08458905651069,6.36869148832482));
#59215=CARTESIAN_POINT('Ctrl Pts',(3.13828319894088,-0.834783536986071,
6.52670212617832));
#59216=CARTESIAN_POINT('Ctrl Pts',(2.41374961827058,2.17244051027326,6.68471276403182));
#59217=CARTESIAN_POINT('Ctrl Pts',(-0.500835156738408,3.20855873191569,
6.84272340188529));
#59218=CARTESIAN_POINT('Ctrl Pts',(-2.96100054007592,1.33347695594927,7.00073403973882));
#59219=CARTESIAN_POINT('Ctrl Pts',(-2.73458123370692,-1.75149949090362,
7.15874467759228));
#59220=CARTESIAN_POINT('Ctrl Pts',(-0.0270127428641371,-3.24729969391502,
7.31675531544581));
#59221=CARTESIAN_POINT('Ctrl Pts',(2.70506503814037,-1.79674932302986,7.47476595329927));
#59222=CARTESIAN_POINT('Ctrl Pts',(2.98277436572273,1.28403351730591,7.6327765911528));
#59223=CARTESIAN_POINT('Ctrl Pts',(0.554143104932792,3.19978286913864,7.79078722900626));
#59224=CARTESIAN_POINT('Ctrl Pts',(-2.37727508935116,2.21229476786618,7.94879786685977));
#59225=CARTESIAN_POINT('Ctrl Pts',(-3.15173627811299,-0.782459854308269,
8.10680850471327));
#59226=CARTESIAN_POINT('Ctrl Pts',(-1.06655380380616,-3.06727044356448,
8.26481914256675));
#59227=CARTESIAN_POINT('Ctrl Pts',(1.98633775439715,-2.56907518687836,8.42282978042027));
#59228=CARTESIAN_POINT('Ctrl Pts',(3.23697884782595,0.260101766824033,8.58084041827374));
#59229=CARTESIAN_POINT('Ctrl Pts',(1.55063371117118,2.85328233516369,8.73885105612725));
#59230=CARTESIAN_POINT('Ctrl Pts',(-1.54263747341621,2.85761344761494,8.89686169398074));
#59231=CARTESIAN_POINT('Ctrl Pts',(-3.236237782651,0.269165385069836,9.05487233183424));
#59232=CARTESIAN_POINT('Ctrl Pts',(-1.99352424747931,-2.5635026945743,9.21288296968773));
#59233=CARTESIAN_POINT('Ctrl Pts',(1.05796022486326,-3.07024512913626,9.37089360754123));
#59234=CARTESIAN_POINT('Ctrl Pts',(3.14953276744873,-0.791282716318499,
9.52890424539472));
#59235=CARTESIAN_POINT('Ctrl Pts',(2.38346094346486,2.20562891741908,9.68691488324822));
#59236=CARTESIAN_POINT('Ctrl Pts',(-0.545180455417489,3.20132211147338,
9.8449255211017));
#59237=CARTESIAN_POINT('Ctrl Pts',(-2.97916694126347,1.29238126203549,10.0029361589552));
#59238=CARTESIAN_POINT('Ctrl Pts',(-2.71008593889043,-1.78916717894277,
10.1609467968087));
#59239=CARTESIAN_POINT('Ctrl Pts',(0.0179190969869355,-3.24736260622999,
10.3189574346622));
#59240=CARTESIAN_POINT('Ctrl Pts',(2.72966571920753,-1.75915037781335,10.4769680725157));
#59241=CARTESIAN_POINT('Ctrl Pts',(2.96472311763905,1.3251799221669,10.6349787103692));
#59242=CARTESIAN_POINT('Ctrl Pts',(0.509818245120129,3.20714364307561,10.7929893482227));
#59243=CARTESIAN_POINT('Ctrl Pts',(-2.407656584187,2.17919130940784,10.9509999860762));
#59244=CARTESIAN_POINT('Ctrl Pts',(-3.14060857075865,-0.82599200701634,
11.1090106239297));
#59245=CARTESIAN_POINT('Ctrl Pts',(-1.02401332207554,-3.08173355541803,
11.2670212617832));
#59246=CARTESIAN_POINT('Ctrl Pts',(2.02169304155291,-2.54134653994968,11.4250318996367));
#59247=CARTESIAN_POINT('Ctrl Pts',(3.23307026568617,0.304863325957073,11.5830425374901));
#59248=CARTESIAN_POINT('Ctrl Pts',(1.51100760726029,2.87446360234028,11.7410531753437));
#59249=CARTESIAN_POINT('Ctrl Pts',(-1.58202741295769,2.83599616625768,11.8990638131971));
#59250=CARTESIAN_POINT('Ctrl Pts',(-3.23965214911027,0.224363417567839,
12.0570744510506));
#59251=CARTESIAN_POINT('Ctrl Pts',(-1.95786510671885,-2.59083948060657,
12.2150850889041));
#59252=CARTESIAN_POINT('Ctrl Pts',(1.10033850467697,-3.05531343163102,12.3730957267576));
#59253=CARTESIAN_POINT('Ctrl Pts',(3.1601793869378,-0.747630411867695,12.5311063646111));
#59254=CARTESIAN_POINT('Ctrl Pts',(2.35271597703043,2.2383950772371,12.6891170024646));
#59255=CARTESIAN_POINT('Ctrl Pts',(-0.589421384323778,3.19347262742205,
12.8471276403181));
#59256=CARTESIAN_POINT('Ctrl Pts',(-2.99676300839876,1.25103815363699,13.0051382781716));
#59257=CARTESIAN_POINT('Ctrl Pts',(-2.68507182310164,-1.82649234740857,
13.1631489160251));
#59258=CARTESIAN_POINT('Ctrl Pts',(0.0628475063948363,-3.24680384092056,
13.3211595538786));
#59259=CARTESIAN_POINT('Ctrl Pts',(2.75374383092715,-1.72121465944234,13.4791701917321));
#59260=CARTESIAN_POINT('Ctrl Pts',(2.9461043006509,1.36607263349075,13.6371808295856));
#59261=CARTESIAN_POINT('Ctrl Pts',(0.465395785284136,3.2138904390286,13.7951914674391));
#59262=CARTESIAN_POINT('Ctrl Pts',(-2.43757715532447,2.14567066465713,13.9532021052926));
#59263=CARTESIAN_POINT('Ctrl Pts',(-3.12887962291158,-0.869366030781908,
14.1112127431461));
#59264=CARTESIAN_POINT('Ctrl Pts',(-0.981276802297831,-3.09560669852456,
14.2692233809996));
#59265=CARTESIAN_POINT('Ctrl Pts',(2.05666129395213,-2.51313137424132,14.4272340188531));
#59266=CARTESIAN_POINT('Ctrl Pts',(3.22854274253641,0.349566519125767,14.5852446567066));
#59267=CARTESIAN_POINT('Ctrl Pts',(1.47109223392897,2.89509458509389,14.74325529456));
#59268=CARTESIAN_POINT('Ctrl Pts',(-1.62111448613489,2.81383594975718,14.9012659324135));
#59269=CARTESIAN_POINT('Ctrl Pts',(-3.2424463174601,0.179518516509487,15.059276570267));
#59270=CARTESIAN_POINT('Ctrl Pts',(-1.92183114416979,-2.61768031011958,
15.2172872081205));
#59271=CARTESIAN_POINT('Ctrl Pts',(1.14250612229568,-3.03979675411041,15.375297845974));
#59272=CARTESIAN_POINT('Ctrl Pts',(3.17022104314579,-0.703835111158572,
15.5333084838275));
#59273=CARTESIAN_POINT('Ctrl Pts',(2.32152055908849,2.27073296659308,15.691319121681));
#59274=CARTESIAN_POINT('Ctrl Pts',(-0.633549386608433,3.18501130561246,
15.8493297595345));
#59275=CARTESIAN_POINT('Ctrl Pts',(-3.01378553969219,1.20945645638823,16.007340397388));
#59276=CARTESIAN_POINT('Ctrl Pts',(-2.65954335641947,-1.8634695906582,16.1653510352415));
#59277=CARTESIAN_POINT('Ctrl Pts',(0.107763275572369,-3.24562018144752,
16.323361673095));
#59278=CARTESIAN_POINT('Ctrl Pts',(2.77729592639622,-1.68295577877773,16.4813723109485));
#59279=CARTESIAN_POINT('Ctrl Pts',(2.92691925835708,1.40671594920387,16.639382948802));
#59280=CARTESIAN_POINT('Ctrl Pts',(0.420888471770377,3.21999880196654,16.7973935866555));
#59281=CARTESIAN_POINT('Ctrl Pts',(-2.46703917776361,2.11178349661654,16.955404224509));
#59282=CARTESIAN_POINT('Ctrl Pts',(-3.11653620196762,-0.912658138985028,
17.1134148623625));
#59283=CARTESIAN_POINT('Ctrl Pts',(-0.938381991251102,-3.10872577081711,
17.2714255002159));
#59284=CARTESIAN_POINT('Ctrl Pts',(2.09129229047302,-2.48474352953584,17.4294361380695));
#59285=CARTESIAN_POINT('Ctrl Pts',(3.2232892813734,0.39479240544154,17.5874467759229));
#59286=CARTESIAN_POINT('Ctrl Pts',(1.43110119084175,2.91404106813249,17.7454574137765));
#59287=CARTESIAN_POINT('Ctrl Pts',(-1.66028393534192,2.79333148483199,17.9034680516299));
#59288=CARTESIAN_POINT('Ctrl Pts',(-3.24387484361673,0.130134764327401,
18.0614786894834));
#59289=CARTESIAN_POINT('Ctrl Pts',(-2.33924127023062,-1.7118378298394,18.1668191147191));
#59290=CARTESIAN_POINT('Ctrl Pts',(-1.59774743137953,-2.24059110187421,
18.2194893273369));
#59291=CARTESIAN_POINT('Ctrl Pts',(-1.28892185405323,2.64462557919718,0.));
#59292=CARTESIAN_POINT('Ctrl Pts',(-2.16412553195875,2.2180740264656,0.0526702126178316));
#59293=CARTESIAN_POINT('Ctrl Pts',(-3.44327246571677,0.435697898018116,
0.158010637853495));
#59294=CARTESIAN_POINT('Ctrl Pts',(-2.24391458970975,-2.65201596455728,
0.31602127570699));
#59295=CARTESIAN_POINT('Ctrl Pts',(0.994272864870662,-3.32526843344238,
0.474031913560484));
#59296=CARTESIAN_POINT('Ctrl Pts',(3.32885851549317,-0.985536913858929,
0.632042551413979));
#59297=CARTESIAN_POINT('Ctrl Pts',(2.64386221675003,2.25052423104204,0.790053189267474));
#59298=CARTESIAN_POINT('Ctrl Pts',(-0.440373921740465,3.44352029787691,
0.948063827120969));
#59299=CARTESIAN_POINT('Ctrl Pts',(-3.12483807353904,1.51271217778069,1.10607446497446));
#59300=CARTESIAN_POINT('Ctrl Pts',(-2.97417411468528,-1.79091950705915,
1.26408510282796));
#59301=CARTESIAN_POINT('Ctrl Pts',(-0.124915091799196,-3.46944878684731,
1.42209574068145));
#59302=CARTESIAN_POINT('Ctrl Pts',(2.8376521022274,-2.00014993298748,1.58010637853495));
#59303=CARTESIAN_POINT('Ctrl Pts',(3.22556732375462,1.2839752006697,1.73811701638844));
#59304=CARTESIAN_POINT('Ctrl Pts',(0.68684198005001,3.40309687805045,1.89612765424193));
#59305=CARTESIAN_POINT('Ctrl Pts',(-2.47506674143882,2.43452154910535,2.05413829209543));
#59306=CARTESIAN_POINT('Ctrl Pts',(-3.39129208428754,-0.742958101059912,
2.21214892994892));
#59307=CARTESIAN_POINT('Ctrl Pts',(-1.23051801937037,-3.24633129537869,
2.37015956780242));
#59308=CARTESIAN_POINT('Ctrl Pts',(2.04673305583136,-2.80423428494102,2.52817020565591));
#59309=CARTESIAN_POINT('Ctrl Pts',(3.46693592938937,0.182210643841385,2.68618084350942));
#59310=CARTESIAN_POINT('Ctrl Pts',(1.74150699149031,3.00333114457405,2.8441914813629));
#59311=CARTESIAN_POINT('Ctrl Pts',(-1.56403167381627,3.09945965973429,3.0022021192164));
#59312=CARTESIAN_POINT('Ctrl Pts',(-3.45048805462229,0.38337617501506,3.1602127570699));
#59313=CARTESIAN_POINT('Ctrl Pts',(-2.20623630941293,-2.68055336651533,
3.31822339492339));
#59314=CARTESIAN_POINT('Ctrl Pts',(1.03978496357064,-3.31235450003327,3.47623403277689));
#59315=CARTESIAN_POINT('Ctrl Pts',(3.34238515098937,-0.938779301776967,
3.63424467063038));
#59316=CARTESIAN_POINT('Ctrl Pts',(2.61236151325119,2.28657219179548,3.79225530848387));
#59317=CARTESIAN_POINT('Ctrl Pts',(-0.487918510817076,3.43726353444563,
3.95026594633737));
#59318=CARTESIAN_POINT('Ctrl Pts',(-3.14549871757786,1.46924568774838,4.10827658419087));
#59319=CARTESIAN_POINT('Ctrl Pts',(-2.94909474458238,-1.83185295801596,
4.26628722204435));
#59320=CARTESIAN_POINT('Ctrl Pts',(-0.0769084874318037,-3.4708687902066,
4.42429785989786));
#59321=CARTESIAN_POINT('Ctrl Pts',(2.8650586300917,-1.96068460481156,4.58230849775135));
#59322=CARTESIAN_POINT('Ctrl Pts',(3.20749138524309,1.32847434561472,4.74031913560485));
#59323=CARTESIAN_POINT('Ctrl Pts',(0.63969257129564,3.41227761002162,4.89832977345833));
#59324=CARTESIAN_POINT('Ctrl Pts',(-2.50851419765219,2.40004199831291,5.05634041131184));
#59325=CARTESIAN_POINT('Ctrl Pts',(-3.3806876642955,-0.789807565154828,
5.21435104916532));
#59326=CARTESIAN_POINT('Ctrl Pts',(-1.18548454770891,-3.26304634669391,
5.37236168701883));
#59327=CARTESIAN_POINT('Ctrl Pts',(2.08533628412643,-2.77564724985249,5.53037232487231));
#59328=CARTESIAN_POINT('Ctrl Pts',(3.4640829815598,0.230161183475004,5.68838296272581));
#59329=CARTESIAN_POINT('Ctrl Pts',(1.6997865838742,3.02713901940368,5.84639360057932));
#59330=CARTESIAN_POINT('Ctrl Pts',(-1.60676573379481,3.07752318435047,6.00440423843279));
#59331=CARTESIAN_POINT('Ctrl Pts',(-3.45546211326527,0.335598953068766,
6.1624148762863));
#59332=CARTESIAN_POINT('Ctrl Pts',(-2.16893731201919,-2.7108220174043,6.32042551413978));
#59333=CARTESIAN_POINT('Ctrl Pts',(1.08551478155176,-3.2976510932094,6.47843615199329));
#59334=CARTESIAN_POINT('Ctrl Pts',(3.35505405491351,-0.89244459890855,6.63644678984678));
#59335=CARTESIAN_POINT('Ctrl Pts',(2.58047471530221,2.3224976463279,6.79445742770027));
#59336=CARTESIAN_POINT('Ctrl Pts',(-0.535429378720641,3.43018373471677,
6.95246806555377));
#59337=CARTESIAN_POINT('Ctrl Pts',(-3.16552593849257,1.42558430345014,7.11047870340726));
#59338=CARTESIAN_POINT('Ctrl Pts',(-2.92346715546102,-1.87248093834177,
7.26848934126076));
#59339=CARTESIAN_POINT('Ctrl Pts',(-0.0288785959505942,-3.47160065390715,
7.42649997911425));
#59340=CARTESIAN_POINT('Ctrl Pts',(2.89191218564355,-1.92085631530288,7.58451061696775));
#59341=CARTESIAN_POINT('Ctrl Pts',(3.18880374912866,1.37272565469421,7.74252125482125));
#59342=CARTESIAN_POINT('Ctrl Pts',(0.592419470567429,3.4208016961533,7.90053189267473));
#59343=CARTESIAN_POINT('Ctrl Pts',(-2.54148077868312,2.36510475985672,8.05854253052824));
#59344=CARTESIAN_POINT('Ctrl Pts',(-3.36943637956882,-0.836506758819556,
8.21655316838173));
#59345=CARTESIAN_POINT('Ctrl Pts',(-1.14022394965853,-3.2791362304939,8.37456380623523));
#59346=CARTESIAN_POINT('Ctrl Pts',(2.12354020171506,-2.7465290978274,8.53257444408871));
#59347=CARTESIAN_POINT('Ctrl Pts',(3.46056691529078,0.278067794444923,8.69058508194221));
#59348=CARTESIAN_POINT('Ctrl Pts',(1.65774074248821,3.05036730644152,8.84859571979571));
#59349=CARTESIAN_POINT('Ctrl Pts',(-1.64919218004073,3.05499758212755,9.00660635764919));
#59350=CARTESIAN_POINT('Ctrl Pts',(-3.45977466246891,0.287757464630905,
9.16461699550271));
#59351=CARTESIAN_POINT('Ctrl Pts',(-2.13122308793902,-2.74057169637072,
9.32262763335619));
#59352=CARTESIAN_POINT('Ctrl Pts',(1.13103678583326,-3.28231638673127,9.48063827120969));
#59353=CARTESIAN_POINT('Ctrl Pts',(3.36708066565756,-0.845939042997581,
9.63864890906319));
#59354=CARTESIAN_POINT('Ctrl Pts',(2.54809390873282,2.35797847865313,9.79665954691667));
#59355=CARTESIAN_POINT('Ctrl Pts',(-0.582837743332163,3.42244725868203,
9.95467018477017));
#59356=CARTESIAN_POINT('Ctrl Pts',(-3.18494714878616,1.38165000378226,10.1126808226237));
#59357=CARTESIAN_POINT('Ctrl Pts',(-2.89727989542405,-1.9127504492443,10.2706914604771));
#59358=CARTESIAN_POINT('Ctrl Pts',(0.0191568240325155,-3.47166791176887,
10.4287020983307));
#59359=CARTESIAN_POINT('Ctrl Pts',(2.91821211128312,-1.88066029550081,10.5867127361841));
#59360=CARTESIAN_POINT('Ctrl Pts',(3.16950564591737,1.41671416807011,10.7447233740376));
#59361=CARTESIAN_POINT('Ctrl Pts',(0.545032956597581,3.42867090134576,10.9027340118911));
#59362=CARTESIAN_POINT('Ctrl Pts',(-2.5739608166471,2.32971474388563,11.0607446497446));
#59363=CARTESIAN_POINT('Ctrl Pts',(-3.3575400473023,-0.883045810971261,
11.2187552875982));
#59364=CARTESIAN_POINT('Ctrl Pts',(-1.0947450662434,-3.29459835388904,11.3767659254516));
#59365=CARTESIAN_POINT('Ctrl Pts',(2.16133758710544,-2.71688514812053,11.5347765633051));
#59366=CARTESIAN_POINT('Ctrl Pts',(3.45638835538215,0.325921171897996,11.6927872011586));
#59367=CARTESIAN_POINT('Ctrl Pts',(1.61537754191679,3.07301162877451,11.8507978390121));
#59368=CARTESIAN_POINT('Ctrl Pts',(-1.69130290364466,3.03188712877575,12.0088084768656));
#59369=CARTESIAN_POINT('Ctrl Pts',(-3.4634248697026,0.239860887678766,12.1668191147191));
#59370=CARTESIAN_POINT('Ctrl Pts',(-2.09310086084253,-2.76979671814595,
12.3248297525726));
#59371=CARTESIAN_POINT('Ctrl Pts',(1.17634226354706,-3.26635331103479,12.4828403904261));
#59372=CARTESIAN_POINT('Ctrl Pts',(3.3784626798429,-0.799271539853375,12.6408510282796));
#59373=CARTESIAN_POINT('Ctrl Pts',(2.51522529307098,2.39300789773122,12.7988616661331));
#59374=CARTESIAN_POINT('Ctrl Pts',(-0.630134529030243,3.41405558666711,
12.9568723039866));
#59375=CARTESIAN_POINT('Ctrl Pts',(-3.2037586303034,1.33745119995158,13.1148829418401));
#59376=CARTESIAN_POINT('Ctrl Pts',(-2.87053797785727,-1.95265378169492,
13.2728935796936));
#59377=CARTESIAN_POINT('Ctrl Pts',(0.0671885766212145,-3.47107055082396,
13.4309042175471));
#59378=CARTESIAN_POINT('Ctrl Pts',(2.94395337210586,-1.84010424058848,13.5889148554006));
#59379=CARTESIAN_POINT('Ctrl Pts',(3.14960077007479,1.46043146451736,13.746925493254));
#59380=CARTESIAN_POINT('Ctrl Pts',(0.497542101071137,3.43588371920981,13.9049361311076));
#59381=CARTESIAN_POINT('Ctrl Pts',(-2.6059480934977,2.29387872528407,14.062946768961));
#59382=CARTESIAN_POINT('Ctrl Pts',(-3.34500094501622,-0.929415811728904,
14.2209574068145));
#59383=CARTESIAN_POINT('Ctrl Pts',(-1.04905660383138,-3.30942975758444,
14.378968044668));
#59384=CARTESIAN_POINT('Ctrl Pts',(2.19872120406036,-2.6867210742881,14.5369786825215));
#59385=CARTESIAN_POINT('Ctrl Pts',(3.45154810230765,0.373712151870365,14.694989320375));
#59386=CARTESIAN_POINT('Ctrl Pts',(1.57270509119793,3.09506765684991,14.8529999582285));
#59387=CARTESIAN_POINT('Ctrl Pts',(-1.73308984097463,3.0081962380834,15.011010596082));
#59388=CARTESIAN_POINT('Ctrl Pts',(-3.46641203983924,0.191918411617718,
15.1690212339355));
#59389=CARTESIAN_POINT('Ctrl Pts',(-2.0545779218657,-2.79849152616241,15.327031871789));
#59390=CARTESIAN_POINT('Ctrl Pts',(1.22142252798128,-3.24976484895722,15.4850425096425));
#59391=CARTESIAN_POINT('Ctrl Pts',(3.38919794407591,-0.752451163260243,
15.643053147496));
#59392=CARTESIAN_POINT('Ctrl Pts',(2.48187511183298,2.42757946439152,15.8010637853495));
#59393=CARTESIAN_POINT('Ctrl Pts',(-0.677310587918214,3.40500981538148,
15.959074423203));
#59394=CARTESIAN_POINT('Ctrl Pts',(-3.22195696009729,1.29299732720621,16.1170850610565));
#59395=CARTESIAN_POINT('Ctrl Pts',(-2.84324618160172,-1.99218515666645,
16.27509569891));
#59396=CARTESIAN_POINT('Ctrl Pts',(0.115206815880023,-3.46980513235694,
16.4331063367635));
#59397=CARTESIAN_POINT('Ctrl Pts',(2.9691322831206,-1.79920270157072,16.591116974617));
#59398=CARTESIAN_POINT('Ctrl Pts',(3.1290905580062,1.50388213883331,16.7491276124704));
#59399=CARTESIAN_POINT('Ctrl Pts',(0.44996053076287,3.44241400553029,16.9071382503239));
#59400=CARTESIAN_POINT('Ctrl Pts',(-2.63744514828349,2.25765086650368,17.0651488881774));
#59401=CARTESIAN_POINT('Ctrl Pts',(-3.33180492608985,-0.975698238764695,
17.2231595260309));
#59402=CARTESIAN_POINT('Ctrl Pts',(-1.00319891648638,-3.32345500447951,
17.3811701638844));
#59403=CARTESIAN_POINT('Ctrl Pts',(2.23574426983795,-2.65637239399007,17.5391808017379));
#59404=CARTESIAN_POINT('Ctrl Pts',(3.44593176845249,0.422061929010304,17.6971914395914));
#59405=CARTESIAN_POINT('Ctrl Pts',(1.5299517439808,3.11532283164306,17.8552020774449));
#59406=CARTESIAN_POINT('Ctrl Pts',(-1.77496484429974,2.98627546681129,18.0132127152984));
#59407=CARTESIAN_POINT('Ctrl Pts',(-3.46793923868349,0.139123572050251,
18.1712233531519));
#59408=CARTESIAN_POINT('Ctrl Pts',(-2.50081984690132,-1.83007972457528,
18.2765637783876));
#59409=CARTESIAN_POINT('Ctrl Pts',(-1.70810875200386,-2.39535560853244,
18.3292339910054));
#59410=CARTESIAN_POINT('',(-1.28892185405336,2.64462557919711,18.));
#59411=CARTESIAN_POINT('Ctrl Pts',(-1.29200505722538,2.64817880365269,18.));
#59412=CARTESIAN_POINT('Ctrl Pts',(-1.36163618241778,2.60626194974374,18.));
#59413=CARTESIAN_POINT('Ctrl Pts',(-1.42923518191538,2.56138581315695,18.));
#59414=CARTESIAN_POINT('Ctrl Pts',(-1.49459061409937,2.51355245406074,18.));
#59415=CARTESIAN_POINT('Ctrl Pts',(-1.57240585429751,2.45659981518786,18.));
#59416=CARTESIAN_POINT('Ctrl Pts',(-1.64704183718319,2.3954553757506,18.));
#59417=CARTESIAN_POINT('Ctrl Pts',(-1.71834950288611,2.3304978961962,18.));
#59418=CARTESIAN_POINT('Ctrl Pts',(-1.79066304650991,2.26462411551435,18.));
#59419=CARTESIAN_POINT('Ctrl Pts',(-1.85955417595172,2.19482804870293,18.));
#59420=CARTESIAN_POINT('Ctrl Pts',(-1.92482309271148,2.12147574581737,18.));
#59421=CARTESIAN_POINT('Ctrl Pts',(-1.98558358441959,2.05319022473766,18.));
#59422=CARTESIAN_POINT('Ctrl Pts',(-2.04320479258379,1.98182188662656,18.));
#59423=CARTESIAN_POINT('Ctrl Pts',(-2.09748654005121,1.90765458443028,18.));
#59424=CARTESIAN_POINT('Ctrl Pts',(-2.10646572746629,1.89538596491152,18.));
#59425=CARTESIAN_POINT('Ctrl Pts',(-2.11535395516661,1.88303990420399,18.));
#59426=CARTESIAN_POINT('Ctrl Pts',(-2.12414062558065,1.87063159113709,18.));
#59427=CARTESIAN_POINT('Ctrl Pts',(-2.17962766214166,1.79227420564738,18.));
#59428=CARTESIAN_POINT('Ctrl Pts',(-2.23116240517441,1.71130999749083,18.));
#59429=CARTESIAN_POINT('Ctrl Pts',(-2.27859485862069,1.62810446801355,18.));
#59430=CARTESIAN_POINT('Ctrl Pts',(-2.32587805625837,1.5451607615642,18.));
#59431=CARTESIAN_POINT('Ctrl Pts',(-2.3690850323679,1.45998884995688,18.));
#59432=CARTESIAN_POINT('Ctrl Pts',(-2.40801882408265,1.37293340222991,18.));
#59433=CARTESIAN_POINT('Ctrl Pts',(-2.44628322593828,1.28737470145007,18.));
#59434=CARTESIAN_POINT('Ctrl Pts',(-2.48042026711449,1.19999579594418,18.));
#59435=CARTESIAN_POINT('Ctrl Pts',(-2.51019309935484,1.11112072325793,18.));
#59436=CARTESIAN_POINT('Ctrl Pts',(-2.52373989101854,1.07068210848132,18.));
#59437=CARTESIAN_POINT('Ctrl Pts',(-2.53638245890231,1.02993377861641,18.));
#59438=CARTESIAN_POINT('Ctrl Pts',(-2.54809485627599,0.988906771366336,
18.));
#59439=CARTESIAN_POINT('Ctrl Pts',(-2.55316334672363,0.971152507426353,
18.));
#59440=CARTESIAN_POINT('Ctrl Pts',(-2.55805761544222,0.953346062512553,
18.));
#59441=CARTESIAN_POINT('Ctrl Pts',(-2.56277542193469,0.935489987393445,
18.));
#59442=CARTESIAN_POINT('Ctrl Pts',(-2.56650095821091,0.921389482060481,
18.));
#59443=CARTESIAN_POINT('Ctrl Pts',(-2.57011653103175,0.907257407319225,
18.));
#59444=CARTESIAN_POINT('Ctrl Pts',(-2.5736173989552,0.893110501520028,18.));
#59445=CARTESIAN_POINT('Ctrl Pts',(-2.59566737033708,0.804007206327108,
18.));
#59446=CARTESIAN_POINT('Ctrl Pts',(-2.61321077029624,0.714169511674567,
18.));
#59447=CARTESIAN_POINT('Ctrl Pts',(-2.62607329651336,0.623911051832834,
18.));
#59448=CARTESIAN_POINT('Ctrl Pts',(-2.63856625673392,0.536245897310476,
18.));
#59449=CARTESIAN_POINT('Ctrl Pts',(-2.64664344597227,0.448183056834854,
18.));
#59450=CARTESIAN_POINT('Ctrl Pts',(-2.65009718893369,0.360012694318155,
18.));
#59451=CARTESIAN_POINT('Ctrl Pts',(-2.65337274389513,0.276391280791186,
18.));
#59452=CARTESIAN_POINT('Ctrl Pts',(-2.65248941241092,0.192672662846889,
18.));
#59453=CARTESIAN_POINT('Ctrl Pts',(-2.64722813834475,0.109115603594406,
18.));
#59454=CARTESIAN_POINT('Ctrl Pts',(-2.64396768384946,0.0573346117613012,
18.));
#59455=CARTESIAN_POINT('Ctrl Pts',(-2.6390249363967,0.00561591434296466,
18.));
#59456=CARTESIAN_POINT('Ctrl Pts',(-2.63242870157844,-0.0459750284110199,
18.));
#59457=CARTESIAN_POINT('Ctrl Pts',(-2.630403908258,-0.0618114865059137,
18.));
#59458=CARTESIAN_POINT('Ctrl Pts',(-2.62822328410621,-0.0776358837596198,
18.));
#59459=CARTESIAN_POINT('Ctrl Pts',(-2.6258875853782,-0.0934462620603028,
18.));
#59460=CARTESIAN_POINT('Ctrl Pts',(-2.62391361832001,-0.106808073482704,
18.));
#59461=CARTESIAN_POINT('Ctrl Pts',(-2.62182902790254,-0.12015847992975,
18.));
#59462=CARTESIAN_POINT('Ctrl Pts',(-2.61963650138613,-0.133484262718106,
18.));
#59463=CARTESIAN_POINT('Ctrl Pts',(-2.60533039958249,-0.22043418271049,
18.));
#59464=CARTESIAN_POINT('Ctrl Pts',(-2.58641281438588,-0.30647770673795,
18.));
#59465=CARTESIAN_POINT('Ctrl Pts',(-2.56311020645715,-0.391323689237884,
18.));
#59466=CARTESIAN_POINT('Ctrl Pts',(-2.53941406581745,-0.47760254438493,
18.));
#59467=CARTESIAN_POINT('Ctrl Pts',(-2.51118302420645,-0.562643940056807,
18.));
#59468=CARTESIAN_POINT('Ctrl Pts',(-2.47860728478706,-0.646118919116556,
18.));
#59469=CARTESIAN_POINT('Ctrl Pts',(-2.44637774874284,-0.728706755781168,
18.));
#59470=CARTESIAN_POINT('Ctrl Pts',(-2.4098946850966,-0.809762009208342,
18.));
#59471=CARTESIAN_POINT('Ctrl Pts',(-2.36930513861691,-0.888932237840673,
18.));
#59472=CARTESIAN_POINT('Ctrl Pts',(-2.35350807431684,-0.919744535607576,
18.));
#59473=CARTESIAN_POINT('Ctrl Pts',(-2.33708865769319,-0.950270887707321,
18.));
#59474=CARTESIAN_POINT('Ctrl Pts',(-2.32005434850432,-0.980488756468179,
18.));
#59475=CARTESIAN_POINT('Ctrl Pts',(-2.31145049889473,-0.99575148273774,
18.));
#59476=CARTESIAN_POINT('Ctrl Pts',(-2.30268977113614,-1.01093549317028,
18.));
#59477=CARTESIAN_POINT('Ctrl Pts',(-2.29377307107857,-1.02603777506919,
18.));
#59478=CARTESIAN_POINT('Ctrl Pts',(-2.28696307843181,-1.03757191079393,
18.));
#59479=CARTESIAN_POINT('Ctrl Pts',(-2.28006311659331,-1.04905657461536,
18.));
#59480=CARTESIAN_POINT('Ctrl Pts',(-2.27307846241723,-1.060482846395,18.));
#59481=CARTESIAN_POINT('Ctrl Pts',(-2.22741856850457,-1.13517836375679,
18.));
#59482=CARTESIAN_POINT('Ctrl Pts',(-2.17808652500359,-1.20747656221673,
18.));
#59483=CARTESIAN_POINT('Ctrl Pts',(-2.12525028267988,-1.27705246380043,
18.));
#59484=CARTESIAN_POINT('Ctrl Pts',(-2.07473471720153,-1.3435724481444,18.));
#59485=CARTESIAN_POINT('Ctrl Pts',(-2.02101528451866,-1.40760435474595,
18.));
#59486=CARTESIAN_POINT('Ctrl Pts',(-1.96421326719147,-1.46882640916218,
18.));
#59487=CARTESIAN_POINT('Ctrl Pts',(-1.94502793769979,-1.48950464105255,
18.));
#59488=CARTESIAN_POINT('Ctrl Pts',(-1.92549077017066,-1.50986197314986,
18.));
#59489=CARTESIAN_POINT('Ctrl Pts',(-1.90560595192038,-1.5298848741256,18.));
#59490=CARTESIAN_POINT('Ctrl Pts',(-1.89094077503979,-1.54465188787328,
18.));
#59491=CARTESIAN_POINT('Ctrl Pts',(-1.87608378637058,-1.55923940543717,
18.));
#59492=CARTESIAN_POINT('Ctrl Pts',(-1.86105580868443,-1.57362393088814,
18.));
#59493=CARTESIAN_POINT('Ctrl Pts',(-1.80044929335635,-1.63163545981358,
18.));
#59494=CARTESIAN_POINT('Ctrl Pts',(-1.73700668600649,-1.68640854165577,
18.));
#59495=CARTESIAN_POINT('Ctrl Pts',(-1.67086296650322,-1.73762479738526,
18.));
#59496=CARTESIAN_POINT('Ctrl Pts',(-1.60658789828107,-1.78739412326861,
18.));
#59497=CARTESIAN_POINT('Ctrl Pts',(-1.53976159075827,-1.83380507910934,
18.));
#59498=CARTESIAN_POINT('Ctrl Pts',(-1.47049053791553,-1.87651975790584,
18.));
#59499=CARTESIAN_POINT('Ctrl Pts',(-1.43981212378135,-1.89543701918527,
18.));
#59500=CARTESIAN_POINT('Ctrl Pts',(-1.40865402146917,-1.91362865851037,
18.));
#59501=CARTESIAN_POINT('Ctrl Pts',(-1.37702479013086,-1.93106208855776,
18.));
#59502=CARTESIAN_POINT('Ctrl Pts',(-2.94047623996122,-0.00254690177668123,
17.1778238829104));
#59503=CARTESIAN_POINT('Ctrl Pts',(-2.94279871458441,-0.28218123486593,
17.1929357639506));
#59504=CARTESIAN_POINT('Ctrl Pts',(-2.9061256239192,-0.561215560283936,
17.2080476449907));
#59505=CARTESIAN_POINT('Ctrl Pts',(-2.82797729485488,-0.828099515505769,
17.2231595260309));
#59506=CARTESIAN_POINT('Ctrl Pts',(-2.5556029228887,-1.7582838273363,17.2758297386488));
#59507=CARTESIAN_POINT('Ctrl Pts',(-1.77940091968755,-2.5408694159079,17.3284999512666));
#59508=CARTESIAN_POINT('Ctrl Pts',(-0.851476053699583,-2.82098177511213,
17.3811701638844));
#59509=CARTESIAN_POINT('Ctrl Pts',(0.0764488122883847,-3.10109413431636,
17.4338403765023));
#59510=CARTESIAN_POINT('Ctrl Pts',(1.15609654106319,-2.87873326415321,17.4865105891201));
#59511=CARTESIAN_POINT('Ctrl Pts',(1.89761832188633,-2.2544804419049,17.5391808017379));
#59512=CARTESIAN_POINT('Ctrl Pts',(2.63914010270947,-1.6302276196566,17.5918510143558));
#59513=CARTESIAN_POINT('Ctrl Pts',(3.04253593558097,-0.604082845323161,
17.6445212269736));
#59514=CARTESIAN_POINT('Ctrl Pts',(2.92490384793812,0.357866358949023,17.6971914395914));
#59515=CARTESIAN_POINT('Ctrl Pts',(2.80727176029526,1.31981556322121,17.7498616522092));
#59516=CARTESIAN_POINT('Ctrl Pts',(2.16861175213802,2.21756919743215,17.8025318648271));
#59517=CARTESIAN_POINT('Ctrl Pts',(1.29846231667931,2.64493812039898,17.8552020774449));
#59518=CARTESIAN_POINT('Ctrl Pts',(0.501074037772838,3.03657081710122,17.9034680516299));
#59519=CARTESIAN_POINT('Ctrl Pts',(-0.490708381591009,3.03319613617707,
17.951734025815));
#59520=CARTESIAN_POINT('Ctrl Pts',(-1.29200505722546,2.64817880365265,18.));
#59521=CARTESIAN_POINT('',(-1.37702479013096,-1.93106208855769,0.));
#59522=CARTESIAN_POINT('Ctrl Pts',(-1.3799494420105,-1.93347660712335,1.42247325030098E-16));
#59523=CARTESIAN_POINT('Ctrl Pts',(-1.43821263219875,-1.90182368491271,
1.23053055000976E-16));
#59524=CARTESIAN_POINT('Ctrl Pts',(-1.49490526047651,-1.86766952812869,
-2.48068321828561E-16));
#59525=CARTESIAN_POINT('Ctrl Pts',(-1.549846300109,-1.83106214637216,-2.13370987545147E-16));
#59526=CARTESIAN_POINT('Ctrl Pts',(-1.61731957854391,-1.78610449579702,
-1.67289625843952E-16));
#59527=CARTESIAN_POINT('Ctrl Pts',(-1.68215240278323,-1.73744874012217,
-3.23480018873332E-16));
#59528=CARTESIAN_POINT('Ctrl Pts',(-1.74427176305372,-1.68546195262933,
-2.84494650060196E-16));
#59529=CARTESIAN_POINT('Ctrl Pts',(-1.80797447841918,-1.63215007832797,
-2.44515586494396E-16));
#59530=CARTESIAN_POINT('Ctrl Pts',(-1.868824194171,-1.57533478867279,-1.55964265601244E-16));
#59531=CARTESIAN_POINT('Ctrl Pts',(-1.92672184730615,-1.51536121788337,
-2.35922392732846E-16));
#59532=CARTESIAN_POINT('Ctrl Pts',(-1.95606181343154,-1.48496926864022,
-2.76441629946403E-16));
#59533=CARTESIAN_POINT('Ctrl Pts',(-1.98464331411229,-1.45376551033272,
6.02784865253053E-16));
#59534=CARTESIAN_POINT('Ctrl Pts',(-2.01245082769788,-1.42179063200257,
6.52256026967279E-16));
#59535=CARTESIAN_POINT('Ctrl Pts',(-2.02687733290328,-1.40520210288967,
6.77921607235376E-16));
#59536=CARTESIAN_POINT('Ctrl Pts',(-2.04109548602495,-1.38840598216825,
-1.37311273491396E-16));
#59537=CARTESIAN_POINT('Ctrl Pts',(-2.05510290128969,-1.37140769097759,
-1.38777878078145E-16));
#59538=CARTESIAN_POINT('Ctrl Pts',(-2.0656990377528,-1.35854905791134,-1.39887314904631E-16));
#59539=CARTESIAN_POINT('Ctrl Pts',(-2.07617457831541,-1.34557473093587,
4.80447834609329E-16));
#59540=CARTESIAN_POINT('Ctrl Pts',(-2.08652842904455,-1.33248699500139,
4.78783679369599E-16));
#59541=CARTESIAN_POINT('Ctrl Pts',(-2.09478335563421,-1.32205239417602,
4.77456880317038E-16));
#59542=CARTESIAN_POINT('Ctrl Pts',(-2.10295522323914,-1.31155289687732,
2.18586909375805E-17));
#59543=CARTESIAN_POINT('Ctrl Pts',(-2.11104250565761,-1.30099164443844,
2.77555756156289E-17));
#59544=CARTESIAN_POINT('Ctrl Pts',(-2.16374877773385,-1.23216206539,6.61866322006358E-17));
#59545=CARTESIAN_POINT('Ctrl Pts',(-2.21288179583151,-1.16069141693027,
-6.93676353204663E-16));
#59546=CARTESIAN_POINT('Ctrl Pts',(-2.25835600178031,-1.08697821947129,
-6.24500451351651E-16));
#59547=CARTESIAN_POINT('Ctrl Pts',(-2.30474705056889,-1.01177882965603,
-5.5392983728813E-16));
#59548=CARTESIAN_POINT('Ctrl Pts',(-2.34733088662335,-0.934244926701822,
-1.69721227198088E-16));
#59549=CARTESIAN_POINT('Ctrl Pts',(-2.38598783736931,-0.854752868970769,
-1.38777878078145E-17));
#59550=CARTESIAN_POINT('Ctrl Pts',(-2.42492693896919,-0.774680611520505,
1.43103127732354E-16));
#59551=CARTESIAN_POINT('Ctrl Pts',(-2.45988224219415,-0.692620710719185,
2.60993908428853E-16));
#59552=CARTESIAN_POINT('Ctrl Pts',(-2.49069311686026,-0.608921827612739,
3.33066907387547E-16));
#59553=CARTESIAN_POINT('Ctrl Pts',(-2.50574516374886,-0.568032384301111,
3.6827675363451E-16));
#59554=CARTESIAN_POINT('Ctrl Pts',(-2.51980745733986,-0.526751310611613,
-3.26906346154409E-16));
#59555=CARTESIAN_POINT('Ctrl Pts',(-2.5328572845043,-0.485117072282149,
-3.19189119579733E-16));
#59556=CARTESIAN_POINT('Ctrl Pts',(-2.53785227082093,-0.469181041242136,
-3.16235253550921E-16));
#59557=CARTESIAN_POINT('Ctrl Pts',(-2.54269948804001,-0.453190870391766,
-7.06596396842216E-16));
#59558=CARTESIAN_POINT('Ctrl Pts',(-2.54739126005051,-0.437171230049419,
-6.80011602582908E-16));
#59559=CARTESIAN_POINT('Ctrl Pts',(-2.57317421298316,-0.349137618863687,
-5.33918719642838E-16));
#59560=CARTESIAN_POINT('Ctrl Pts',(-2.59431180385391,-0.260075883706848,
-3.6235006954443E-17));
#59561=CARTESIAN_POINT('Ctrl Pts',(-2.61068704576328,-0.170387020957126,
-5.55111512312578E-17));
#59562=CARTESIAN_POINT('Ctrl Pts',(-2.62702393945783,-0.0809081952739614,
-7.47421538408212E-17));
#59563=CARTESIAN_POINT('Ctrl Pts',(-2.63862130354526,0.00919573051068487,
-2.73664664561228E-16));
#59564=CARTESIAN_POINT('Ctrl Pts',(-2.64532172794212,0.0995568412614959,
-2.22044604925031E-16));
#59565=CARTESIAN_POINT('Ctrl Pts',(-2.65107237655398,0.177109390970093,
-1.77741616530647E-16));
#59566=CARTESIAN_POINT('Ctrl Pts',(-2.65321550243264,0.254852199236274,
1.12929186103332E-17));
#59567=CARTESIAN_POINT('Ctrl Pts',(-2.65162265236425,0.332562839778456,
0.));
#59568=CARTESIAN_POINT('Ctrl Pts',(-2.65043736981845,0.390389415979805,
1.93522113658955E-17));
#59569=CARTESIAN_POINT('Ctrl Pts',(-2.64718281331851,0.44819839777396,-2.31905195015141E-17));
#59570=CARTESIAN_POINT('Ctrl Pts',(-2.64191368221943,0.505918652854124,
-5.55111512312578E-17));
#59571=CARTESIAN_POINT('Ctrl Pts',(-2.64062714885064,0.520011874833084,
-6.34026935821171E-17));
#59572=CARTESIAN_POINT('Ctrl Pts',(-2.63922017825452,0.534102463086072,
2.85447298507148E-17));
#59573=CARTESIAN_POINT('Ctrl Pts',(-2.63769444945471,0.54818059290278,2.77555756156289E-17));
#59574=CARTESIAN_POINT('Ctrl Pts',(-2.62812339489243,0.636494157297667,
2.28051294793074E-17));
#59575=CARTESIAN_POINT('Ctrl Pts',(-2.61390606721349,0.724122954628742,
-4.18247658184506E-16));
#59576=CARTESIAN_POINT('Ctrl Pts',(-2.59532950233633,0.810804767956044,
-3.60822483003176E-16));
#59577=CARTESIAN_POINT('Ctrl Pts',(-2.57528112215592,0.904354353673597,
-2.98847529529524E-16));
#59578=CARTESIAN_POINT('Ctrl Pts',(-2.55015582011987,0.996801631758693,
-3.84935125803439E-17));
#59579=CARTESIAN_POINT('Ctrl Pts',(-2.52025055163084,1.08782868833812,2.77555756156289E-17));
#59580=CARTESIAN_POINT('Ctrl Pts',(-2.49271682268382,1.1716371418092,8.87509964741449E-17));
#59581=CARTESIAN_POINT('Ctrl Pts',(-2.4611302440109,1.25424238620021,0.));
#59582=CARTESIAN_POINT('Ctrl Pts',(-2.42567698904207,1.33539544644047,0.));
#59583=CARTESIAN_POINT('Ctrl Pts',(-2.40983756184422,1.37165214531589,0.));
#59584=CARTESIAN_POINT('Ctrl Pts',(-2.393225777586,1.40761891354161,-2.28767883718138E-16));
#59585=CARTESIAN_POINT('Ctrl Pts',(-2.37585563123953,1.4432729734042,-2.77555756156289E-16));
#59586=CARTESIAN_POINT('Ctrl Pts',(-2.36243258110441,1.47082520143443,-3.15257341661739E-16));
#59587=CARTESIAN_POINT('Ctrl Pts',(-2.34855663009738,1.49819068371341,-2.16366534335116E-16));
#59588=CARTESIAN_POINT('Ctrl Pts',(-2.33423361450165,1.525358672182,-1.94289029309402E-16));
#59589=CARTESIAN_POINT('Ctrl Pts',(-2.32544410379061,1.54203067285435,-1.80740872107477E-16));
#59590=CARTESIAN_POINT('Ctrl Pts',(-2.31648502739695,1.55863024006332,-2.44555389199E-16));
#59591=CARTESIAN_POINT('Ctrl Pts',(-2.30736938707237,1.57513424614642,-2.22044604925031E-16));
#59592=CARTESIAN_POINT('Ctrl Pts',(-2.26079576520303,1.65945650012684,-1.07032524870574E-16));
#59593=CARTESIAN_POINT('Ctrl Pts',(-2.21007880645611,1.74140267576173,4.6804266504151E-16));
#59594=CARTESIAN_POINT('Ctrl Pts',(-2.15547853607709,1.82066722818668,2.22044604925031E-16));
#59595=CARTESIAN_POINT('Ctrl Pts',(-2.09852378318569,1.90334984065495,-3.45614270312331E-17));
#59596=CARTESIAN_POINT('Ctrl Pts',(-2.0373435353391,1.983115662051,-7.77281236950037E-17));
#59597=CARTESIAN_POINT('Ctrl Pts',(-1.97217568716847,2.05960284446263,-5.55111512312578E-17));
#59598=CARTESIAN_POINT('Ctrl Pts',(-1.95099981991528,2.08445685555532,-4.82918909231929E-17));
#59599=CARTESIAN_POINT('Ctrl Pts',(-1.92940247813391,2.10896449437444,8.29443404019046E-17));
#59600=CARTESIAN_POINT('Ctrl Pts',(-1.90739062217049,2.13311271156995,5.55111512312578E-17));
#59601=CARTESIAN_POINT('Ctrl Pts',(-1.89181625573621,2.15019864852877,3.61009505959917E-17));
#59602=CARTESIAN_POINT('Ctrl Pts',(-1.8760313823833,2.16710758411654,-7.69645308807625E-17));
#59603=CARTESIAN_POINT('Ctrl Pts',(-1.86005799875434,2.18381470943084,-5.55111512312578E-17));
#59604=CARTESIAN_POINT('Ctrl Pts',(-1.79161590462605,2.25540070961311,3.64114034038663E-17));
#59605=CARTESIAN_POINT('Ctrl Pts',(-1.71965512009666,2.32335348522212,6.21368422360659E-16));
#59606=CARTESIAN_POINT('Ctrl Pts',(-1.64441684451929,2.38734608371888,4.44089209850063E-16));
#59607=CARTESIAN_POINT('Ctrl Pts',(-1.57011202763153,2.45054474526429,2.69009447288759E-16));
#59608=CARTESIAN_POINT('Ctrl Pts',(-1.49261003531049,2.5098817110976,1.70169119721682E-16));
#59609=CARTESIAN_POINT('Ctrl Pts',(-1.41210026973023,2.56501611482162,2.22044604925031E-16));
#59610=CARTESIAN_POINT('Ctrl Pts',(-1.37178873803333,2.59262211078115,2.48018848558651E-16));
#59611=CARTESIAN_POINT('Ctrl Pts',(-1.33072251584557,2.61917402239002,1.62339022710125E-17));
#59612=CARTESIAN_POINT('Ctrl Pts',(-1.28892185405323,2.64462557919718,0.));
#59613=CARTESIAN_POINT('Ctrl Pts',(-1.37994944201052,-1.93347660712334,
-9.85539774789324E-16));
#59614=CARTESIAN_POINT('Ctrl Pts',(-0.794121452243435,-2.34631813400529,
0.0482659741850328));
#59615=CARTESIAN_POINT('Ctrl Pts',(0.854011297622218,-2.62815453910416,
0.149202160987898));
#59616=CARTESIAN_POINT('Ctrl Pts',(2.68362344803569,-0.794509576969642,
0.302808560408595));
#59617=CARTESIAN_POINT('Ctrl Pts',(2.13140048014165,1.81430348231616,0.46081919826209));
#59618=CARTESIAN_POINT('Ctrl Pts',(-0.355015924163216,2.7760602537354,0.618829836115584));
#59619=CARTESIAN_POINT('Ctrl Pts',(-2.12533378997424,1.50275432854008,0.748086733996563));
#59620=CARTESIAN_POINT('Ctrl Pts',(-2.36885104996457,0.358299771164603,
0.824673419259709));
#59621=CARTESIAN_POINT('Ctrl Pts',(-2.36807033412218,0.000590439285148986,
0.848589891905023));
#59622=CARTESIAN_POINT('Origin',(0.,0.,-1.848589891905));
#59623=CARTESIAN_POINT('',(1.37702479013102,-1.93106208855765,0.));
#59624=CARTESIAN_POINT('Origin',(0.,0.,0.));
#59625=CARTESIAN_POINT('Ctrl Pts',(1.37702479013102,-1.93106208855765,-4.44089209850063E-15));
#59626=CARTESIAN_POINT('Ctrl Pts',(2.01608411688934,-1.47535404036748,0.0526702126178271));
#59627=CARTESIAN_POINT('Ctrl Pts',(2.79574737452458,0.112154857826279,0.15801063785349));
#59628=CARTESIAN_POINT('Ctrl Pts',(1.43092122672701,2.40744480175264,0.316021275706985));
#59629=CARTESIAN_POINT('Ctrl Pts',(-1.23339961524159,2.5114765043851,0.47403191356048));
#59630=CARTESIAN_POINT('Ctrl Pts',(-2.3262441272451,0.975284966418893,0.585828191023147));
#59631=CARTESIAN_POINT('Ctrl Pts',(-2.37490421603833,0.0976170616511061,
0.644954255867982));
#59632=CARTESIAN_POINT('Ctrl Pts',(-2.37417832678934,0.00170073231846661,
0.651410108094986));
#59633=CARTESIAN_POINT('Ctrl Pts',(1.70810875200392,-2.3953556085324,-0.329233991005388));
#59634=CARTESIAN_POINT('Ctrl Pts',(2.50081984690136,-1.83007972457522,-0.276563778387557));
#59635=CARTESIAN_POINT('Ctrl Pts',(3.46794087734851,0.139120730146379,-0.171223353151894));
#59636=CARTESIAN_POINT('Ctrl Pts',(1.77496373944601,2.9862770556577,-0.0132127152983989));
#59637=CARTESIAN_POINT('Ctrl Pts',(-1.52995116181745,3.11532154565238,0.144797922555096));
#59638=CARTESIAN_POINT('Ctrl Pts',(-3.4459318095318,0.422062600215018,0.302808560408591));
#59639=CARTESIAN_POINT('Ctrl Pts',(-2.23574402944417,-2.65637266992881,
0.460819198262086));
#59640=CARTESIAN_POINT('Ctrl Pts',(1.00319880637436,-3.3234545571268,0.618829836115579));
#59641=CARTESIAN_POINT('Ctrl Pts',(3.3318047603238,-0.975698335728692,0.776840473969075));
#59642=CARTESIAN_POINT('Ctrl Pts',(2.6374449866523,2.25765082687173,0.93485111182257));
#59643=CARTESIAN_POINT('Ctrl Pts',(-0.449960500168118,3.44241375743347,
1.09286174967606));
#59644=CARTESIAN_POINT('Ctrl Pts',(-3.12909038149708,1.50388208255809,1.25087238752956));
#59645=CARTESIAN_POINT('Ctrl Pts',(-2.96913211278082,-1.79920261568766,
1.40888302538306));
#59646=CARTESIAN_POINT('Ctrl Pts',(-0.115206809624608,-3.46980492478986,
1.56689366323655));
#59647=CARTESIAN_POINT('Ctrl Pts',(2.84324601940593,-1.99218504829265,1.72490430109004));
#59648=CARTESIAN_POINT('Ctrl Pts',(3.22195677616531,1.29299725638943,1.88291493894354));
#59649=CARTESIAN_POINT('Ctrl Pts',(0.677310549247169,3.40500961935277,2.04092557679703));
#59650=CARTESIAN_POINT('Ctrl Pts',(-2.48187497014949,2.42757932674622,2.19893621465053));
#59651=CARTESIAN_POINT('Ctrl Pts',(-3.3891977506279,-0.752451120820911,
2.35694685250402));
#59652=CARTESIAN_POINT('Ctrl Pts',(-1.22142245825137,-3.24976466317345,
2.51495749035752));
#59653=CARTESIAN_POINT('Ctrl Pts',(2.05457780458113,-2.7984913665756,2.67296812821101));
#59654=CARTESIAN_POINT('Ctrl Pts',(3.46641184197517,0.191918400748076,2.83097876606451));
#59655=CARTESIAN_POINT('Ctrl Pts',(1.73308974204474,3.00819606632432,2.988989403918));
#59656=CARTESIAN_POINT('Ctrl Pts',(-1.57270500142412,3.09506748020428,3.1470000417715));
#59657=CARTESIAN_POINT('Ctrl Pts',(-3.45154790528896,0.373712130524309,
3.30501067962499));
#59658=CARTESIAN_POINT('Ctrl Pts',(-2.19872107855347,-2.68672092091844,
3.46302131747849));
#59659=CARTESIAN_POINT('Ctrl Pts',(1.0490565439494,-3.3094295686813,3.62103195533198));
#59660=CARTESIAN_POINT('Ctrl Pts',(3.34500075407871,-0.929415758674134,
3.77904259318548));
#59661=CARTESIAN_POINT('Ctrl Pts',(2.6059479447461,2.29387859434484,3.93705323103896));
#59662=CARTESIAN_POINT('Ctrl Pts',(-0.497542072670693,3.43588352308502,
4.09506386889247));
#59663=CARTESIAN_POINT('Ctrl Pts',(-3.14960059029087,1.46043138115332,4.25307450674595));
#59664=CARTESIAN_POINT('Ctrl Pts',(-2.9439532040605,-1.8401041355524,4.41108514459945));
#59665=CARTESIAN_POINT('Ctrl Pts',(-0.0671885727859433,-3.47107035269011,
4.56909578245295));
#59666=CARTESIAN_POINT('Ctrl Pts',(2.87053781400266,-1.95265367023439,4.72710642030644));
#59667=CARTESIAN_POINT('Ctrl Pts',(3.203758447428,1.33745112360787,4.88511705815994));
#59668=CARTESIAN_POINT('Ctrl Pts',(0.630134493061158,3.41405539178769,5.04312769601343));
#59669=CARTESIAN_POINT('Ctrl Pts',(-2.51522514949815,2.39300776113466,5.20113833386693));
#59670=CARTESIAN_POINT('Ctrl Pts',(-3.37846248699513,-0.799271494229795,
5.35914897172041));
#59671=CARTESIAN_POINT('Ctrl Pts',(-1.17634219639961,-3.26635312458643,
5.51715960957392));
#59672=CARTESIAN_POINT('Ctrl Pts',(2.0931007413652,-2.76979656004174,5.67517024742741));
#59673=CARTESIAN_POINT('Ctrl Pts',(3.46342467200507,0.239860873987174,5.83318088528091));
#59674=CARTESIAN_POINT('Ctrl Pts',(1.69130280710249,3.03188695571109,5.9911915231344));
#59675=CARTESIAN_POINT('Ctrl Pts',(-1.61537744970865,3.07301145336234,6.1492021609879));
#59676=CARTESIAN_POINT('Ctrl Pts',(-3.45638815808628,0.325921153293867,
6.30721279884139));
#59677=CARTESIAN_POINT('Ctrl Pts',(-2.16133746373299,-2.71688499303665,
6.46522343669488));
#59678=CARTESIAN_POINT('Ctrl Pts',(1.09474500375374,-3.29459816582837,6.62323407454838));
#59679=CARTESIAN_POINT('Ctrl Pts',(3.35753985564886,-0.883045760565633,
6.78124471240187));
#59680=CARTESIAN_POINT('Ctrl Pts',(2.57396066972148,2.32971461090203,6.93925535025537));
#59681=CARTESIAN_POINT('Ctrl Pts',(-0.545032925486335,3.42867070563204,
7.09726598810886));
#59682=CARTESIAN_POINT('Ctrl Pts',(-3.16950546499722,1.41671408720188,7.25527662596235));
#59683=CARTESIAN_POINT('Ctrl Pts',(-2.91821194470713,-1.88066018814992,
7.41328726381586));
#59684=CARTESIAN_POINT('Ctrl Pts',(-0.0191568229389774,-3.47166771360082,
7.57129790166934));
#59685=CARTESIAN_POINT('Ctrl Pts',(2.89727973004295,-1.91275034006159,7.72930853952286));
#59686=CARTESIAN_POINT('Ctrl Pts',(3.18494696698455,1.38164992491564,7.88731917737633));
#59687=CARTESIAN_POINT('Ctrl Pts',(0.58283771006284,3.42244706332358,8.04532981522985));
#59688=CARTESIAN_POINT('Ctrl Pts',(-2.54809376328382,2.3579783440561,8.20334045308332));
#59689=CARTESIAN_POINT('Ctrl Pts',(-3.3670804734595,-0.845938994710182,
8.36135109093683));
#59690=CARTESIAN_POINT('Ctrl Pts',(-1.13103672127189,-3.28231619937171,
8.51936172879031));
#59691=CARTESIAN_POINT('Ctrl Pts',(2.13122296628565,-2.74057153993471,8.67737236664381));
#59692=CARTESIAN_POINT('Ctrl Pts',(3.45977446497974,0.287757448205339,8.83538300449731));
#59693=CARTESIAN_POINT('Ctrl Pts',(1.64919208590229,3.0549974077437,8.9933936423508));
#59694=CARTESIAN_POINT('Ctrl Pts',(-1.65774064786191,3.05036713232192,9.1514042802043));
#59695=CARTESIAN_POINT('Ctrl Pts',(-3.46056671775639,0.278067778572342,
9.30941491805778));
#59696=CARTESIAN_POINT('Ctrl Pts',(-2.12354008050013,-2.74652894105141,
9.46742555591129));
#59697=CARTESIAN_POINT('Ctrl Pts',(1.14022388457288,-3.27913604331583,9.62543619376477));
#59698=CARTESIAN_POINT('Ctrl Pts',(3.36943618723632,-0.836506711070431,
9.78344683161829));
#59699=CARTESIAN_POINT('Ctrl Pts',(2.54148063361152,2.365104624853,9.94145746947176));
#59700=CARTESIAN_POINT('Ctrl Pts',(-0.592419436751292,3.42080150088876,
10.0994681073253));
#59701=CARTESIAN_POINT('Ctrl Pts',(-3.18880356710694,1.37272557633691,10.2574787451788));
#59702=CARTESIAN_POINT('Ctrl Pts',(-2.8919120205688,-1.92085620565756,10.4154893830323));
#59703=CARTESIAN_POINT('Ctrl Pts',(0.0288785943022343,-3.47160045574294,
10.5735000208857));
#59704=CARTESIAN_POINT('Ctrl Pts',(2.92346698858513,-1.87248083145767,10.7315106587392));
#59705=CARTESIAN_POINT('Ctrl Pts',(3.16552575779954,1.42558422207569,10.8895212965927));
#59706=CARTESIAN_POINT('Ctrl Pts',(0.535429348157471,3.4301835389167,11.0475319344462));
#59707=CARTESIAN_POINT('Ctrl Pts',(-2.58047456800486,2.32249751375618,11.2055425722997));
#59708=CARTESIAN_POINT('Ctrl Pts',(-3.35505386340194,-0.892444547966527,
11.3635532101532));
#59709=CARTESIAN_POINT('Ctrl Pts',(-1.08551471958888,-3.2976509049745,11.5215638480067));
#59710=CARTESIAN_POINT('Ctrl Pts',(2.16893718821302,-2.71082186266645,11.6795744858602));
#59711=CARTESIAN_POINT('Ctrl Pts',(3.45546191602226,0.335598933912326,11.8375851237137));
#59712=CARTESIAN_POINT('Ctrl Pts',(1.60676564207814,3.07752300868082,11.9955957615672));
#59713=CARTESIAN_POINT('Ctrl Pts',(-1.69978648684786,3.02713884660998,12.1536063994207));
#59714=CARTESIAN_POINT('Ctrl Pts',(-3.46408278382471,0.230161170336986,
12.3116170372742));
#59715=CARTESIAN_POINT('Ctrl Pts',(-2.08533616509223,-2.77564709141439,
12.4696276751277));
#59716=CARTESIAN_POINT('Ctrl Pts',(1.18548448003973,-3.26304616043428,12.6276383129812));
#59717=CARTESIAN_POINT('Ctrl Pts',(3.38068747132074,-0.789807520071332,
12.7856489508347));
#59718=CARTESIAN_POINT('Ctrl Pts',(2.50851405446239,2.40004186131487,12.9436595886882));
#59719=CARTESIAN_POINT('Ctrl Pts',(-0.639692534781115,3.41227741524375,
13.1016702265417));
#59720=CARTESIAN_POINT('Ctrl Pts',(-3.20749120215462,1.32847426978314,13.2596808643952));
#59721=CARTESIAN_POINT('Ctrl Pts',(-2.86505846654987,-1.96068449289242,
13.4176915022487));
#59722=CARTESIAN_POINT('Ctrl Pts',(0.0769084830419716,-3.47086859208481,
13.5757021401021));
#59723=CARTESIAN_POINT('Ctrl Pts',(2.94909457624333,-1.83185285344978,13.7337127779556));
#59724=CARTESIAN_POINT('Ctrl Pts',(3.14549853802855,1.46924560387948,13.8917234158091));
#59725=CARTESIAN_POINT('Ctrl Pts',(0.487918482964918,3.43726333824546,14.0497340536626));
#59726=CARTESIAN_POINT('Ctrl Pts',(-2.61236136413192,2.28657206126704,14.2077446915161));
#59727=CARTESIAN_POINT('Ctrl Pts',(-3.34238496020413,-0.938779248176496,
14.3657553293696));
#59728=CARTESIAN_POINT('Ctrl Pts',(-1.03978490421238,-3.31235431098403,
14.5237659672231));
#59729=CARTESIAN_POINT('Ctrl Pts',(2.20623618346753,-2.68055321345958,14.6817766050766));
#59730=CARTESIAN_POINT('Ctrl Pts',(3.45048785768122,0.383376153047962,14.8397872429301));
#59731=CARTESIAN_POINT('Ctrl Pts',(1.56403158450715,3.09945948296467,14.9977978807836));
#59732=CARTESIAN_POINT('Ctrl Pts',(-1.74150689202679,3.00333097286243,15.1558085186371));
#59733=CARTESIAN_POINT('Ctrl Pts',(-3.46693573158834,0.182210633943016,
15.3138191564906));
#59734=CARTESIAN_POINT('Ctrl Pts',(-2.04673293883378,-2.8042341257807,15.4718297943441));
#59735=CARTESIAN_POINT('Ctrl Pts',(1.2305179488465,-3.24633110843195,15.6298404321976));
#59736=CARTESIAN_POINT('Ctrl Pts',(3.39129189118379,-0.742958061601936,
15.7878510700511));
#59737=CARTESIAN_POINT('Ctrl Pts',(2.47506659937511,2.43452141542566,15.9458617079046));
#59738=CARTESIAN_POINT('Ctrl Pts',(-0.686841939590187,3.40309667436876,
16.1038723457581));
#59739=CARTESIAN_POINT('Ctrl Pts',(-3.22556714156735,1.28397514410703,16.2618829836115));
#59740=CARTESIAN_POINT('Ctrl Pts',(-2.83765193744026,-2.00014984832596,
16.4198936214651));
#59741=CARTESIAN_POINT('Ctrl Pts',(0.124915080987664,-3.46944853710508,
16.5779042593186));
#59742=CARTESIAN_POINT('Ctrl Pts',(2.97417394872773,-1.7909194946734,16.735914897172));
#59743=CARTESIAN_POINT('Ctrl Pts',(3.12483789403196,1.51271224602764,16.8939255350255));
#59744=CARTESIAN_POINT('Ctrl Pts',(0.440373887044776,3.44351983848023,17.051936172879));
#59745=CARTESIAN_POINT('Ctrl Pts',(-2.64386202524497,2.25052454290272,17.2099468107325));
#59746=CARTESIAN_POINT('Ctrl Pts',(-3.32885844512377,-0.985537582627644,
17.367957448586));
#59747=CARTESIAN_POINT('Ctrl Pts',(-0.994272503154261,-3.32526706894708,
17.5259680864395));
#59748=CARTESIAN_POINT('Ctrl Pts',(2.24391376251738,-2.65201771409636,17.683978724293));
#59749=CARTESIAN_POINT('Ctrl Pts',(3.44327361237846,0.435700971584197,17.8419893621465));
#59750=CARTESIAN_POINT('Ctrl Pts',(2.16412553195871,2.21807402646564,17.9473297873822));
#59751=CARTESIAN_POINT('Ctrl Pts',(1.28892185405319,2.64462557919719,18.));
#59752=CARTESIAN_POINT('Ctrl Pts',(1.59774743137962,-2.24059110187415,-0.219489327336927));
#59753=CARTESIAN_POINT('Ctrl Pts',(2.33924127023069,-1.71183782983931,-0.166819114719096));
#59754=CARTESIAN_POINT('Ctrl Pts',(3.2438763764072,0.130132106039679,-0.0614786894834324));
#59755=CARTESIAN_POINT('Ctrl Pts',(1.66028290187301,2.79333297102268,0.0965319483700627));
#59756=CARTESIAN_POINT('Ctrl Pts',(-1.43110064629217,2.91403986522995,0.254542586223557));
#59757=CARTESIAN_POINT('Ctrl Pts',(-3.22328931979857,0.394793033279504,
0.412553224077053));
#59758=CARTESIAN_POINT('Ctrl Pts',(-2.0912920656111,-2.48474378764615,0.570563861930546));
#59759=CARTESIAN_POINT('Ctrl Pts',(0.938381888253501,-3.10872535236795,
0.728574499784042));
#59760=CARTESIAN_POINT('Ctrl Pts',(3.11653604691177,-0.912658229684108,
0.886585137637534));
#59761=CARTESIAN_POINT('Ctrl Pts',(2.46703902657541,2.11178345954526,1.04459577549103));
#59762=CARTESIAN_POINT('Ctrl Pts',(-0.42088844315241,3.21999856989931,1.20260641334452));
#59763=CARTESIAN_POINT('Ctrl Pts',(-2.92691909325228,1.40671589656455,1.36061705119802));
#59764=CARTESIAN_POINT('Ctrl Pts',(-2.77729576706211,-1.68295569844364,
1.51862768905151));
#59765=CARTESIAN_POINT('Ctrl Pts',(-0.107763269721067,-3.2456199872914,
1.67663832690501));
#59766=CARTESIAN_POINT('Ctrl Pts',(2.65954320470322,-1.86346948928641,1.8346489647585));
#59767=CARTESIAN_POINT('Ctrl Pts',(3.01378536764409,1.20945639014698,1.992659602612));
#59768=CARTESIAN_POINT('Ctrl Pts',(0.633549350435882,3.18501112224923,2.15067024046549));
#59769=CARTESIAN_POINT('Ctrl Pts',(-2.32152042655924,2.27073283784104,2.30868087831899));
#59770=CARTESIAN_POINT('Ctrl Pts',(-3.17022086219649,-0.703835071461303,
2.46669151617248));
#59771=CARTESIAN_POINT('Ctrl Pts',(-1.14250605707099,-3.03979658033019,
2.62470215402598));
#59772=CARTESIAN_POINT('Ctrl Pts',(1.92183103446304,-2.61768016084369,2.78271279187947));
#59773=CARTESIAN_POINT('Ctrl Pts',(3.24244613238007,0.179518506342186,2.94072342973297));
#59774=CARTESIAN_POINT('Ctrl Pts',(1.62111439359683,2.81383578909553,3.09873406758646));
#59775=CARTESIAN_POINT('Ctrl Pts',(-1.47109214995551,2.89509441986136,3.25674470543996));
#59776=CARTESIAN_POINT('Ctrl Pts',(-3.22854255824715,0.349566499158832,
3.41475534329345));
#59777=CARTESIAN_POINT('Ctrl Pts',(-2.05666117655423,-2.51313123078094,
3.57276598114695));
#59778=CARTESIAN_POINT('Ctrl Pts',(0.981276746284894,-3.09560652182649,
3.73077661900044));
#59779=CARTESIAN_POINT('Ctrl Pts',(3.1288794443106,-0.869365981154969,3.88878725685394));
#59780=CARTESIAN_POINT('Ctrl Pts',(2.43757701618371,2.14567054217795,4.04679789470743));
#59781=CARTESIAN_POINT('Ctrl Pts',(-0.465395758718706,3.21389025557547,
4.20480853256093));
#59782=CARTESIAN_POINT('Ctrl Pts',(-2.94610413248288,1.36607255551284,4.36281917041442));
#59783=CARTESIAN_POINT('Ctrl Pts',(-2.75374367373922,-1.72121456119272,
4.52082980826791));
#59784=CARTESIAN_POINT('Ctrl Pts',(-0.0628475028073083,-3.24680365558819,
4.67884044612141));
#59785=CARTESIAN_POINT('Ctrl Pts',(2.68507166983374,-1.82649224314949,4.8368510839749));
#59786=CARTESIAN_POINT('Ctrl Pts',(2.99676283733896,1.25103808222591,4.9948617218284));
#59787=CARTESIAN_POINT('Ctrl Pts',(0.589421350678613,3.19347244513383,5.1528723596819));
#59788=CARTESIAN_POINT('Ctrl Pts',(-2.35271584273392,2.23839494946604,5.31088299753539));
#59789=CARTESIAN_POINT('Ctrl Pts',(-3.16017920654996,-0.747630369191917,
5.46889363538888));
#59790=CARTESIAN_POINT('Ctrl Pts',(-1.10033844186788,-3.05531325722915,
5.62690427324238));
#59791=CARTESIAN_POINT('Ctrl Pts',(1.95786499496102,-2.59083933271748,5.78491491109587));
#59792=CARTESIAN_POINT('Ctrl Pts',(3.23965196418602,0.224363404760918,5.94292554894936));
#59793=CARTESIAN_POINT('Ctrl Pts',(1.5820273226531,2.83599600437479,6.10093618680287));
#59794=CARTESIAN_POINT('Ctrl Pts',(-1.51100752100979,2.8744634382615,6.25894682465635));
#59795=CARTESIAN_POINT('Ctrl Pts',(-3.23307008113764,0.304863308554905,
6.41695746250985));
#59796=CARTESIAN_POINT('Ctrl Pts',(-2.02169292615153,-2.54134639488584,
6.57496810036335));
#59797=CARTESIAN_POINT('Ctrl Pts',(1.0240132636234,-3.08173337950799,6.73297873821683));
#59798=CARTESIAN_POINT('Ctrl Pts',(3.140608391488,-0.825991959867379,6.89098937607034));
#59799=CARTESIAN_POINT('Ctrl Pts',(2.40765644675425,2.17919118501639,7.04900001392383));
#59800=CARTESIAN_POINT('Ctrl Pts',(-0.509818216019039,3.20714346000698,
7.20701065177733));
#59801=CARTESIAN_POINT('Ctrl Pts',(-2.96472294840821,1.32517984652353,7.36502128963082));
#59802=CARTESIAN_POINT('Ctrl Pts',(-2.72966556339403,-1.75915027739847,
7.52303192748432));
#59803=CARTESIAN_POINT('Ctrl Pts',(-0.0179190959639986,-3.24736242086562,
7.6810425653378));
#59804=CARTESIAN_POINT('Ctrl Pts',(2.71008578419468,-1.78916707681433,7.83905320319131));
#59805=CARTESIAN_POINT('Ctrl Pts',(2.97916677120809,1.29238118826451,7.99706384104479));
#59806=CARTESIAN_POINT('Ctrl Pts',(0.545180424297654,3.2013219287371,8.1550744788983));
#59807=CARTESIAN_POINT('Ctrl Pts',(-2.38346080741339,2.20562879151835,8.31308511675178));
#59808=CARTESIAN_POINT('Ctrl Pts',(-3.14953258766861,-0.791282671151008,
8.47109575460529));
#59809=CARTESIAN_POINT('Ctrl Pts',(-1.05796016447317,-3.07024495388206,
8.62910639245878));
#59810=CARTESIAN_POINT('Ctrl Pts',(1.99352413368603,-2.56350254824561,8.78711703031228));
#59811=CARTESIAN_POINT('Ctrl Pts',(3.23623759792164,0.26916536970558,8.94512766816576));
#59812=CARTESIAN_POINT('Ctrl Pts',(1.54263738536003,2.85761328449809,9.10313830601927));
#59813=CARTESIAN_POINT('Ctrl Pts',(-1.55063362265875,2.85328217229397,9.26114894387275));
#59814=CARTESIAN_POINT('Ctrl Pts',(-3.23697866305431,0.260101751976928,
9.41915958172626));
#59815=CARTESIAN_POINT('Ctrl Pts',(-1.98633764101391,-2.56907504023173,
9.57717021957974));
#59816=CARTESIAN_POINT('Ctrl Pts',(1.06655374292576,-3.06727026848002,9.73518085743324));
#59817=CARTESIAN_POINT('Ctrl Pts',(3.15173609820715,-0.782459809644175,
9.89319149528675));
#59818=CARTESIAN_POINT('Ctrl Pts',(2.37727495365263,2.21229464158513,10.0512021331402));
#59819=CARTESIAN_POINT('Ctrl Pts',(-0.554143073301574,3.19978268649018,
10.2092127709937));
#59820=CARTESIAN_POINT('Ctrl Pts',(-2.9827741954615,1.28403344401124,10.3672234088472));
#59821=CARTESIAN_POINT('Ctrl Pts',(-2.70506488373111,-1.79674922046879,
10.5252340467007));
#59822=CARTESIAN_POINT('Ctrl Pts',(0.027012741322331,-3.24729950855425,
10.6832446845542));
#59823=CARTESIAN_POINT('Ctrl Pts',(2.73458107761294,-1.75149939092527,10.8412553224077));
#59824=CARTESIAN_POINT('Ctrl Pts',(2.96100037105749,1.33347687983249,10.9992659602612));
#59825=CARTESIAN_POINT('Ctrl Pts',(0.500835128149877,3.20855854876633,11.1572765981147));
#59826=CARTESIAN_POINT('Ctrl Pts',(-2.41374948049017,2.17244038626699,11.3152872359682));
#59827=CARTESIAN_POINT('Ctrl Pts',(-3.13828301980291,-0.834783489335473,
11.4732978738217));
#59828=CARTESIAN_POINT('Ctrl Pts',(-1.01537935035641,-3.08458888043772,
11.6313085116752));
#59829=CARTESIAN_POINT('Ctrl Pts',(2.02880163059028,-2.53567500483893,11.7893191495287));
#59830=CARTESIAN_POINT('Ctrl Pts',(3.23220368379796,0.313915805421134,11.9473297873822));
#59831=CARTESIAN_POINT('Ctrl Pts',(1.50295212435831,2.87868350089698,12.1053404252357));
#59832=CARTESIAN_POINT('Ctrl Pts',(-1.58996286979316,2.83155467175394,12.2633510630892));
#59833=CARTESIAN_POINT('Ctrl Pts',(-3.24026755524143,0.215290401315357,
12.4213617009427));
#59834=CARTESIAN_POINT('Ctrl Pts',(-1.95060208984364,-2.59631185983962,
12.5793723387961));
#59835=CARTESIAN_POINT('Ctrl Pts',(1.10889004034537,-3.05221995683268,12.7373829766496));
#59836=CARTESIAN_POINT('Ctrl Pts',(3.16226043409883,-0.738777864698467,
12.8953936145032));
#59837=CARTESIAN_POINT('Ctrl Pts',(2.34643835317558,2.24497457472812,13.0534042523566));
#59838=CARTESIAN_POINT('Ctrl Pts',(-0.598361845005598,3.19180934408549,
13.2114148902101));
#59839=CARTESIAN_POINT('Ctrl Pts',(-3.00025441787765,1.24264122510332,13.3694255280636));
#59840=CARTESIAN_POINT('Ctrl Pts',(-2.6799463443484,-1.83400419240843,13.5274361659171));
#59841=CARTESIAN_POINT('Ctrl Pts',(0.0719394073050037,-3.24661493078452,
13.6854468037706));
#59842=CARTESIAN_POINT('Ctrl Pts',(2.75855286061874,-1.71349639642736,13.8434574416241));
#59843=CARTESIAN_POINT('Ctrl Pts',(2.94226711481182,1.37431728917156,14.0014680794776));
#59844=CARTESIAN_POINT('Ctrl Pts',(0.45639395147716,3.21518092054385,14.1594787173311));
#59845=CARTESIAN_POINT('Ctrl Pts',(-2.44357606298802,2.13883608597385,14.3174893551846));
#59846=CARTESIAN_POINT('Ctrl Pts',(-3.12643265751249,-0.878124493330309,
14.4754999930381));
#59847=CARTESIAN_POINT('Ctrl Pts',(-0.972604149439291,-3.09834229581991,
14.6335106308916));
#59848=CARTESIAN_POINT('Ctrl Pts',(2.06369072871768,-2.50736202039641,14.7915212687451));
#59849=CARTESIAN_POINT('Ctrl Pts',(3.22755100057236,0.358606126844088,14.9495319065986));
#59850=CARTESIAN_POINT('Ctrl Pts',(1.46297912460851,2.89920265425852,15.1075425444521));
#59851=CARTESIAN_POINT('Ctrl Pts',(-1.62898770947773,2.8092850305018,15.2655531823055));
#59852=CARTESIAN_POINT('Ctrl Pts',(-3.2429361733583,0.170437960704151,15.4235638201591));
#59853=CARTESIAN_POINT('Ctrl Pts',(-1.9144930273937,-2.62305187898416,15.5815744580125));
#59854=CARTESIAN_POINT('Ctrl Pts',(1.15101388581347,-3.03658486839304,15.739585095866));
#59855=CARTESIAN_POINT('Ctrl Pts',(3.17217969982332,-0.694955361100154,
15.8975957337195));
#59856=CARTESIAN_POINT('Ctrl Pts',(2.31515194627134,2.27722639648772,16.055606371573));
#59857=CARTESIAN_POINT('Ctrl Pts',(-0.642464915337856,3.18322177310445,
16.2136170094265));
#59858=CARTESIAN_POINT('Ctrl Pts',(-3.01716246646213,1.20101719872665,16.37162764728));
#59859=CARTESIAN_POINT('Ctrl Pts',(-2.6543105577297,-1.87091968165842,16.5296382851335));
#59860=CARTESIAN_POINT('Ctrl Pts',(0.116844287317486,-3.24528662590135,
16.687648922987));
#59861=CARTESIAN_POINT('Ctrl Pts',(2.78201184876604,-1.67520775188644,16.8456595608405));
#59862=CARTESIAN_POINT('Ctrl Pts',(2.92294136003334,1.41497554103137,17.003670198694));
#59863=CARTESIAN_POINT('Ctrl Pts',(0.411921223427336,3.22103318678147,17.1616808365475));
#59864=CARTESIAN_POINT('Ctrl Pts',(-2.47304145874873,2.10511760651132,17.319691474401));
#59865=CARTESIAN_POINT('Ctrl Pts',(-3.11378009385118,-0.921861760455288,
17.4777021122545));
#59866=CARTESIAN_POINT('Ctrl Pts',(-0.930032315648715,-3.11042075736007,
17.635712750108));
#59867=CARTESIAN_POINT('Ctrl Pts',(2.09893395024961,-2.48067020656593,17.7937233879615));
#59868=CARTESIAN_POINT('Ctrl Pts',(3.22080286940782,0.407550226167737,17.951734025815));
#59869=CARTESIAN_POINT('Ctrl Pts',(2.02430085661319,2.07476372580941,18.0570744510506));
#59870=CARTESIAN_POINT('Ctrl Pts',(1.20564430054378,2.47375567929496,18.1097446636685));
#59871=CARTESIAN_POINT('Ctrl Pts',(1.48738611075532,-2.0858265952159,-0.109744663668466));
#59872=CARTESIAN_POINT('Ctrl Pts',(2.17766269356001,-1.59359593510339,-0.0570744510506341));
#59873=CARTESIAN_POINT('Ctrl Pts',(3.01981187546589,0.121143481932978,0.0482659741850286));
#59874=CARTESIAN_POINT('Ctrl Pts',(1.54560206430001,2.60038888638766,0.206276612038524));
#59875=CARTESIAN_POINT('Ctrl Pts',(-1.33225013076688,2.71275818480752,0.364287249892018));
#59876=CARTESIAN_POINT('Ctrl Pts',(-3.00064683006534,0.36752346634399,0.522297887745513));
#59877=CARTESIAN_POINT('Ctrl Pts',(-1.94684010177802,-2.31311490536349,
0.680308525599008));
#59878=CARTESIAN_POINT('Ctrl Pts',(0.873564970132635,-2.8939961476091,0.838319163452502));
#59879=CARTESIAN_POINT('Ctrl Pts',(2.90126733349974,-0.849618123639522,
0.996329801305998));
#59880=CARTESIAN_POINT('Ctrl Pts',(2.29663306649852,1.96591609221879,1.15434043915949));
#59881=CARTESIAN_POINT('Ctrl Pts',(-0.3918163861367,2.99758338236515,1.31235107701299));
#59882=CARTESIAN_POINT('Ctrl Pts',(-2.72474780500748,1.30954971057102,1.47036171486648));
#59883=CARTESIAN_POINT('Ctrl Pts',(-2.58545942134339,-1.56670878119963,
1.62837235271998));
#59884=CARTESIAN_POINT('Ctrl Pts',(-0.100319729817524,-3.02143504979294,
1.78638299057347));
#59885=CARTESIAN_POINT('Ctrl Pts',(2.47584039000051,-1.73475393028017,1.94439362842697));
#59886=CARTESIAN_POINT('Ctrl Pts',(2.80561395912286,1.12591552390453,2.10240426628046));
#59887=CARTESIAN_POINT('Ctrl Pts',(0.589788151624594,2.96501262514568,2.26041490413395));
#59888=CARTESIAN_POINT('Ctrl Pts',(-2.16116588296898,2.11388634893584,2.41842554198745));
#59889=CARTESIAN_POINT('Ctrl Pts',(-2.95124397376509,-0.655219022101695,
2.57643617984094));
#59890=CARTESIAN_POINT('Ctrl Pts',(-1.06358965589061,-2.82982849748694,
2.73444681769444));
#59891=CARTESIAN_POINT('Ctrl Pts',(1.78908426434496,-2.43686895511177,2.89245745554793));
#59892=CARTESIAN_POINT('Ctrl Pts',(3.01848042278497,0.167118611936303,3.05046809340143));
#59893=CARTESIAN_POINT('Ctrl Pts',(1.50913904514892,2.61947551186673,3.20847873125492));
#59894=CARTESIAN_POINT('Ctrl Pts',(-1.36947929848691,2.69512135951845,3.36648936910842));
#59895=CARTESIAN_POINT('Ctrl Pts',(-3.00553721120534,0.325420867793348,
3.52450000696191));
#59896=CARTESIAN_POINT('Ctrl Pts',(-1.91460127455499,-2.33954154064343,
3.68251064481541));
#59897=CARTESIAN_POINT('Ctrl Pts',(0.913496948620389,-2.88178347497167,
3.8405212826689));
#59898=CARTESIAN_POINT('Ctrl Pts',(2.91275813454249,-0.809316203635805,
3.9985319205224));
#59899=CARTESIAN_POINT('Ctrl Pts',(2.26920608762133,1.99746249001107,4.15654255837589));
#59900=CARTESIAN_POINT('Ctrl Pts',(-0.433249444766719,2.99189698806592,
4.31455319622939));
#59901=CARTESIAN_POINT('Ctrl Pts',(-2.7426076746749,1.27171372987236,4.47256383408288));
#59902=CARTESIAN_POINT('Ctrl Pts',(-2.56353414341794,-1.60232498683304,
4.63057447193638));
#59903=CARTESIAN_POINT('Ctrl Pts',(-0.0585064328286764,-3.02253695848627,
4.78858510978987));
#59904=CARTESIAN_POINT('Ctrl Pts',(2.49960552566482,-1.70033081606459,4.94659574764337));
#59905=CARTESIAN_POINT('Ctrl Pts',(2.78976722724991,1.16462504084395,5.10460638549686));
#59906=CARTESIAN_POINT('Ctrl Pts',(0.548708208296067,2.97288949847998,5.26261702335036));
#59907=CARTESIAN_POINT('Ctrl Pts',(-2.19020653596968,2.08378213779743,5.42062766120385));
#59908=CARTESIAN_POINT('Ctrl Pts',(-2.9418959261048,-0.69598924415404,5.57863829905735));
#59909=CARTESIAN_POINT('Ctrl Pts',(-1.02433468733615,-2.84427338987187,
5.73664893691084));
#59910=CARTESIAN_POINT('Ctrl Pts',(1.82262924855683,-2.41188210539321,5.89465957476434));
#59911=CARTESIAN_POINT('Ctrl Pts',(3.01587925636697,0.20886593553466,6.05267021261782));
#59912=CARTESIAN_POINT('Ctrl Pts',(1.4727518382037,2.6401050530385,6.21068085047133));
#59913=CARTESIAN_POINT('Ctrl Pts',(-1.40663759231093,2.67591542316066,6.36869148832481));
#59914=CARTESIAN_POINT('Ctrl Pts',(-3.009752004189,0.283805463815948,6.52670212617831));
#59915=CARTESIAN_POINT('Ctrl Pts',(-1.88204838857008,-2.36580779673504,
6.68471276403181));
#59916=CARTESIAN_POINT('Ctrl Pts',(0.953281523493066,-2.8688685931876,6.8427234018853));
#59917=CARTESIAN_POINT('Ctrl Pts',(2.92367692732715,-0.76893815916913,7.0007340397388));
#59918=CARTESIAN_POINT('Ctrl Pts',(2.24135222378701,2.02866775913074,7.15874467759229));
#59919=CARTESIAN_POINT('Ctrl Pts',(-0.474603506551743,2.98561621438193,
7.31675531544579));
#59920=CARTESIAN_POINT('Ctrl Pts',(-2.7599404318192,1.23364560584519,7.47476595329927));
#59921=CARTESIAN_POINT('Ctrl Pts',(-2.54111918208094,-1.63764036664702,
7.63277659115279));
#59922=CARTESIAN_POINT('Ctrl Pts',(-0.0166813689890152,-3.02305712813042,
7.79078722900626));
#59923=CARTESIAN_POINT('Ctrl Pts',(2.5228918383464,-1.66558381356707,7.94879786685977));
#59924=CARTESIAN_POINT('Ctrl Pts',(2.77338657543163,1.20311245161337,8.10680850471326));
#59925=CARTESIAN_POINT('Ctrl Pts',(0.507523138532463,2.98019679415063,8.26481914256676));
#59926=CARTESIAN_POINT('Ctrl Pts',(-2.21882785154296,2.05327923898061,8.42282978042025));
#59927=CARTESIAN_POINT('Ctrl Pts',(-2.93198470187773,-0.736626347591836,
8.58084041827374));
#59928=CARTESIAN_POINT('Ctrl Pts',(-0.984883607674447,-2.85817370839241,
8.73885105612724));
#59929=CARTESIAN_POINT('Ctrl Pts',(1.85582530108642,-2.38643355655653,8.89686169398072));
#59930=CARTESIAN_POINT('Ctrl Pts',(3.01270073086355,0.250573291205824,9.05487233183424));
#59931=CARTESIAN_POINT('Ctrl Pts',(1.43608268481777,2.66022916125249,9.2128829696877));
#59932=CARTESIAN_POINT('Ctrl Pts',(-1.44352659745559,2.65619721226602,9.37089360754124));
#59933=CARTESIAN_POINT('Ctrl Pts',(-3.01339060835223,0.242135725381516,
9.5289042453947));
#59934=CARTESIAN_POINT('Ctrl Pts',(-1.84913520152769,-2.39162113941206,
9.68691488324822));
#59935=CARTESIAN_POINT('Ctrl Pts',(0.992883601278639,-2.8554044936442,9.8449255211017));
#59936=CARTESIAN_POINT('Ctrl Pts',(2.93403600917798,-0.728412908217918,
10.0029361589552));
#59937=CARTESIAN_POINT('Ctrl Pts',(2.21306927369375,2.05948465831726,10.1609467968087));
#59938=CARTESIAN_POINT('Ctrl Pts',(-0.515866709851859,2.9787638720916,10.3189574346622));
#59939=CARTESIAN_POINT('Ctrl Pts',(-2.77674482381607,1.19534131168557,10.4769680725157));
#59940=CARTESIAN_POINT('Ctrl Pts',(-2.51821774689341,-1.67264223528003,
10.6349787103692));
#59941=CARTESIAN_POINT('Ctrl Pts',(0.025146888342429,-3.02299856136555,
10.7929893482227));
#59942=CARTESIAN_POINT('Ctrl Pts',(2.54569516664075,-1.63051795039287,10.9509999860762));
#59943=CARTESIAN_POINT('Ctrl Pts',(2.75647498431545,1.24136953758929,11.1090106239297));
#59944=CARTESIAN_POINT('Ctrl Pts',(0.466240908142281,2.98693355861595,11.2670212617832));
#59945=CARTESIAN_POINT('Ctrl Pts',(-2.24702439297549,2.02238325877779,11.4250318996367));
#59946=CARTESIAN_POINT('Ctrl Pts',(-2.92151217620389,-0.777122430704416,
11.5830425374901));
#59947=CARTESIAN_POINT('Ctrl Pts',(-0.945243981123939,-2.87152685590094,
11.7410531753436));
#59948=CARTESIAN_POINT('Ctrl Pts',(1.88866607296754,-2.36052814701141,11.8990638131971));
#59949=CARTESIAN_POINT('Ctrl Pts',(3.00894545157365,0.292232676929939,12.0570744510506));
#59950=CARTESIAN_POINT('Ctrl Pts',(1.39913860663847,2.67984399311315,12.2150850889041));
#59951=CARTESIAN_POINT('Ctrl Pts',(-1.48013925273846,2.63597049689789,12.3730957267576));
#59952=CARTESIAN_POINT('Ctrl Pts',(-3.01645232665815,0.20041963229373,12.5311063646111));
#59953=CARTESIAN_POINT('Ctrl Pts',(-1.81586801459506,-2.41697662826485,
12.6891170024646));
#59954=CARTESIAN_POINT('Ctrl Pts',(1.03229560065101,-2.84139375323108,12.8471276403181));
#59955=CARTESIAN_POINT('Ctrl Pts',(2.94383339687692,-0.687748209325603,
13.0051382781716));
#59956=CARTESIAN_POINT('Ctrl Pts',(2.18436265188878,2.08990728814137,13.1631489160251));
#59957=CARTESIAN_POINT('Ctrl Pts',(-0.557031155230083,2.97134127292723,
13.3211595538786));
#59958=CARTESIAN_POINT('Ctrl Pts',(-2.79301763360067,1.15680818042351,13.4791701917321));
#59959=CARTESIAN_POINT('Ctrl Pts',(-2.49483422214693,-1.70732389192444,
13.6371808295856));
#59960=CARTESIAN_POINT('Ctrl Pts',(0.0669703315680426,-3.02236126948423,
13.7951914674391));
#59961=CARTESIAN_POINT('Ctrl Pts',(2.56801114499415,-1.59513993940493,13.9532021052926));
#59962=CARTESIAN_POINT('Ctrl Pts',(2.73903569159509,1.27938897446365,14.1112127431461));
#59963=CARTESIAN_POINT('Ctrl Pts',(0.424869419989396,2.99309850284224,14.2692233809996));
#59964=CARTESIAN_POINT('Ctrl Pts',(-2.27479076184412,1.99110011068065,14.427234018853));
#59965=CARTESIAN_POINT('Ctrl Pts',(-2.91048035482084,-0.817469738484123,
14.5852446567066));
#59966=CARTESIAN_POINT('Ctrl Pts',(-0.905423394666194,-2.88433028065578,
14.74325529456));
#59967=CARTESIAN_POINT('Ctrl Pts',(1.92114527396783,-2.33417082733325,14.9012659324135));
#59968=CARTESIAN_POINT('Ctrl Pts',(3.00461414346351,0.333836100640218,15.059276570267));
#59969=CARTESIAN_POINT('Ctrl Pts',(1.36192666470986,2.69894582555237,15.2172872081205));
#59970=CARTESIAN_POINT('Ctrl Pts',(-1.51646852692866,2.61523908814117,15.375297845974));
#59971=CARTESIAN_POINT('Ctrl Pts',(-3.01893661512828,0.158665287465281,
15.5333084838275));
#59972=CARTESIAN_POINT('Ctrl Pts',(-1.78225311595362,-2.44186963218761,
15.691319121681));
#59973=CARTESIAN_POINT('Ctrl Pts',(1.07150982278044,-2.82683862835414,15.8493297595345));
#59974=CARTESIAN_POINT('Ctrl Pts',(2.95306750846284,-0.646952660598369,
16.007340397388));
#59975=CARTESIAN_POINT('Ctrl Pts',(2.15523729316758,2.11993137754977,16.1653510352415));
#59976=CARTESIAN_POINT('Ctrl Pts',(-0.598087891085528,2.96334687184014,
16.323361673095));
#59977=CARTESIAN_POINT('Ctrl Pts',(-2.8087577913569,1.11805925334627,16.4813723109485));
#59978=CARTESIAN_POINT('Ctrl Pts',(-2.47096917801914,-1.74168951499088,
16.639382948802));
#59979=CARTESIAN_POINT('Ctrl Pts',(0.108773493647311,-3.02112471469761,
16.7973935866555));
#59980=CARTESIAN_POINT('Ctrl Pts',(2.58984974880435,-1.55949600909948,16.955404224509));
#59981=CARTESIAN_POINT('Ctrl Pts',(2.72104482603472,1.3172388360351,17.1134148623625));
#59982=CARTESIAN_POINT('Ctrl Pts',(0.383468559809897,2.9985465350827,17.271425500216));
#59983=CARTESIAN_POINT('Ctrl Pts',(-2.30222089225249,1.95971067011992,17.4294361380694));
#59984=CARTESIAN_POINT('Ctrl Pts',(-2.89870174257858,-0.858185938282932,
17.5874467759229));
#59985=CARTESIAN_POINT('Ctrl Pts',(-0.86579212814317,-2.89557444577305,
17.7454574137764));
#59986=CARTESIAN_POINT('Ctrl Pts',(1.95395413798184,-2.30932269903549,17.9034680516299));
#59987=CARTESIAN_POINT('Ctrl Pts',(2.99833212643718,0.37939948075128,18.0614786894834));
#59988=CARTESIAN_POINT('Ctrl Pts',(1.88447618126766,1.93145342515318,18.1668191147191));
#59989=CARTESIAN_POINT('Ctrl Pts',(1.12236674703438,2.30288577939273,18.2194893273369));
#59990=CARTESIAN_POINT('Ctrl Pts',(1.37702479013102,-1.93106208855765,-4.44089209850063E-15));
#59991=CARTESIAN_POINT('Ctrl Pts',(2.01608411688934,-1.47535404036748,0.0526702126178271));
#59992=CARTESIAN_POINT('Ctrl Pts',(2.79574737452458,0.112154857826279,0.15801063785349));
#59993=CARTESIAN_POINT('Ctrl Pts',(1.43092122672701,2.40744480175264,0.316021275706985));
#59994=CARTESIAN_POINT('Ctrl Pts',(-1.23339961524159,2.5114765043851,0.47403191356048));
#59995=CARTESIAN_POINT('Ctrl Pts',(-2.77800434033211,0.340253899408475,
0.632042551413975));
#59996=CARTESIAN_POINT('Ctrl Pts',(-1.80238813794495,-2.14148602308083,
0.790053189267469));
#59997=CARTESIAN_POINT('Ctrl Pts',(0.80874805201177,-2.67926694285025,0.948063827120964));
#59998=CARTESIAN_POINT('Ctrl Pts',(2.68599862008771,-0.786578017594937,
1.10607446497446));
#59999=CARTESIAN_POINT('Ctrl Pts',(2.12622710642163,1.82004872489232,1.26408510282796));
#60000=CARTESIAN_POINT('Ctrl Pts',(-0.362744329120993,2.775168194831,1.42209574068145));
#60001=CARTESIAN_POINT('Ctrl Pts',(-2.52257651676268,1.21238352457748,1.58010637853494));
#60002=CARTESIAN_POINT('Ctrl Pts',(-2.39362307562467,-1.45046186395561,
1.73811701638844));
#60003=CARTESIAN_POINT('Ctrl Pts',(-0.0928761899139844,-2.79725011229448,
1.89612765424193));
#60004=CARTESIAN_POINT('Ctrl Pts',(2.29213757529781,-1.60603837127393,2.05413829209543));
#60005=CARTESIAN_POINT('Ctrl Pts',(2.59744255060163,1.04237465766208,2.21214892994892));
#60006=CARTESIAN_POINT('Ctrl Pts',(0.546026952813309,2.74501412804214,2.37015956780242));
#60007=CARTESIAN_POINT('Ctrl Pts',(-2.00081133937873,1.95703986003066,2.52817020565591));
#60008=CARTESIAN_POINT('Ctrl Pts',(-2.73226708533368,-0.606602972742087,
2.68618084350941));
#60009=CARTESIAN_POINT('Ctrl Pts',(-0.984673254710223,-2.61986041464368,
2.8441914813629));
#60010=CARTESIAN_POINT('Ctrl Pts',(1.65633749422688,-2.25605774937986,3.0022021192164));
#60011=CARTESIAN_POINT('Ctrl Pts',(2.79451471318987,0.154718717530414,3.16021275706989));
#60012=CARTESIAN_POINT('Ctrl Pts',(1.39716369670102,2.42511523463794,3.31822339492339));
#60013=CARTESIAN_POINT('Ctrl Pts',(-1.2678664470183,2.49514829917553,3.47623403277688));
#60014=CARTESIAN_POINT('Ctrl Pts',(-2.78253186416353,0.301275236427873,
3.63424467063038));
#60015=CARTESIAN_POINT('Ctrl Pts',(-1.77254137255575,-2.16595185050593,
3.79225530848387));
#60016=CARTESIAN_POINT('Ctrl Pts',(0.845717150955885,-2.66796042811686,
3.95026594633737));
#60017=CARTESIAN_POINT('Ctrl Pts',(2.69663682477438,-0.749266426116641,
4.10827658419086));
#60018=CARTESIAN_POINT('Ctrl Pts',(2.10083515905894,1.84925443784418,4.26628722204435));
#60019=CARTESIAN_POINT('Ctrl Pts',(-0.401103130814736,2.76990372055638,
4.42429785989785));
#60020=CARTESIAN_POINT('Ctrl Pts',(-2.53911121686691,1.17735490423188,4.58230849775134));
#60021=CARTESIAN_POINT('Ctrl Pts',(-2.37332461309666,-1.48343541247336,
4.74031913560484));
#60022=CARTESIAN_POINT('Ctrl Pts',(-0.054165362850041,-2.79827026138436,
4.89832977345834));
#60023=CARTESIAN_POINT('Ctrl Pts',(2.3141393814959,-1.57416938897968,5.05634041131182));
#60024=CARTESIAN_POINT('Ctrl Pts',(2.58277161716087,1.07821199946199,5.21435104916533));
#60025=CARTESIAN_POINT('Ctrl Pts',(0.50799506591352,2.75230655182614,5.37236168701881));
#60026=CARTESIAN_POINT('Ctrl Pts',(-2.02769722920544,1.92916932612881,5.53037232487232));
#60027=CARTESIAN_POINT('Ctrl Pts',(-2.72361264565964,-0.644348119116159,
5.6883829627258));
#60028=CARTESIAN_POINT('Ctrl Pts',(-0.948330932804408,-2.6332335225146,
5.84639360057931));
#60029=CARTESIAN_POINT('Ctrl Pts',(1.68739350215265,-2.23292487806895,6.00440423843279));
#60030=CARTESIAN_POINT('Ctrl Pts',(2.79210654854793,0.193368466308401,6.1624148762863));
#60031=CARTESIAN_POINT('Ctrl Pts',(1.3634763537543,2.4442141017022,6.32042551413978));
#60032=CARTESIAN_POINT('Ctrl Pts',(-1.30226766361206,2.47736740805983,6.47843615199329));
#60033=CARTESIAN_POINT('Ctrl Pts',(-2.78643392724037,0.262747619076987,
6.63644678984677));
#60034=CARTESIAN_POINT('Ctrl Pts',(-1.74240385098862,-2.19026919858423,
6.79445742770028));
#60035=CARTESIAN_POINT('Ctrl Pts',(0.882549783362729,-2.65600380686722,
6.95246806555376));
#60036=CARTESIAN_POINT('Ctrl Pts',(2.70674546316629,-0.711884358470874,
7.11047870340726));
#60037=CARTESIAN_POINT('Ctrl Pts',(2.07504800081977,1.87814433324509,7.26848934126075));
#60038=CARTESIAN_POINT('Ctrl Pts',(-0.439388797084447,2.76408896875688,
7.42649997911426));
#60039=CARTESIAN_POINT('Ctrl Pts',(-2.5551579152302,1.14211136516684,7.58451061696773));
#60040=CARTESIAN_POINT('Ctrl Pts',(-2.35257280076785,-1.51613045589557,
7.74252125482125));
#60041=CARTESIAN_POINT('Ctrl Pts',(-0.0154436420140344,-2.79875183539522,
7.90053189267472));
#60042=CARTESIAN_POINT('Ctrl Pts',(2.33569789249813,-1.54200055031981,8.05854253052824));
#60043=CARTESIAN_POINT('Ctrl Pts',(2.56760637965517,1.11384371496224,8.21655316838172));
#60044=CARTESIAN_POINT('Ctrl Pts',(0.469865852767273,2.75907165956415,8.37456380623522));
#60045=CARTESIAN_POINT('Ctrl Pts',(-2.05419489567252,1.90092968644286,8.53257444408872));
#60046=CARTESIAN_POINT('Ctrl Pts',(-2.71443681608685,-0.681970024032665,
8.69058508194221));
#60047=CARTESIAN_POINT('Ctrl Pts',(-0.911807050875725,-2.64610246290276,
8.8485957197957));
#60048=CARTESIAN_POINT('Ctrl Pts',(1.7181264684868,-2.20936456486744,9.0066063576492));
#60049=CARTESIAN_POINT('Ctrl Pts',(2.78916386380546,0.231981212706065,9.16461699550269));
#60050=CARTESIAN_POINT('Ctrl Pts',(1.32952798427551,2.46284503800688,9.32262763335619));
#60051=CARTESIAN_POINT('Ctrl Pts',(-1.33641957225244,2.45911225223807,9.48063827120967));
#60052=CARTESIAN_POINT('Ctrl Pts',(-2.78980255365015,0.224169698786106,
9.63864890906318));
#60053=CARTESIAN_POINT('Ctrl Pts',(-1.71193276204147,-2.21416723859239,
9.79665954691667));
#60054=CARTESIAN_POINT('Ctrl Pts',(0.919213459631522,-2.64353871880838,
9.95467018477016));
#60055=CARTESIAN_POINT('Ctrl Pts',(2.71633592014881,-0.674366006791661,
10.1126808226237));
#60056=CARTESIAN_POINT('Ctrl Pts',(2.04886359373486,1.90667467504938,10.2706914604772));
#60057=CARTESIAN_POINT('Ctrl Pts',(-0.477590346402141,2.75774505769302,
10.4287020983307));
#60058=CARTESIAN_POINT('Ctrl Pts',(-2.57071545217063,1.10664917935991,10.5867127361841));
#60059=CARTESIAN_POINT('Ctrl Pts',(-2.33137061005572,-1.54853525009127,
10.7447233740376));
#60060=CARTESIAN_POINT('Ctrl Pts',(0.0232810353625256,-2.79869761417686,
10.9027340118911));
#60061=CARTESIAN_POINT('Ctrl Pts',(2.35680925566857,-1.50953650986048,11.0607446497446));
#60062=CARTESIAN_POINT('Ctrl Pts',(2.5519495975734,1.1492621953461,11.2187552875981));
#60063=CARTESIAN_POINT('Ctrl Pts',(0.431646688134689,2.76530856846557,11.3767659254516));
#60064=CARTESIAN_POINT('Ctrl Pts',(-2.0802993054608,1.8723261312886,11.5347765633051));
#60065=CARTESIAN_POINT('Ctrl Pts',(-2.70474133260486,-0.719461372073362,
11.6927872011586));
#60066=CARTESIAN_POINT('Ctrl Pts',(-0.875108611891469,-2.65846483136416,
11.8507978390121));
#60067=CARTESIAN_POINT('Ctrl Pts',(1.7485305153448,-2.18538128918389,12.0088084768656));
#60068=CARTESIAN_POINT('Ctrl Pts',(2.78568721934935,0.270549548438745,12.1668191147191));
#60069=CARTESIAN_POINT('Ctrl Pts',(1.29532508891864,2.48100448532931,12.3248297525726));
#60070=CARTESIAN_POINT('Ctrl Pts',(-1.37031563568376,2.44038632204184,12.4828403904261));
#60071=CARTESIAN_POINT('Ctrl Pts',(-2.79263709807487,0.1855488632721,12.6408510282796));
#60072=CARTESIAN_POINT('Ctrl Pts',(-1.68113393934647,-2.23764139669008,
12.7988616661331));
#60073=CARTESIAN_POINT('Ctrl Pts',(0.955701160956647,-2.63056754962948,
12.9568723039866));
#60074=CARTESIAN_POINT('Ctrl Pts',(2.725406359655,-0.636718553952737,13.1148829418401));
#60075=CARTESIAN_POINT('Ctrl Pts',(2.02228695060197,1.93484000155462,13.2728935796935));
#60076=CARTESIAN_POINT('Ctrl Pts',(-0.515700465454569,2.75087320176898,
13.4309042175471));
#60077=CARTESIAN_POINT('Ctrl Pts',(-2.5857808493237,1.07097513574369,13.5889148554005));
#60078=CARTESIAN_POINT('Ctrl Pts',(-2.30972209994545,-1.58064359144045,
13.746925493254));
#60079=CARTESIAN_POINT('Ctrl Pts',(0.0620012558310767,-2.79810760818394,
13.9049361311075));
#60080=CARTESIAN_POINT('Ctrl Pts',(2.37746942936956,-1.4767834823825,14.062946768961));
#60081=CARTESIAN_POINT('Ctrl Pts',(2.53580426837836,1.18446065975573,14.2209574068145));
#60082=CARTESIAN_POINT('Ctrl Pts',(0.393344888501637,2.77101608514062,14.378968044668));
#60083=CARTESIAN_POINT('Ctrl Pts',(-2.10600546070022,1.84336413538746,14.5369786825215));
#60084=CARTESIAN_POINT('Ctrl Pts',(-2.69452805212919,-0.756814983637939,
14.694989320375));
#60085=CARTESIAN_POINT('Ctrl Pts',(-0.838242639893101,-2.67031826549166,
14.8529999582285));
#60086=CARTESIAN_POINT('Ctrl Pts',(1.77859981921798,-2.16097963427009,15.011010596082));
#60087=CARTESIAN_POINT('Ctrl Pts',(2.78167728635466,0.309066074436347,15.1690212339355));
#60088=CARTESIAN_POINT('Ctrl Pts',(1.26087420481122,2.49868899684622,15.327031871789));
#60089=CARTESIAN_POINT('Ctrl Pts',(-1.40394934437959,2.42119314578055,15.4850425096425));
#60090=CARTESIAN_POINT('Ctrl Pts',(-2.79493705689825,0.146892614226416,
15.643053147496));
#60091=CARTESIAN_POINT('Ctrl Pts',(-1.65001320451353,-2.26068738539107,
15.8010637853495));
#60092=CARTESIAN_POINT('Ctrl Pts',(0.992005759747417,-2.61709238831523,
15.959074423203));
#60093=CARTESIAN_POINT('Ctrl Pts',(2.73395531710238,-0.598949960096589,
16.1170850610565));
#60094=CARTESIAN_POINT('Ctrl Pts',(1.99532264006382,1.96263635861182,16.2750956989099));
#60095=CARTESIAN_POINT('Ctrl Pts',(-0.553710866833194,2.74347197057582,
16.4331063367635));
#60096=CARTESIAN_POINT('Ctrl Pts',(-2.60035311625168,1.03510130796588,16.5911169746169));
#60097=CARTESIAN_POINT('Ctrl Pts',(-2.28762779830857,-1.61245934832335,
16.7491276124704));
#60098=CARTESIAN_POINT('Ctrl Pts',(0.100702699977133,-2.79696280349387,
16.9071382503239));
#60099=CARTESIAN_POINT('Ctrl Pts',(2.39768764884266,-1.44378426631252,17.0651488881774));
#60100=CARTESIAN_POINT('Ctrl Pts',(2.51914829203609,1.21950213103884,17.2231595260309));
#60101=CARTESIAN_POINT('Ctrl Pts',(0.35501589619246,2.77605988338393,17.3811701638844));
#60102=CARTESIAN_POINT('Ctrl Pts',(-2.13140032575625,1.81430373372853,17.5391808017379));
#60103=CARTESIAN_POINT('Ctrl Pts',(-2.68362339130599,-0.79451011611058,
17.6971914395914));
#60104=CARTESIAN_POINT('Ctrl Pts',(-0.801551940637627,-2.68072813418604,
17.8552020774449));
#60105=CARTESIAN_POINT('Ctrl Pts',(1.80897432571407,-2.13797519150506,18.0132127152984));
#60106=CARTESIAN_POINT('Ctrl Pts',(2.77586138346654,0.351248735334821,18.1712233531519));
#60107=CARTESIAN_POINT('Ctrl Pts',(1.74465150592214,1.78814312449695,18.2765637783876));
#60108=CARTESIAN_POINT('Ctrl Pts',(1.03908919352497,2.13201587949049,18.3292339910054));
#60109=CARTESIAN_POINT('',(1.28892185405319,2.64462557919719,18.));
#60110=CARTESIAN_POINT('Ctrl Pts',(1.37994918219943,-1.93347698736447,18.));
#60111=CARTESIAN_POINT('Ctrl Pts',(1.43821237480841,-1.90182406103466,18.));
#60112=CARTESIAN_POINT('Ctrl Pts',(1.49490500816213,-1.86766989359623,18.));
#60113=CARTESIAN_POINT('Ctrl Pts',(1.54984605587159,-1.83106249366945,18.));
#60114=CARTESIAN_POINT('Ctrl Pts',(1.61731929964478,-1.78610485048391,18.));
#60115=CARTESIAN_POINT('Ctrl Pts',(1.68215209723072,-1.73744909575843,18.));
#60116=CARTESIAN_POINT('Ctrl Pts',(1.74427143803024,-1.68546230453832,18.));
#60117=CARTESIAN_POINT('Ctrl Pts',(1.80797414842667,-1.63215041386288,18.));
#60118=CARTESIAN_POINT('Ctrl Pts',(1.86882386541983,-1.57533510126562,18.));
#60119=CARTESIAN_POINT('Ctrl Pts',(1.92672152516503,-1.51536150307498,18.));
#60120=CARTESIAN_POINT('Ctrl Pts',(1.95606151098823,-1.48496952301181,18.));
#60121=CARTESIAN_POINT('Ctrl Pts',(1.98464303190203,-1.45376573183374,18.));
#60122=CARTESIAN_POINT('Ctrl Pts',(2.01245056612922,-1.42179081892014,18.));
#60123=CARTESIAN_POINT('Ctrl Pts',(2.02687703313248,-1.40520232810643,18.));
#60124=CARTESIAN_POINT('Ctrl Pts',(2.04109514957463,-1.38840624663065,18.));
#60125=CARTESIAN_POINT('Ctrl Pts',(2.05510252968955,-1.37140799562356,18.));
#60126=CARTESIAN_POINT('Ctrl Pts',(2.06569873728338,-1.35854927436908,18.));
#60127=CARTESIAN_POINT('Ctrl Pts',(2.07617434762788,-1.34557485760829,18.));
#60128=CARTESIAN_POINT('Ctrl Pts',(2.08652826676332,-1.33248703035156,18.));
#60129=CARTESIAN_POINT('Ctrl Pts',(2.094783223847,-1.32205238711072,18.));
#60130=CARTESIAN_POINT('Ctrl Pts',(2.10295512158607,-1.31155284675917,18.));
#60131=CARTESIAN_POINT('Ctrl Pts',(2.11104243361189,-1.30099155085768,18.));
#60132=CARTESIAN_POINT('Ctrl Pts',(2.16374871732536,-1.23216192534195,18.));
#60133=CARTESIAN_POINT('Ctrl Pts',(2.21288175146922,-1.16069122843785,18.));
#60134=CARTESIAN_POINT('Ctrl Pts',(2.25835597691573,-1.08697798281416,18.));
#60135=CARTESIAN_POINT('Ctrl Pts',(2.30474705699815,-1.01177852537899,18.));
#60136=CARTESIAN_POINT('Ctrl Pts',(2.34733092606907,-0.934244553946303,
18.));
#60137=CARTESIAN_POINT('Ctrl Pts',(2.38598791054104,-0.854752429497406,
18.));
#60138=CARTESIAN_POINT('Ctrl Pts',(2.42492705239859,-0.77468009191716,18.));
#60139=CARTESIAN_POINT('Ctrl Pts',(2.459882395318,-0.692620112126303,18.));
#60140=CARTESIAN_POINT('Ctrl Pts',(2.4906933080418,-0.608921153989719,18.));
#60141=CARTESIAN_POINT('Ctrl Pts',(2.50574535552365,-0.568031722918762,
18.));
#60142=CARTESIAN_POINT('Ctrl Pts',(2.51980765168383,-0.526750663351143,
18.));
#60143=CARTESIAN_POINT('Ctrl Pts',(2.53285748335047,-0.485116441218252,
18.));
#60144=CARTESIAN_POINT('Ctrl Pts',(2.53785250263207,-0.46918031670412,18.));
#60145=CARTESIAN_POINT('Ctrl Pts',(2.54269975128169,-0.453190051907574,
18.));
#60146=CARTESIAN_POINT('Ctrl Pts',(2.54739155306582,-0.437170317508783,
18.));
#60147=CARTESIAN_POINT('Ctrl Pts',(2.57317453750917,-0.349136640513436,
18.));
#60148=CARTESIAN_POINT('Ctrl Pts',(2.59431215770916,-0.260074846372698,
18.));
#60149=CARTESIAN_POINT('Ctrl Pts',(2.61068742566702,-0.170385934282095,
18.));
#60150=CARTESIAN_POINT('Ctrl Pts',(2.62702434602131,-0.08090705569159,18.));
#60151=CARTESIAN_POINT('Ctrl Pts',(2.63862173311556,0.00919691345965296,
18.));
#60152=CARTESIAN_POINT('Ctrl Pts',(2.64532217576655,0.0995580551948545,
18.));
#60153=CARTESIAN_POINT('Ctrl Pts',(2.65107284244143,0.177110663813041,18.));
#60154=CARTESIAN_POINT('Ctrl Pts',(2.65321597987867,0.254853522028482,18.));
#60155=CARTESIAN_POINT('Ctrl Pts',(2.65162313398611,0.332564201440169,18.));
#60156=CARTESIAN_POINT('Ctrl Pts',(2.65043785503477,0.390390782800784,18.));
#60157=CARTESIAN_POINT('Ctrl Pts',(2.64718329974002,0.448199763632709,18.));
#60158=CARTESIAN_POINT('Ctrl Pts',(2.64191416774207,0.505920012373682,18.));
#60159=CARTESIAN_POINT('Ctrl Pts',(2.64062763401441,0.520013234331792,18.));
#60160=CARTESIAN_POINT('Ctrl Pts',(2.63922066290764,0.534103822243259,18.));
#60161=CARTESIAN_POINT('Ctrl Pts',(2.63769493345068,0.548181951403584,18.));
#60162=CARTESIAN_POINT('Ctrl Pts',(2.62812387695765,0.636495491458,18.));
#60163=CARTESIAN_POINT('Ctrl Pts',(2.6139065437193,0.724124252500042,18.));
#60164=CARTESIAN_POINT('Ctrl Pts',(2.59532997065339,0.810806020554952,18.));
#60165=CARTESIAN_POINT('Ctrl Pts',(2.5752815789767,0.904355569819364,18.));
#60166=CARTESIAN_POINT('Ctrl Pts',(2.55015626103555,0.996802800692518,18.));
#60167=CARTESIAN_POINT('Ctrl Pts',(2.52025097354548,1.08782980267173,18.));
#60168=CARTESIAN_POINT('Ctrl Pts',(2.49271715414392,1.17163842795221,18.));
#60169=CARTESIAN_POINT('Ctrl Pts',(2.46113046092889,1.25424383150991,18.));
#60170=CARTESIAN_POINT('Ctrl Pts',(2.42567706973452,1.3353970388071,18.));
#60171=CARTESIAN_POINT('Ctrl Pts',(2.40983754709368,1.37165388254068,18.));
#60172=CARTESIAN_POINT('Ctrl Pts',(2.39322565968621,1.40762079193962,18.));
#60173=CARTESIAN_POINT('Ctrl Pts',(2.3758554027599,1.44327498917763,18.));
#60174=CARTESIAN_POINT('Ctrl Pts',(2.36243191962062,1.47082803675195,18.));
#60175=CARTESIAN_POINT('Ctrl Pts',(2.34855550772026,1.49819432663718,18.));
#60176=CARTESIAN_POINT('Ctrl Pts',(2.3342320039039,1.52536310987849,18.));
#60177=CARTESIAN_POINT('Ctrl Pts',(2.32544284172995,1.54203436888314,18.));
#60178=CARTESIAN_POINT('Ctrl Pts',(2.31648412915412,1.55863319919544,18.));
#60179=CARTESIAN_POINT('Ctrl Pts',(2.30736886637286,1.57513647613047,18.));
#60180=CARTESIAN_POINT('Ctrl Pts',(2.26079517697126,1.65945861938906,18.));
#60181=CARTESIAN_POINT('Ctrl Pts',(2.2100781528945,1.74140468208013,18.));
#60182=CARTESIAN_POINT('Ctrl Pts',(2.15547782018911,1.82066912257117,18.));
#60183=CARTESIAN_POINT('Ctrl Pts',(2.09852307134651,1.90335151801874,18.));
#60184=CARTESIAN_POINT('Ctrl Pts',(2.03734284105072,1.98311713055562,18.));
#60185=CARTESIAN_POINT('Ctrl Pts',(1.97217502405287,2.05960411713276,18.));
#60186=CARTESIAN_POINT('Ctrl Pts',(1.9509987109036,2.08445859982404,18.));
#60187=CARTESIAN_POINT('Ctrl Pts',(1.92940090651591,2.10896669670022,18.));
#60188=CARTESIAN_POINT('Ctrl Pts',(1.90738857169095,2.13311535773337,18.));
#60189=CARTESIAN_POINT('Ctrl Pts',(1.89181486376242,2.15020051461408,18.));
#60190=CARTESIAN_POINT('Ctrl Pts',(1.87603066798751,2.16710868538781,18.));
#60191=CARTESIAN_POINT('Ctrl Pts',(1.86005797891342,2.18381506371099,18.));
#60192=CARTESIAN_POINT('Ctrl Pts',(1.79161585954772,2.25540100231282,18.));
#60193=CARTESIAN_POINT('Ctrl Pts',(1.71965505267813,2.32335372378486,18.));
#60194=CARTESIAN_POINT('Ctrl Pts',(1.6444167588703,2.38734627880606,18.));
#60195=CARTESIAN_POINT('Ctrl Pts',(1.57011188953763,2.45054492670815,18.));
#60196=CARTESIAN_POINT('Ctrl Pts',(1.49260984581683,2.50988188571361,18.));
#60197=CARTESIAN_POINT('Ctrl Pts',(1.41210003131952,2.5650162920718,18.));
#60198=CARTESIAN_POINT('Ctrl Pts',(1.3717885747323,2.59262222114079,18.));
#60199=CARTESIAN_POINT('Ctrl Pts',(1.33072243200449,2.61917407343912,18.));
#60200=CARTESIAN_POINT('Ctrl Pts',(1.28892185405319,2.64462557919719,18.));
#60201=CARTESIAN_POINT('Ctrl Pts',(1.29200466145509,2.64817921559509,-6.24500451351651E-17));
#60202=CARTESIAN_POINT('Ctrl Pts',(1.36163579271623,2.60626235479205,-6.87923715339042E-17));
#60203=CARTESIAN_POINT('Ctrl Pts',(1.42923480273934,2.56138620404723,-2.42496828474002E-16));
#60204=CARTESIAN_POINT('Ctrl Pts',(1.49459025051858,2.51355282242146,-2.30718222304915E-16));
#60205=CARTESIAN_POINT('Ctrl Pts',(1.57240550431648,2.4566001603604,-2.24944840579866E-16));
#60206=CARTESIAN_POINT('Ctrl Pts',(1.6470415083937,2.3954556864035,-4.65838301304871E-16));
#60207=CARTESIAN_POINT('Ctrl Pts',(1.71834920131344,2.33049816358297,-4.78783679369599E-16));
#60208=CARTESIAN_POINT('Ctrl Pts',(1.79066277758345,2.26462433442851,-4.91911668029694E-16));
#60209=CARTESIAN_POINT('Ctrl Pts',(1.85955394539379,2.19482820959758,-1.96384928419704E-16));
#60210=CARTESIAN_POINT('Ctrl Pts',(1.92482290460833,2.12147584187517,-1.31838984174237E-16));
#60211=CARTESIAN_POINT('Ctrl Pts',(1.98558343594445,2.0531902603183,-7.17515258304525E-17));
#60212=CARTESIAN_POINT('Ctrl Pts',(2.0432046872693,1.98182185580739,-1.54434603693546E-16));
#60213=CARTESIAN_POINT('Ctrl Pts',(2.09748648009497,1.9076544835139,-1.2490009027033E-16));
#60214=CARTESIAN_POINT('Ctrl Pts',(2.10646567520803,1.89538585213349,-1.20014544955935E-16));
#60215=CARTESIAN_POINT('Ctrl Pts',(2.11535391066683,1.88303977945376,3.07879830521503E-17));
#60216=CARTESIAN_POINT('Ctrl Pts',(2.12414058888115,1.87063145433286,2.77555756156289E-17));
#60217=CARTESIAN_POINT('Ctrl Pts',(2.17962767318294,1.79227399486589,8.60619481851236E-18));
#60218=CARTESIAN_POINT('Ctrl Pts',(2.23116246589918,1.7113097095221,-9.20636394827646E-17));
#60219=CARTESIAN_POINT('Ctrl Pts',(2.27859496939366,1.62810410227917,-1.66533453693773E-16));
#60220=CARTESIAN_POINT('Ctrl Pts',(2.32587821025047,1.54516033001208,-2.40768923097373E-16));
#60221=CARTESIAN_POINT('Ctrl Pts',(2.36908523109373,1.45998835263573,-3.28642479298764E-16));
#60222=CARTESIAN_POINT('Ctrl Pts',(2.40801906757308,1.37293284166191,-3.05311331771918E-16));
#60223=CARTESIAN_POINT('Ctrl Pts',(2.44628350384463,1.28737410014124,-2.82381323110772E-16));
#60224=CARTESIAN_POINT('Ctrl Pts',(2.48042058153336,1.19999515723855,-3.78426003229508E-16));
#60225=CARTESIAN_POINT('Ctrl Pts',(2.5101934511382,1.11112005268495,-4.44089209850063E-16));
#60226=CARTESIAN_POINT('Ctrl Pts',(2.52374026722379,1.07068140125652,-4.73966322653916E-16));
#60227=CARTESIAN_POINT('Ctrl Pts',(2.53638285871564,1.02993303554646,-5.32472828915682E-16));
#60228=CARTESIAN_POINT('Ctrl Pts',(2.54809527872308,0.988905993523423,-5.68989300120393E-16));
#60229=CARTESIAN_POINT('Ctrl Pts',(2.55316374923826,0.971151818665729,-5.84791555973746E-16));
#60230=CARTESIAN_POINT('Ctrl Pts',(2.55805799988541,0.953345463647252,-1.91210667779528E-16));
#60231=CARTESIAN_POINT('Ctrl Pts',(2.56277579019384,0.935489479213339,-1.94289029309402E-16));
#60232=CARTESIAN_POINT('Ctrl Pts',(2.56650136447238,0.921388853289753,-1.96719969174464E-16));
#60233=CARTESIAN_POINT('Ctrl Pts',(2.57011697351366,0.907256657441779,-7.89089153153375E-16));
#60234=CARTESIAN_POINT('Ctrl Pts',(2.57361787574017,0.893109630455151,-7.91033905045424E-16));
#60235=CARTESIAN_POINT('Ctrl Pts',(2.59566788235011,0.804006302688932,-8.03282688159008E-16));
#60236=CARTESIAN_POINT('Ctrl Pts',(2.61321131606813,0.714168582471938,-3.64080492391637E-16));
#60237=CARTESIAN_POINT('Ctrl Pts',(2.62607387329613,0.623910106232047,-3.88578058618805E-16));
#60238=CARTESIAN_POINT('Ctrl Pts',(2.63856685923259,0.536244966685939,-4.1237175258874E-16));
#60239=CARTESIAN_POINT('Ctrl Pts',(2.64664407470688,0.448182150112304,-7.31559005160491E-16));
#60240=CARTESIAN_POINT('Ctrl Pts',(2.65009784347288,0.360011822186139,-7.21644966006352E-16));
#60241=CARTESIAN_POINT('Ctrl Pts',(2.65337342956238,0.276390271575919,-7.12242400014153E-16));
#60242=CARTESIAN_POINT('Ctrl Pts',(2.65249011193531,0.192671525761824,-5.49469972717259E-16));
#60243=CARTESIAN_POINT('Ctrl Pts',(2.64722883229478,0.109114351042944,-5.55111512312578E-16));
#60244=CARTESIAN_POINT('Ctrl Pts',(2.64396837891794,0.0573333602792648,
-5.59772983305919E-16));
#60245=CARTESIAN_POINT('Ctrl Pts',(2.63902562983071,0.00561466852570915,
-5.84771322736047E-16));
#60246=CARTESIAN_POINT('Ctrl Pts',(2.63242939092862,-0.0459762644840405,
-6.38378239159465E-16));
#60247=CARTESIAN_POINT('Ctrl Pts',(2.63040459618663,-0.0618127209015484,
-6.54833525894753E-16));
#60248=CARTESIAN_POINT('Ctrl Pts',(2.62822397035665,-0.0776371160914911,
8.07626614741256E-17));
#60249=CARTESIAN_POINT('Ctrl Pts',(2.62588826970276,-0.0934474919564786,
8.32667268468867E-17));
#60250=CARTESIAN_POINT('Ctrl Pts',(2.62391430098318,-0.10680930154901,8.53829854990407E-17));
#60251=CARTESIAN_POINT('Ctrl Pts',(2.62182970872418,-0.120159705897083,
-4.668564614999E-16));
#60252=CARTESIAN_POINT('Ctrl Pts',(2.61963718019352,-0.133485486331073,
-4.71844785465692E-16));
#60253=CARTESIAN_POINT('Ctrl Pts',(2.60533107299951,-0.220435343843426,
-5.04393277480817E-16));
#60254=CARTESIAN_POINT('Ctrl Pts',(2.58641348004362,-0.30647879548521,-5.84701050508147E-16));
#60255=CARTESIAN_POINT('Ctrl Pts',(2.56311086331968,-0.391324698838268,
-5.55111512312578E-16));
#60256=CARTESIAN_POINT('Ctrl Pts',(2.5394147018448,-0.477603516799134,-5.25022253095215E-16));
#60257=CARTESIAN_POINT('Ctrl Pts',(2.51118363377731,-0.562644867046194,
-6.60463472264379E-16));
#60258=CARTESIAN_POINT('Ctrl Pts',(2.4786078639959,-0.646119795222761,-7.21644966006352E-16));
#60259=CARTESIAN_POINT('Ctrl Pts',(2.44637828472532,-0.728707615336435,
-7.82176269354827E-16));
#60260=CARTESIAN_POINT('Ctrl Pts',(2.40989517054765,-0.809762845613054,
-5.71017860423719E-16));
#60261=CARTESIAN_POINT('Ctrl Pts',(2.36930556806385,-0.888933046760586,
-5.27355936696949E-16));
#60262=CARTESIAN_POINT('Ctrl Pts',(2.35350849036712,-0.919745317447226,
-5.10363141515569E-16));
#60263=CARTESIAN_POINT('Ctrl Pts',(2.33708906017935,-0.950271642113999,
-7.68273519756434E-16));
#60264=CARTESIAN_POINT('Ctrl Pts',(2.32005473735486,-0.980489483259258,
-7.7715611723761E-16));
#60265=CARTESIAN_POINT('Ctrl Pts',(2.31145085630386,-0.995752239138126,
-7.81642636187581E-16));
#60266=CARTESIAN_POINT('Ctrl Pts',(2.30269009619025,-1.01093627868412,-4.6423720985487E-16));
#60267=CARTESIAN_POINT('Ctrl Pts',(2.2937733628843,-1.02603858919702,-4.71844785465692E-16));
#60268=CARTESIAN_POINT('Ctrl Pts',(2.28696334816895,-1.03757274114479,-4.77654951597187E-16));
#60269=CARTESIAN_POINT('Ctrl Pts',(2.28006336389062,-1.04905742084503,-5.28398787028243E-16));
#60270=CARTESIAN_POINT('Ctrl Pts',(2.27307868687177,-1.06048370824817,-5.27355936696949E-16));
#60271=CARTESIAN_POINT('Ctrl Pts',(2.22741873521752,-1.13517917791805,-5.20538657160472E-16));
#60272=CARTESIAN_POINT('Ctrl Pts',(2.17808663173844,-1.20747732680705,-1.22707103107793E-16));
#60273=CARTESIAN_POINT('Ctrl Pts',(2.12525032891489,-1.27705317933263,-2.22044604925031E-16));
#60274=CARTESIAN_POINT('Ctrl Pts',(2.07473473787799,-1.343573074261,-3.17018937879127E-16));
#60275=CARTESIAN_POINT('Ctrl Pts',(2.02101528324939,-1.40760489508775,-2.95247053471268E-16));
#60276=CARTESIAN_POINT('Ctrl Pts',(1.96421324888463,-1.46882687010891,-2.77555756156289E-16));
#60277=CARTESIAN_POINT('Ctrl Pts',(1.94502782179757,-1.4895051741702,-2.71580352308384E-16));
#60278=CARTESIAN_POINT('Ctrl Pts',(1.92549055386547,-1.5098625760957,9.78135150092519E-17));
#60279=CARTESIAN_POINT('Ctrl Pts',(1.90560563251692,-1.52988554447117,1.11022302462516E-16));
#60280=CARTESIAN_POINT('Ctrl Pts',(1.89094057784228,-1.54465240830875,1.20763733509313E-16));
#60281=CARTESIAN_POINT('Ctrl Pts',(1.87608371516564,-1.55923977942274,-4.05819302166216E-16));
#60282=CARTESIAN_POINT('Ctrl Pts',(1.86105586686576,-1.57362416245269,-4.44089209850063E-16));
#60283=CARTESIAN_POINT('Ctrl Pts',(1.80044928191378,-1.63163568311025,-5.98429895546516E-16));
#60284=CARTESIAN_POINT('Ctrl Pts',(1.73700660477931,-1.68640875868871,-1.11912723490306E-15));
#60285=CARTESIAN_POINT('Ctrl Pts',(1.67086281709221,-1.73762501202154,-1.99840144432528E-15));
#60286=CARTESIAN_POINT('Ctrl Pts',(1.60658766700043,-1.78739434766466,-2.85283515244317E-15));
#60287=CARTESIAN_POINT('Ctrl Pts',(1.53976127787681,-1.83380531528516,-3.83545286917222E-15));
#60288=CARTESIAN_POINT('Ctrl Pts',(1.47049014543338,-1.87652000934262,-4.38538094726937E-15));
#60289=CARTESIAN_POINT('Ctrl Pts',(1.43981185670265,-1.89543717831499,-4.62892904249903E-15));
#60290=CARTESIAN_POINT('Ctrl Pts',(1.40865388521069,-1.91362873361342,-4.4670584227815E-15));
#60291=CARTESIAN_POINT('Ctrl Pts',(1.37702479013102,-1.93106208855765,-4.44089209850063E-15));
#60292=CARTESIAN_POINT('Ctrl Pts',(1.28892185405319,2.64462557919719,18.));
#60293=CARTESIAN_POINT('Ctrl Pts',(2.16412553195871,2.21807402646564,17.9473297873822));
#60294=CARTESIAN_POINT('Ctrl Pts',(2.80369957216858,1.32688749902492,17.8946595747643));
#60295=CARTESIAN_POINT('Ctrl Pts',(2.92359328396334,0.366674454357809,17.8419893621465));
#60296=CARTESIAN_POINT('Ctrl Pts',(3.0434869957581,-0.593538590309304,17.7893191495287));
#60297=CARTESIAN_POINT('Ctrl Pts',(2.64370037913775,-1.62277815220282,17.7366489369109));
#60298=CARTESIAN_POINT('Ctrl Pts',(1.90410935988231,-2.24960615895804,17.683978724293));
#60299=CARTESIAN_POINT('Ctrl Pts',(1.16451834062685,-2.87643416571327,17.6313085116752));
#60300=CARTESIAN_POINT('Ctrl Pts',(0.0851229187362741,-3.10085061733018,
17.5786382990573));
#60301=CARTESIAN_POINT('Ctrl Pts',(-0.843672449203934,-2.82310392875205,
17.5259680864395));
#60302=CARTESIAN_POINT('Ctrl Pts',(-1.77246781714411,-2.54535724017392,
17.4732978738217));
#60303=CARTESIAN_POINT('Ctrl Pts',(-2.55066313113394,-1.76544741140077,
17.4206276612039));
#60304=CARTESIAN_POINT('Ctrl Pts',(-2.82559471814905,-0.836148809425809,
17.367957448586));
#60305=CARTESIAN_POINT('Ctrl Pts',(-2.90525222915565,-0.566897777127469,
17.3526970047539));
#60306=CARTESIAN_POINT('Ctrl Pts',(-2.94266235676508,-0.285106034186959,
17.3374365609218));
#60307=CARTESIAN_POINT('Ctrl Pts',(-2.94033980469539,-0.00268911818531531,
17.3221761170896));
#60308=CARTESIAN_POINT('Origin',(0.,0.,18.));
#60309=CARTESIAN_POINT('Origin',(0.,0.,18.));
#60310=CARTESIAN_POINT('Origin',(0.,0.,0.));
#60311=CARTESIAN_POINT('Origin',(0.,0.,0.));
#60312=CARTESIAN_POINT('',(0.,0.,0.));
#60313=CARTESIAN_POINT('Origin',(32.,-32.,4.));
#60314=CARTESIAN_POINT('',(28.,-32.,4.));
#60315=CARTESIAN_POINT('Origin',(32.,-32.,4.));
#60316=CARTESIAN_POINT('',(29.5,-32.,4.));
#60317=CARTESIAN_POINT('Origin',(32.,-32.,4.));
#60318=CARTESIAN_POINT('Origin',(32.,-32.,7.5));
#60319=CARTESIAN_POINT('',(28.,-32.,11.));
#60320=CARTESIAN_POINT('Origin',(32.,-32.,11.));
#60321=CARTESIAN_POINT('',(28.,-32.,7.5));
#60322=CARTESIAN_POINT('Origin',(32.,-32.,5.5));
#60323=CARTESIAN_POINT('',(29.5,-32.,0.));
#60324=CARTESIAN_POINT('',(29.5,-32.,5.5));
#60325=CARTESIAN_POINT('Origin',(32.,-32.,0.));
#60326=CARTESIAN_POINT('Origin',(-32.,-32.,4.));
#60327=CARTESIAN_POINT('',(-36.,-32.,4.));
#60328=CARTESIAN_POINT('Origin',(-32.,-32.,4.));
#60329=CARTESIAN_POINT('',(-34.5,-32.,4.));
#60330=CARTESIAN_POINT('Origin',(-32.,-32.,4.));
#60331=CARTESIAN_POINT('Origin',(-32.,-32.,7.5));
#60332=CARTESIAN_POINT('',(-36.,-32.,11.));
#60333=CARTESIAN_POINT('Origin',(-32.,-32.,11.));
#60334=CARTESIAN_POINT('',(-36.,-32.,7.5));
#60335=CARTESIAN_POINT('Origin',(-32.,-32.,5.5));
#60336=CARTESIAN_POINT('',(-34.5,-32.,0.));
#60337=CARTESIAN_POINT('',(-34.5,-32.,5.5));
#60338=CARTESIAN_POINT('Origin',(-32.,-32.,0.));
#60339=CARTESIAN_POINT('Origin',(-32.,32.,4.));
#60340=CARTESIAN_POINT('',(-36.,32.,4.));
#60341=CARTESIAN_POINT('Origin',(-32.,32.,4.));
#60342=CARTESIAN_POINT('',(-34.5,32.,4.));
#60343=CARTESIAN_POINT('Origin',(-32.,32.,4.));
#60344=CARTESIAN_POINT('Origin',(-32.,32.,7.5));
#60345=CARTESIAN_POINT('',(-36.,32.,11.));
#60346=CARTESIAN_POINT('Origin',(-32.,32.,11.));
#60347=CARTESIAN_POINT('',(-36.,32.,7.5));
#60348=CARTESIAN_POINT('Origin',(-32.,32.,5.5));
#60349=CARTESIAN_POINT('',(-34.5,32.,0.));
#60350=CARTESIAN_POINT('',(-34.5,32.,5.5));
#60351=CARTESIAN_POINT('Origin',(-32.,32.,0.));
#60352=CARTESIAN_POINT('Origin',(32.,32.,4.));
#60353=CARTESIAN_POINT('',(28.,32.,4.));
#60354=CARTESIAN_POINT('Origin',(32.,32.,4.));
#60355=CARTESIAN_POINT('',(29.5,32.,4.));
#60356=CARTESIAN_POINT('Origin',(32.,32.,4.));
#60357=CARTESIAN_POINT('Origin',(32.,32.,7.5));
#60358=CARTESIAN_POINT('',(28.,32.,11.));
#60359=CARTESIAN_POINT('Origin',(32.,32.,11.));
#60360=CARTESIAN_POINT('',(28.,32.,7.5));
#60361=CARTESIAN_POINT('Origin',(32.,32.,5.5));
#60362=CARTESIAN_POINT('',(29.5,32.,0.));
#60363=CARTESIAN_POINT('',(29.5,32.,5.5));
#60364=CARTESIAN_POINT('Origin',(32.,32.,0.));
#60365=CARTESIAN_POINT('Origin',(0.,0.,0.));
#60366=CARTESIAN_POINT('',(-28.,-3.42901103761259E-15,11.));
#60367=CARTESIAN_POINT('Origin',(0.,0.,11.));
#60368=CARTESIAN_POINT('',(-28.,-3.42901103761259E-15,0.));
#60369=CARTESIAN_POINT('',(-28.,-3.42901103761259E-15,0.));
#60370=CARTESIAN_POINT('Origin',(0.,0.,0.));
#60371=CARTESIAN_POINT('Origin',(0.,0.,0.));
#60372=CARTESIAN_POINT('',(-50.,-6.12323399573677E-15,11.));
#60373=CARTESIAN_POINT('Origin',(0.,0.,11.));
#60374=CARTESIAN_POINT('',(-50.,-6.12323399573677E-15,0.));
#60375=CARTESIAN_POINT('',(-50.,-6.12323399573677E-15,0.));
#60376=CARTESIAN_POINT('Origin',(0.,0.,0.));
#60377=CARTESIAN_POINT('Origin',(0.,0.,11.));
#60378=CARTESIAN_POINT('Origin',(0.,0.,0.));
#60379=CARTESIAN_POINT('',(0.,0.,0.));
#60380=CARTESIAN_POINT('Origin',(0.,0.,0.));
#60381=CARTESIAN_POINT('',(-27.5,-3.36777869765522E-15,4.87339717240448));
#60382=CARTESIAN_POINT('Origin',(0.,0.,4.87339717240448));
#60383=CARTESIAN_POINT('',(-27.5,3.36777869765522E-15,-4.87339717240448));
#60384=CARTESIAN_POINT('Origin',(-31.,-3.7964050773568E-15,0.));
#60385=CARTESIAN_POINT('Origin',(0.,0.,-4.87339717240448));
#60386=CARTESIAN_POINT('Origin',(0.,0.,-9.));
#60387=CARTESIAN_POINT('',(-27.5,-3.36777869765522E-15,-9.));
#60388=CARTESIAN_POINT('',(-27.5,-3.36777869765522E-15,-9.));
#60389=CARTESIAN_POINT('Origin',(0.,0.,-9.));
#60390=CARTESIAN_POINT('Origin',(0.,0.,-9.));
#60391=CARTESIAN_POINT('',(-20.,-2.44929359829471E-15,9.));
#60392=CARTESIAN_POINT('Origin',(0.,0.,9.));
#60393=CARTESIAN_POINT('',(-20.,-2.44929359829471E-15,-9.));
#60394=CARTESIAN_POINT('',(-20.,-2.44929359829471E-15,-9.));
#60395=CARTESIAN_POINT('Origin',(0.,0.,-9.));
#60396=CARTESIAN_POINT('Origin',(0.,0.,-9.));
#60397=CARTESIAN_POINT('',(-27.5,-3.36777869765522E-15,9.));
#60398=CARTESIAN_POINT('Origin',(0.,0.,9.));
#60399=CARTESIAN_POINT('',(-27.5,-3.36777869765522E-15,-9.));
#60400=CARTESIAN_POINT('Origin',(0.,0.,9.));
#60401=CARTESIAN_POINT('Origin',(0.,0.,-9.));
#60402=CARTESIAN_POINT('',(0.,0.,0.));
#60403=CARTESIAN_POINT('Origin',(0.,0.,0.));
#60404=CARTESIAN_POINT('',(-32.5,-3.9801020972289E-15,-4.87339717240448));
#60405=CARTESIAN_POINT('Origin',(0.,0.,-4.87339717240448));
#60406=CARTESIAN_POINT('',(-32.5,3.9801020972289E-15,4.87339717240448));
#60407=CARTESIAN_POINT('Origin',(-29.,-3.55147571752732E-15,0.));
#60408=CARTESIAN_POINT('Origin',(0.,0.,4.87339717240448));
#60409=CARTESIAN_POINT('Origin',(0.,0.,-9.));
#60410=CARTESIAN_POINT('',(-32.5,-3.9801020972289E-15,9.));
#60411=CARTESIAN_POINT('Origin',(0.,0.,9.));
#60412=CARTESIAN_POINT('',(-32.5,-3.9801020972289E-15,-9.));
#60413=CARTESIAN_POINT('Origin',(0.,0.,-9.));
#60414=CARTESIAN_POINT('',(-32.5,-3.9801020972289E-15,-9.));
#60415=CARTESIAN_POINT('',(-32.5,-3.9801020972289E-15,-9.));
#60416=CARTESIAN_POINT('Origin',(0.,0.,-9.));
#60417=CARTESIAN_POINT('Origin',(0.,0.,-9.));
#60418=CARTESIAN_POINT('',(-40.,-4.89858719658941E-15,9.));
#60419=CARTESIAN_POINT('Origin',(0.,0.,9.));
#60420=CARTESIAN_POINT('',(-40.,-4.89858719658941E-15,-9.));
#60421=CARTESIAN_POINT('',(-40.,-4.89858719658941E-15,-9.));
#60422=CARTESIAN_POINT('Origin',(0.,0.,-9.));
#60423=CARTESIAN_POINT('Origin',(0.,0.,9.));
#60424=CARTESIAN_POINT('Origin',(0.,0.,-9.));
#60425=CARTESIAN_POINT('',(0.,0.,0.));
#60426=CARTESIAN_POINT('Origin',(0.,0.,0.));
#60427=CARTESIAN_POINT('',(-3.06161699786838E-16,-3.74939945665464E-32,
5.));
#60428=CARTESIAN_POINT('',(-3.06161699786838E-16,-3.74939945665464E-32,
-5.));
#60429=CARTESIAN_POINT('Origin',(0.,0.,0.));
#60430=CARTESIAN_POINT('',(0.,0.,0.));
#60431=CARTESIAN_POINT('Origin',(25.9807621135332,-15.,0.));
#60432=CARTESIAN_POINT('',(24.3419428085142,-20.771851634051,0.));
#60433=CARTESIAN_POINT('',(30.1599226029865,-10.6948150326157,0.));
#60434=CARTESIAN_POINT('Ctrl Pts',(24.3419428085141,-20.771851634051,-5.55111512312578E-16));
#60435=CARTESIAN_POINT('Ctrl Pts',(24.3419428085141,-20.771851634051,0.650190448083162));
#60436=CARTESIAN_POINT('Ctrl Pts',(24.4227996788253,-20.6782577017963,1.34576815070429));
#60437=CARTESIAN_POINT('Ctrl Pts',(24.7453933436892,-20.2911063999427,2.63799288444813));
#60438=CARTESIAN_POINT('Ctrl Pts',(24.9861795488087,-19.9970150157524,3.23471700046071));
#60439=CARTESIAN_POINT('Ctrl Pts',(25.3750265832533,-19.4973595993855,3.93620747216805));
#60440=CARTESIAN_POINT('Ctrl Pts',(25.5173253431967,-19.3113833049334,4.15945687249389));
#60441=CARTESIAN_POINT('Ctrl Pts',(25.8180939601395,-18.9073912038163,4.56176656225471));
#60442=CARTESIAN_POINT('Ctrl Pts',(25.9764367690932,-18.6893185292651,4.74086471477472));
#60443=CARTESIAN_POINT('Ctrl Pts',(26.3690354996372,-18.1343047842461,5.12459397949762));
#60444=CARTESIAN_POINT('Ctrl Pts',(26.6450813997796,-17.7284768246621,5.32832509625205));
#60445=CARTESIAN_POINT('Ctrl Pts',(27.1956249100491,-16.8717882618769,5.59441429610713));
#60446=CARTESIAN_POINT('Ctrl Pts',(27.4698694309609,-16.4207904682926,5.65685424949238));
#60447=CARTESIAN_POINT('Ctrl Pts',(27.9557564112432,-15.5792095317074,5.65685424949238));
#60448=CARTESIAN_POINT('Ctrl Pts',(28.2092096970821,-15.116207912957,5.59441429610713));
#60449=CARTESIAN_POINT('Ctrl Pts',(28.6758520004508,-14.2110789657823,5.32832509625205));
#60450=CARTESIAN_POINT('Ctrl Pts',(28.8892863729454,-13.7691022238565,5.12459397949763));
#60451=CARTESIAN_POINT('Ctrl Pts',(29.1736430103094,-13.1515948772024,4.74086471477473));
#60452=CARTESIAN_POINT('Ctrl Pts',(29.2833280818651,-12.9054296448663,4.56176656225472));
#60453=CARTESIAN_POINT('Ctrl Pts',(29.4828111958893,-12.4429603313742,4.15945687249389));
#60454=CARTESIAN_POINT('Ctrl Pts',(29.5727220114149,-12.2267378431101,3.93620747216806));
#60455=CARTESIAN_POINT('Ctrl Pts',(29.8110127779048,-11.6401587249113,3.23471700046071));
#60456=CARTESIAN_POINT('Ctrl Pts',(29.945310285088,-11.2845860623018,2.63799288444813));
#60457=CARTESIAN_POINT('Ctrl Pts',(30.1192963151694,-10.811636102503,1.34576815070429));
#60458=CARTESIAN_POINT('Ctrl Pts',(30.1599226029865,-10.6948150326157,0.650190448083163));
#60459=CARTESIAN_POINT('Ctrl Pts',(30.1599226029865,-10.6948150326157,1.38777878078145E-16));
#60460=CARTESIAN_POINT('',(21.0673540166964,-18.4436057953749,0.));
#60461=CARTESIAN_POINT('Origin',(25.9807621135332,-15.,0.));
#60462=CARTESIAN_POINT('',(23.6431808351666,-14.9999999999269,5.52591293516556));
#60463=CARTESIAN_POINT('Ctrl Pts',(23.6431808351666,-14.9999999998537,5.52591293516556));
#60464=CARTESIAN_POINT('Ctrl Pts',(23.6009406541951,-15.0665794823356,5.50804442051787));
#60465=CARTESIAN_POINT('Ctrl Pts',(23.5585526426266,-15.1327690152579,5.48833637748936));
#60466=CARTESIAN_POINT('Ctrl Pts',(23.2618588909767,-15.5918378185285,5.3379209922756));
#60467=CARTESIAN_POINT('Ctrl Pts',(23.0071885556824,-15.9630484519639,5.14122028307955));
#60468=CARTESIAN_POINT('Ctrl Pts',(22.5419616872921,-16.6141770101942,4.66899487999358));
#60469=CARTESIAN_POINT('Ctrl Pts',(22.3089325549727,-16.9242282724357,4.36544996647721));
#60470=CARTESIAN_POINT('Ctrl Pts',(21.8870655758732,-17.4663772648075,3.66070649008719));
#60471=CARTESIAN_POINT('Ctrl Pts',(21.6983404251917,-17.6986070028546,3.25954202901027));
#60472=CARTESIAN_POINT('Ctrl Pts',(21.2342115445438,-18.2576809083209,1.96027825599731));
#60473=CARTESIAN_POINT('Ctrl Pts',(21.0673540166964,-18.4436057953749,0.960060375520683));
#60474=CARTESIAN_POINT('Ctrl Pts',(21.0673540166964,-18.4436057953749,0.));
#60475=CARTESIAN_POINT('',(25.9807621135332,-15.,6.));
#60476=CARTESIAN_POINT('Origin',(25.9807621135332,-15.,0.));
#60477=CARTESIAN_POINT('',(26.5063081645287,-9.02306087129181,0.));
#60478=CARTESIAN_POINT('Ctrl Pts',(26.5063081645287,-9.02306087129183,-2.77555756156289E-16));
#60479=CARTESIAN_POINT('Ctrl Pts',(26.5063081645287,-9.02306087129183,0.960060375520683));
#60480=CARTESIAN_POINT('Ctrl Pts',(26.428721253068,-9.26052617274731,1.96027825599731));
#60481=CARTESIAN_POINT('Ctrl Pts',(26.1766134886651,-9.94201052675154,3.25954202901027));
#60482=CARTESIAN_POINT('Ctrl Pts',(26.0698592113429,-10.2215661705984,3.6607064900872));
#60483=CARTESIAN_POINT('Ctrl Pts',(25.8112779008625,-10.8579881877023,4.36544996647721));
#60484=CARTESIAN_POINT('Ctrl Pts',(25.6592801974456,-11.2148229672334,4.66899487999358));
#60485=CARTESIAN_POINT('Ctrl Pts',(25.3279997590838,-11.9432855328977,5.14122028307955));
#60486=CARTESIAN_POINT('Ctrl Pts',(25.1338570880209,-12.3494418295706,5.3379209922756));
#60487=CARTESIAN_POINT('Ctrl Pts',(24.7066441580527,-13.1833691308415,5.59576473572533));
#60488=CARTESIAN_POINT('Ctrl Pts',(24.4732931529197,-13.6110128306156,5.65685424949238));
#60489=CARTESIAN_POINT('Ctrl Pts',(24.0615711505723,-14.3241362572753,5.65685424949238));
#60490=CARTESIAN_POINT('Ctrl Pts',(23.8543046840289,-14.6672240440326,5.61522291204339));
#60491=CARTESIAN_POINT('Ctrl Pts',(23.6431808351666,-14.9999999998537,5.52591293516556));
#60492=CARTESIAN_POINT('Origin',(25.9807621135332,-15.,0.));
#60493=CARTESIAN_POINT('Origin',(0.,0.,0.));
#60494=CARTESIAN_POINT('',(-28.,-3.42901103761259E-15,8.));
#60495=CARTESIAN_POINT('Origin',(0.,0.,8.));
#60496=CARTESIAN_POINT('',(-28.,8.96068962095847E-17,5.65685424949238));
#60497=CARTESIAN_POINT('',(-28.,-3.42901103761259E-15,0.));
#60498=CARTESIAN_POINT('',(-27.4666666666667,5.43895414783232,0.));
#60499=CARTESIAN_POINT('Ctrl Pts',(-28.,3.88578058618805E-15,5.65685424949238));
#60500=CARTESIAN_POINT('Ctrl Pts',(-28.,0.449163693910781,5.65685424949238));
#60501=CARTESIAN_POINT('Ctrl Pts',(-27.9882660485567,0.936189504250082,
5.59576473572533));
#60502=CARTESIAN_POINT('Ctrl Pts',(-27.941279648099,1.8719981970442,5.3379209922756));
#60503=CARTESIAN_POINT('Ctrl Pts',(-27.9063339848615,2.32081120340133,5.14122028307955));
#60504=CARTESIAN_POINT('Ctrl Pts',(-27.8289999774276,3.11731851015347,4.66899487999359));
#60505=CARTESIAN_POINT('Ctrl Pts',(-27.7822164601379,3.50234534588973,4.36544996647722));
#60506=CARTESIAN_POINT('Ctrl Pts',(-27.6879434354058,4.18279363546963,3.6607064900872));
#60507=CARTESIAN_POINT('Ctrl Pts',(-27.6406175296061,4.47827306347342,3.25954202901027));
#60508=CARTESIAN_POINT('Ctrl Pts',(-27.5182070810682,5.19450970852415,1.96027825599731));
#60509=CARTESIAN_POINT('Ctrl Pts',(-27.4666666666667,5.43895414783231,0.960060375520684));
#60510=CARTESIAN_POINT('Ctrl Pts',(-27.4666666666667,5.43895414783231,-5.55111512312578E-16));
#60511=CARTESIAN_POINT('',(-26.5063081645287,9.0230608712918,0.));
#60512=CARTESIAN_POINT('Origin',(0.,0.,0.));
#60513=CARTESIAN_POINT('',(-21.0673540166964,18.4436057953749,0.));
#60514=CARTESIAN_POINT('Ctrl Pts',(-26.5063081645287,9.02306087129181,-5.55111512312578E-16));
#60515=CARTESIAN_POINT('Ctrl Pts',(-26.5063081645287,9.02306087129181,0.960060375520683));
#60516=CARTESIAN_POINT('Ctrl Pts',(-26.428721253068,9.2605261727473,1.96027825599731));
#60517=CARTESIAN_POINT('Ctrl Pts',(-26.1766134886651,9.94201052675152,3.25954202901027));
#60518=CARTESIAN_POINT('Ctrl Pts',(-26.0698592113429,10.2215661705984,3.6607064900872));
#60519=CARTESIAN_POINT('Ctrl Pts',(-25.8112779008625,10.8579881877022,4.36544996647722));
#60520=CARTESIAN_POINT('Ctrl Pts',(-25.6592801974456,11.2148229672334,4.66899487999358));
#60521=CARTESIAN_POINT('Ctrl Pts',(-25.3279997590838,11.9432855328977,5.14122028307955));
#60522=CARTESIAN_POINT('Ctrl Pts',(-25.1338570880209,12.3494418295705,5.3379209922756));
#60523=CARTESIAN_POINT('Ctrl Pts',(-24.7066441580527,13.1833691308414,5.59576473572533));
#60524=CARTESIAN_POINT('Ctrl Pts',(-24.4732931529197,13.6110128306156,5.65685424949238));
#60525=CARTESIAN_POINT('Ctrl Pts',(-24.0241294590089,14.3889871693844,5.65685424949238));
#60526=CARTESIAN_POINT('Ctrl Pts',(-23.7704546538026,14.8048969177153,5.59576473572533));
#60527=CARTESIAN_POINT('Ctrl Pts',(-23.2618588909767,15.5918378185284,5.3379209922756));
#60528=CARTESIAN_POINT('Ctrl Pts',(-23.0071885556824,15.9630484519638,5.14122028307955));
#60529=CARTESIAN_POINT('Ctrl Pts',(-22.5419616872921,16.6141770101942,4.66899487999358));
#60530=CARTESIAN_POINT('Ctrl Pts',(-22.3089325549727,16.9242282724357,4.36544996647721));
#60531=CARTESIAN_POINT('Ctrl Pts',(-21.8870655758732,17.4663772648075,3.66070649008719));
#60532=CARTESIAN_POINT('Ctrl Pts',(-21.6983404251917,17.6986070028546,3.25954202901027));
#60533=CARTESIAN_POINT('Ctrl Pts',(-21.2342115445438,18.2576809083209,1.96027825599731));
#60534=CARTESIAN_POINT('Ctrl Pts',(-21.0673540166964,18.4436057953748,0.960060375520683));
#60535=CARTESIAN_POINT('Ctrl Pts',(-21.0673540166964,18.4436057953748,-2.77555756156289E-16));
#60536=CARTESIAN_POINT('',(-18.4436057953749,21.0673540166964,0.));
#60537=CARTESIAN_POINT('Origin',(0.,0.,0.));
#60538=CARTESIAN_POINT('',(-9.0230608712918,26.5063081645287,0.));
#60539=CARTESIAN_POINT('Ctrl Pts',(-18.4436057953748,21.0673540166964,-2.77555756156289E-16));
#60540=CARTESIAN_POINT('Ctrl Pts',(-18.4436057953748,21.0673540166964,0.960060375520684));
#60541=CARTESIAN_POINT('Ctrl Pts',(-18.2576809083209,21.2342115445438,1.96027825599731));
#60542=CARTESIAN_POINT('Ctrl Pts',(-17.6986070028546,21.6983404251917,3.25954202901027));
#60543=CARTESIAN_POINT('Ctrl Pts',(-17.4663772648075,21.8870655758732,3.6607064900872));
#60544=CARTESIAN_POINT('Ctrl Pts',(-16.9242282724357,22.3089325549727,4.36544996647722));
#60545=CARTESIAN_POINT('Ctrl Pts',(-16.6141770101941,22.5419616872921,4.66899487999358));
#60546=CARTESIAN_POINT('Ctrl Pts',(-15.9630484519638,23.0071885556824,5.14122028307955));
#60547=CARTESIAN_POINT('Ctrl Pts',(-15.5918378185284,23.2618588909768,5.3379209922756));
#60548=CARTESIAN_POINT('Ctrl Pts',(-14.8048969177153,23.7704546538026,5.59576473572533));
#60549=CARTESIAN_POINT('Ctrl Pts',(-14.3889871693844,24.0241294590089,5.65685424949238));
#60550=CARTESIAN_POINT('Ctrl Pts',(-13.6110128306156,24.4732931529197,5.65685424949238));
#60551=CARTESIAN_POINT('Ctrl Pts',(-13.1833691308414,24.7066441580527,5.59576473572533));
#60552=CARTESIAN_POINT('Ctrl Pts',(-12.3494418295705,25.1338570880209,5.3379209922756));
#60553=CARTESIAN_POINT('Ctrl Pts',(-11.9432855328977,25.3279997590838,5.14122028307955));
#60554=CARTESIAN_POINT('Ctrl Pts',(-11.2148229672334,25.6592801974456,4.66899487999358));
#60555=CARTESIAN_POINT('Ctrl Pts',(-10.8579881877022,25.8112779008625,4.36544996647721));
#60556=CARTESIAN_POINT('Ctrl Pts',(-10.2215661705984,26.0698592113429,3.6607064900872));
#60557=CARTESIAN_POINT('Ctrl Pts',(-9.94201052675152,26.1766134886651,3.25954202901027));
#60558=CARTESIAN_POINT('Ctrl Pts',(-9.26052617274729,26.428721253068,1.96027825599731));
#60559=CARTESIAN_POINT('Ctrl Pts',(-9.02306087129181,26.5063081645287,0.960060375520683));
#60560=CARTESIAN_POINT('Ctrl Pts',(-9.02306087129181,26.5063081645287,-2.77555756156289E-16));
#60561=CARTESIAN_POINT('',(-5.43895414783229,27.4666666666667,0.));
#60562=CARTESIAN_POINT('Origin',(0.,0.,0.));
#60563=CARTESIAN_POINT('',(5.4389541478323,27.4666666666667,0.));
#60564=CARTESIAN_POINT('Ctrl Pts',(-5.4389541478323,27.4666666666667,2.77555756156289E-16));
#60565=CARTESIAN_POINT('Ctrl Pts',(-5.4389541478323,27.4666666666667,0.960060375520684));
#60566=CARTESIAN_POINT('Ctrl Pts',(-5.19450970852415,27.5182070810682,1.96027825599731));
#60567=CARTESIAN_POINT('Ctrl Pts',(-4.47827306347342,27.6406175296061,3.25954202901027));
#60568=CARTESIAN_POINT('Ctrl Pts',(-4.18279363546962,27.6879434354058,3.6607064900872));
#60569=CARTESIAN_POINT('Ctrl Pts',(-3.50234534588973,27.7822164601379,4.36544996647721));
#60570=CARTESIAN_POINT('Ctrl Pts',(-3.11731851015347,27.8289999774276,4.66899487999358));
#60571=CARTESIAN_POINT('Ctrl Pts',(-2.32081120340133,27.9063339848615,5.14122028307955));
#60572=CARTESIAN_POINT('Ctrl Pts',(-1.8719981970442,27.941279648099,5.3379209922756));
#60573=CARTESIAN_POINT('Ctrl Pts',(-0.936189504250081,27.9882660485567,
5.59576473572533));
#60574=CARTESIAN_POINT('Ctrl Pts',(-0.449163693910777,28.,5.65685424949238));
#60575=CARTESIAN_POINT('Ctrl Pts',(0.449163693910781,28.,5.65685424949238));
#60576=CARTESIAN_POINT('Ctrl Pts',(0.936189504250085,27.9882660485567,5.59576473572533));
#60577=CARTESIAN_POINT('Ctrl Pts',(1.8719981970442,27.941279648099,5.3379209922756));
#60578=CARTESIAN_POINT('Ctrl Pts',(2.32081120340133,27.9063339848615,5.14122028307955));
#60579=CARTESIAN_POINT('Ctrl Pts',(3.11731851015347,27.8289999774276,4.66899487999358));
#60580=CARTESIAN_POINT('Ctrl Pts',(3.50234534588973,27.7822164601379,4.36544996647721));
#60581=CARTESIAN_POINT('Ctrl Pts',(4.18279363546963,27.6879434354058,3.6607064900872));
#60582=CARTESIAN_POINT('Ctrl Pts',(4.47827306347342,27.6406175296061,3.25954202901027));
#60583=CARTESIAN_POINT('Ctrl Pts',(5.19450970852415,27.5182070810682,1.96027825599731));
#60584=CARTESIAN_POINT('Ctrl Pts',(5.4389541478323,27.4666666666667,0.960060375520683));
#60585=CARTESIAN_POINT('Ctrl Pts',(5.4389541478323,27.4666666666667,2.77555756156289E-16));
#60586=CARTESIAN_POINT('',(9.0230608712918,26.5063081645287,0.));
#60587=CARTESIAN_POINT('Origin',(0.,0.,0.));
#60588=CARTESIAN_POINT('',(10.4403065089456,25.9807621135261,3.89989682781948));
#60589=CARTESIAN_POINT('Ctrl Pts',(9.02306087129182,26.5063081645287,0.));
#60590=CARTESIAN_POINT('Ctrl Pts',(9.02306087129182,26.5063081645287,0.960060375520684));
#60591=CARTESIAN_POINT('Ctrl Pts',(9.2605261727473,26.428721253068,1.96027825599731));
#60592=CARTESIAN_POINT('Ctrl Pts',(9.9180326009165,26.1854838629323,3.21382762602157));
#60593=CARTESIAN_POINT('Ctrl Pts',(10.1630550776949,26.0921749315747,3.57573913794424));
#60594=CARTESIAN_POINT('Ctrl Pts',(10.4403065089456,25.9807621135191,3.89989682781948));
#60595=CARTESIAN_POINT('',(18.4436057953749,21.0673540166964,0.));
#60596=CARTESIAN_POINT('Ctrl Pts',(10.4403065089456,25.9807621135191,3.89989682781948));
#60597=CARTESIAN_POINT('Ctrl Pts',(10.4730252750948,25.9676141563614,3.93815105649065));
#60598=CARTESIAN_POINT('Ctrl Pts',(10.5061885578498,25.9542157736402,3.97588378637688));
#60599=CARTESIAN_POINT('Ctrl Pts',(10.8579881877023,25.8112779008625,4.36544996647722));
#60600=CARTESIAN_POINT('Ctrl Pts',(11.2148229672334,25.6592801974456,4.66899487999358));
#60601=CARTESIAN_POINT('Ctrl Pts',(11.9432855328977,25.3279997590838,5.14122028307955));
#60602=CARTESIAN_POINT('Ctrl Pts',(12.3494418295706,25.1338570880209,5.3379209922756));
#60603=CARTESIAN_POINT('Ctrl Pts',(13.1833691308414,24.7066441580527,5.59576473572533));
#60604=CARTESIAN_POINT('Ctrl Pts',(13.6110128306156,24.4732931529197,5.65685424949238));
#60605=CARTESIAN_POINT('Ctrl Pts',(14.3889871693844,24.0241294590089,5.65685424949238));
#60606=CARTESIAN_POINT('Ctrl Pts',(14.8048969177153,23.7704546538026,5.59576473572533));
#60607=CARTESIAN_POINT('Ctrl Pts',(15.5918378185284,23.2618588909767,5.3379209922756));
#60608=CARTESIAN_POINT('Ctrl Pts',(15.9630484519639,23.0071885556824,5.14122028307955));
#60609=CARTESIAN_POINT('Ctrl Pts',(16.6141770101942,22.5419616872921,4.66899487999358));
#60610=CARTESIAN_POINT('Ctrl Pts',(16.9242282724357,22.3089325549727,4.36544996647722));
#60611=CARTESIAN_POINT('Ctrl Pts',(17.4663772648075,21.8870655758732,3.6607064900872));
#60612=CARTESIAN_POINT('Ctrl Pts',(17.6986070028546,21.6983404251917,3.25954202901027));
#60613=CARTESIAN_POINT('Ctrl Pts',(18.2576809083209,21.2342115445438,1.96027825599731));
#60614=CARTESIAN_POINT('Ctrl Pts',(18.4436057953749,21.0673540166964,0.960060375520683));
#60615=CARTESIAN_POINT('Ctrl Pts',(18.4436057953749,21.0673540166964,-2.77555756156289E-16));
#60616=CARTESIAN_POINT('',(21.0673540166964,18.4436057953749,0.));
#60617=CARTESIAN_POINT('Origin',(0.,0.,0.));
#60618=CARTESIAN_POINT('',(23.6431808351666,14.9999999999269,5.52591293516556));
#60619=CARTESIAN_POINT('Ctrl Pts',(21.0673540166964,18.4436057953749,-2.77555756156289E-16));
#60620=CARTESIAN_POINT('Ctrl Pts',(21.0673540166964,18.4436057953749,0.960060375520684));
#60621=CARTESIAN_POINT('Ctrl Pts',(21.2342115445438,18.2576809083209,1.96027825599731));
#60622=CARTESIAN_POINT('Ctrl Pts',(21.6983404251917,17.6986070028546,3.25954202901027));
#60623=CARTESIAN_POINT('Ctrl Pts',(21.8870655758732,17.4663772648075,3.6607064900872));
#60624=CARTESIAN_POINT('Ctrl Pts',(22.3089325549727,16.9242282724357,4.36544996647722));
#60625=CARTESIAN_POINT('Ctrl Pts',(22.5419616872921,16.6141770101941,4.66899487999358));
#60626=CARTESIAN_POINT('Ctrl Pts',(23.0071885556824,15.9630484519638,5.14122028307955));
#60627=CARTESIAN_POINT('Ctrl Pts',(23.2618588909767,15.5918378185284,5.3379209922756));
#60628=CARTESIAN_POINT('Ctrl Pts',(23.5585526426266,15.1327690152579,5.48833637748937));
#60629=CARTESIAN_POINT('Ctrl Pts',(23.6009406541952,15.0665794823355,5.50804442051787));
#60630=CARTESIAN_POINT('Ctrl Pts',(23.6431808351666,14.9999999998537,5.52591293516556));
#60631=CARTESIAN_POINT('',(26.5063081645287,9.0230608712918,0.));
#60632=CARTESIAN_POINT('Ctrl Pts',(23.6431808351666,14.9999999998537,5.52591293516556));
#60633=CARTESIAN_POINT('Ctrl Pts',(23.8543046840289,14.6672240440326,5.61522291204339));
#60634=CARTESIAN_POINT('Ctrl Pts',(24.0615711505723,14.3241362572753,5.65685424949238));
#60635=CARTESIAN_POINT('Ctrl Pts',(24.4732931529197,13.6110128306156,5.65685424949238));
#60636=CARTESIAN_POINT('Ctrl Pts',(24.7066441580527,13.1833691308414,5.59576473572533));
#60637=CARTESIAN_POINT('Ctrl Pts',(25.1338570880209,12.3494418295705,5.3379209922756));
#60638=CARTESIAN_POINT('Ctrl Pts',(25.3279997590838,11.9432855328977,5.14122028307955));
#60639=CARTESIAN_POINT('Ctrl Pts',(25.6592801974456,11.2148229672334,4.66899487999358));
#60640=CARTESIAN_POINT('Ctrl Pts',(25.8112779008625,10.8579881877022,4.36544996647722));
#60641=CARTESIAN_POINT('Ctrl Pts',(26.0698592113429,10.2215661705984,3.6607064900872));
#60642=CARTESIAN_POINT('Ctrl Pts',(26.1766134886651,9.94201052675152,3.25954202901027));
#60643=CARTESIAN_POINT('Ctrl Pts',(26.428721253068,9.2605261727473,1.96027825599731));
#60644=CARTESIAN_POINT('Ctrl Pts',(26.5063081645287,9.02306087129181,0.960060375520683));
#60645=CARTESIAN_POINT('Ctrl Pts',(26.5063081645287,9.02306087129181,-2.77555756156289E-16));
#60646=CARTESIAN_POINT('',(27.4666666666667,5.43895414783232,0.));
#60647=CARTESIAN_POINT('Origin',(0.,0.,0.));
#60648=CARTESIAN_POINT('',(28.,-2.6124255799288E-16,5.65685424949238));
#60649=CARTESIAN_POINT('Ctrl Pts',(27.4666666666667,5.4389541478323,-2.77555756156289E-16));
#60650=CARTESIAN_POINT('Ctrl Pts',(27.4666666666667,5.4389541478323,0.960060375520684));
#60651=CARTESIAN_POINT('Ctrl Pts',(27.5182070810682,5.19450970852415,1.96027825599731));
#60652=CARTESIAN_POINT('Ctrl Pts',(27.6406175296061,4.47827306347342,3.25954202901027));
#60653=CARTESIAN_POINT('Ctrl Pts',(27.6879434354058,4.18279363546963,3.6607064900872));
#60654=CARTESIAN_POINT('Ctrl Pts',(27.7822164601379,3.50234534588973,4.36544996647722));
#60655=CARTESIAN_POINT('Ctrl Pts',(27.8289999774276,3.11731851015347,4.66899487999358));
#60656=CARTESIAN_POINT('Ctrl Pts',(27.9063339848615,2.32081120340133,5.14122028307955));
#60657=CARTESIAN_POINT('Ctrl Pts',(27.941279648099,1.8719981970442,5.3379209922756));
#60658=CARTESIAN_POINT('Ctrl Pts',(27.9882660485567,0.936189504250083,5.59576473572533));
#60659=CARTESIAN_POINT('Ctrl Pts',(28.,0.449163693910779,5.65685424949238));
#60660=CARTESIAN_POINT('Ctrl Pts',(28.,-1.38777878078145E-16,5.65685424949238));
#60661=CARTESIAN_POINT('',(27.4666666666667,-5.43895414783232,0.));
#60662=CARTESIAN_POINT('Ctrl Pts',(28.,0.,5.65685424949238));
#60663=CARTESIAN_POINT('Ctrl Pts',(28.,-0.449163693910779,5.65685424949238));
#60664=CARTESIAN_POINT('Ctrl Pts',(27.9882660485567,-0.936189504250083,
5.59576473572533));
#60665=CARTESIAN_POINT('Ctrl Pts',(27.941279648099,-1.8719981970442,5.3379209922756));
#60666=CARTESIAN_POINT('Ctrl Pts',(27.9063339848615,-2.32081120340133,5.14122028307955));
#60667=CARTESIAN_POINT('Ctrl Pts',(27.8289999774276,-3.11731851015347,4.66899487999358));
#60668=CARTESIAN_POINT('Ctrl Pts',(27.7822164601379,-3.50234534588973,4.36544996647722));
#60669=CARTESIAN_POINT('Ctrl Pts',(27.6879434354058,-4.18279363546962,3.6607064900872));
#60670=CARTESIAN_POINT('Ctrl Pts',(27.6406175296061,-4.47827306347342,3.25954202901027));
#60671=CARTESIAN_POINT('Ctrl Pts',(27.5182070810682,-5.19450970852415,1.96027825599731));
#60672=CARTESIAN_POINT('Ctrl Pts',(27.4666666666667,-5.4389541478323,0.960060375520684));
#60673=CARTESIAN_POINT('Ctrl Pts',(27.4666666666667,-5.4389541478323,-2.77555756156289E-16));
#60674=CARTESIAN_POINT('Origin',(0.,0.,0.));
#60675=CARTESIAN_POINT('',(18.4436057953749,-21.0673540166964,0.));
#60676=CARTESIAN_POINT('Origin',(0.,0.,0.));
#60677=CARTESIAN_POINT('',(10.4403065089456,-25.9807621135261,3.89989682781947));
#60678=CARTESIAN_POINT('Ctrl Pts',(18.4436057953749,-21.0673540166964,-2.77555756156289E-16));
#60679=CARTESIAN_POINT('Ctrl Pts',(18.4436057953749,-21.0673540166964,0.960060375520682));
#60680=CARTESIAN_POINT('Ctrl Pts',(18.2576809083209,-21.2342115445438,1.96027825599731));
#60681=CARTESIAN_POINT('Ctrl Pts',(17.6986070028546,-21.6983404251917,3.25954202901027));
#60682=CARTESIAN_POINT('Ctrl Pts',(17.4663772648075,-21.8870655758732,3.6607064900872));
#60683=CARTESIAN_POINT('Ctrl Pts',(16.9242282724357,-22.3089325549727,4.36544996647722));
#60684=CARTESIAN_POINT('Ctrl Pts',(16.6141770101942,-22.5419616872921,4.66899487999358));
#60685=CARTESIAN_POINT('Ctrl Pts',(15.9630484519639,-23.0071885556824,5.14122028307955));
#60686=CARTESIAN_POINT('Ctrl Pts',(15.5918378185284,-23.2618588909767,5.3379209922756));
#60687=CARTESIAN_POINT('Ctrl Pts',(14.8048969177153,-23.7704546538026,5.59576473572533));
#60688=CARTESIAN_POINT('Ctrl Pts',(14.3889871693844,-24.0241294590089,5.65685424949238));
#60689=CARTESIAN_POINT('Ctrl Pts',(13.6110128306156,-24.4732931529197,5.65685424949238));
#60690=CARTESIAN_POINT('Ctrl Pts',(13.1833691308414,-24.7066441580527,5.59576473572533));
#60691=CARTESIAN_POINT('Ctrl Pts',(12.3494418295706,-25.133857088021,5.3379209922756));
#60692=CARTESIAN_POINT('Ctrl Pts',(11.9432855328977,-25.3279997590838,5.14122028307955));
#60693=CARTESIAN_POINT('Ctrl Pts',(11.2148229672334,-25.6592801974456,4.66899487999358));
#60694=CARTESIAN_POINT('Ctrl Pts',(10.8579881877023,-25.8112779008625,4.36544996647722));
#60695=CARTESIAN_POINT('Ctrl Pts',(10.5061885578498,-25.9542157736402,3.97588378637689));
#60696=CARTESIAN_POINT('Ctrl Pts',(10.4730252750948,-25.9676141563614,3.93815105649065));
#60697=CARTESIAN_POINT('Ctrl Pts',(10.4403065089456,-25.9807621135191,3.89989682781947));
#60698=CARTESIAN_POINT('',(9.0230608712918,-26.5063081645287,0.));
#60699=CARTESIAN_POINT('Ctrl Pts',(10.4403065089456,-25.9807621135191,3.89989682781947));
#60700=CARTESIAN_POINT('Ctrl Pts',(10.1630550776949,-26.0921749315747,3.57573913794424));
#60701=CARTESIAN_POINT('Ctrl Pts',(9.9180326009165,-26.1854838629323,3.21382762602157));
#60702=CARTESIAN_POINT('Ctrl Pts',(9.2605261727473,-26.428721253068,1.96027825599731));
#60703=CARTESIAN_POINT('Ctrl Pts',(9.02306087129182,-26.5063081645287,0.960060375520684));
#60704=CARTESIAN_POINT('Ctrl Pts',(9.02306087129182,-26.5063081645287,-5.55111512312578E-16));
#60705=CARTESIAN_POINT('',(5.43895414783231,-27.4666666666667,0.));
#60706=CARTESIAN_POINT('Origin',(0.,0.,0.));
#60707=CARTESIAN_POINT('',(-5.43895414783233,-27.4666666666667,0.));
#60708=CARTESIAN_POINT('Ctrl Pts',(5.4389541478323,-27.4666666666667,0.));
#60709=CARTESIAN_POINT('Ctrl Pts',(5.4389541478323,-27.4666666666667,0.960060375520685));
#60710=CARTESIAN_POINT('Ctrl Pts',(5.19450970852414,-27.5182070810682,1.96027825599731));
#60711=CARTESIAN_POINT('Ctrl Pts',(4.47827306347341,-27.6406175296061,3.25954202901027));
#60712=CARTESIAN_POINT('Ctrl Pts',(4.18279363546962,-27.6879434354058,3.6607064900872));
#60713=CARTESIAN_POINT('Ctrl Pts',(3.50234534588972,-27.7822164601379,4.36544996647722));
#60714=CARTESIAN_POINT('Ctrl Pts',(3.11731851015346,-27.8289999774276,4.66899487999358));
#60715=CARTESIAN_POINT('Ctrl Pts',(2.32081120340132,-27.9063339848615,5.14122028307955));
#60716=CARTESIAN_POINT('Ctrl Pts',(1.87199819704419,-27.941279648099,5.3379209922756));
#60717=CARTESIAN_POINT('Ctrl Pts',(0.936189504250074,-27.9882660485567,
5.59576473572533));
#60718=CARTESIAN_POINT('Ctrl Pts',(0.449163693910773,-28.,5.65685424949238));
#60719=CARTESIAN_POINT('Ctrl Pts',(-0.449163693910784,-28.,5.65685424949238));
#60720=CARTESIAN_POINT('Ctrl Pts',(-0.936189504250087,-27.9882660485567,
5.59576473572533));
#60721=CARTESIAN_POINT('Ctrl Pts',(-1.87199819704421,-27.941279648099,5.3379209922756));
#60722=CARTESIAN_POINT('Ctrl Pts',(-2.32081120340134,-27.9063339848615,
5.14122028307955));
#60723=CARTESIAN_POINT('Ctrl Pts',(-3.11731851015348,-27.8289999774276,
4.66899487999358));
#60724=CARTESIAN_POINT('Ctrl Pts',(-3.50234534588974,-27.7822164601379,
4.36544996647722));
#60725=CARTESIAN_POINT('Ctrl Pts',(-4.18279363546963,-27.6879434354058,
3.6607064900872));
#60726=CARTESIAN_POINT('Ctrl Pts',(-4.47827306347343,-27.6406175296061,
3.25954202901027));
#60727=CARTESIAN_POINT('Ctrl Pts',(-5.19450970852415,-27.5182070810682,
1.96027825599731));
#60728=CARTESIAN_POINT('Ctrl Pts',(-5.43895414783231,-27.4666666666667,
0.960060375520684));
#60729=CARTESIAN_POINT('Ctrl Pts',(-5.43895414783231,-27.4666666666667,
-2.77555756156289E-16));
#60730=CARTESIAN_POINT('',(-9.02306087129181,-26.5063081645287,0.));
#60731=CARTESIAN_POINT('Origin',(0.,0.,0.));
#60732=CARTESIAN_POINT('',(-18.4436057953749,-21.0673540166964,0.));
#60733=CARTESIAN_POINT('Ctrl Pts',(-9.02306087129183,-26.5063081645287,
-2.77555756156289E-16));
#60734=CARTESIAN_POINT('Ctrl Pts',(-9.02306087129183,-26.5063081645287,
0.960060375520684));
#60735=CARTESIAN_POINT('Ctrl Pts',(-9.26052617274731,-26.428721253068,1.96027825599731));
#60736=CARTESIAN_POINT('Ctrl Pts',(-9.94201052675154,-26.1766134886651,
3.25954202901027));
#60737=CARTESIAN_POINT('Ctrl Pts',(-10.2215661705984,-26.0698592113429,
3.6607064900872));
#60738=CARTESIAN_POINT('Ctrl Pts',(-10.8579881877023,-25.8112779008625,
4.36544996647722));
#60739=CARTESIAN_POINT('Ctrl Pts',(-11.2148229672334,-25.6592801974456,
4.66899487999358));
#60740=CARTESIAN_POINT('Ctrl Pts',(-11.9432855328977,-25.3279997590838,
5.14122028307955));
#60741=CARTESIAN_POINT('Ctrl Pts',(-12.3494418295706,-25.1338570880209,
5.3379209922756));
#60742=CARTESIAN_POINT('Ctrl Pts',(-13.1833691308415,-24.7066441580527,
5.59576473572533));
#60743=CARTESIAN_POINT('Ctrl Pts',(-13.6110128306156,-24.4732931529197,
5.65685424949238));
#60744=CARTESIAN_POINT('Ctrl Pts',(-14.3889871693844,-24.0241294590089,
5.65685424949238));
#60745=CARTESIAN_POINT('Ctrl Pts',(-14.8048969177153,-23.7704546538026,
5.59576473572533));
#60746=CARTESIAN_POINT('Ctrl Pts',(-15.5918378185285,-23.2618588909767,
5.3379209922756));
#60747=CARTESIAN_POINT('Ctrl Pts',(-15.9630484519639,-23.0071885556824,
5.14122028307955));
#60748=CARTESIAN_POINT('Ctrl Pts',(-16.6141770101942,-22.5419616872921,
4.66899487999358));
#60749=CARTESIAN_POINT('Ctrl Pts',(-16.9242282724357,-22.3089325549727,
4.36544996647722));
#60750=CARTESIAN_POINT('Ctrl Pts',(-17.4663772648075,-21.8870655758732,
3.6607064900872));
#60751=CARTESIAN_POINT('Ctrl Pts',(-17.6986070028546,-21.6983404251917,
3.25954202901027));
#60752=CARTESIAN_POINT('Ctrl Pts',(-18.2576809083209,-21.2342115445438,
1.96027825599731));
#60753=CARTESIAN_POINT('Ctrl Pts',(-18.4436057953749,-21.0673540166964,
0.960060375520684));
#60754=CARTESIAN_POINT('Ctrl Pts',(-18.4436057953749,-21.0673540166964,
-5.55111512312578E-16));
#60755=CARTESIAN_POINT('',(-21.0673540166964,-18.4436057953749,0.));
#60756=CARTESIAN_POINT('Origin',(0.,0.,0.));
#60757=CARTESIAN_POINT('',(-26.5063081645287,-9.0230608712918,0.));
#60758=CARTESIAN_POINT('Ctrl Pts',(-21.0673540166964,-18.4436057953749,
-2.77555756156289E-16));
#60759=CARTESIAN_POINT('Ctrl Pts',(-21.0673540166964,-18.4436057953749,
0.960060375520684));
#60760=CARTESIAN_POINT('Ctrl Pts',(-21.2342115445438,-18.2576809083209,
1.96027825599731));
#60761=CARTESIAN_POINT('Ctrl Pts',(-21.6983404251917,-17.6986070028546,
3.25954202901027));
#60762=CARTESIAN_POINT('Ctrl Pts',(-21.8870655758732,-17.4663772648075,
3.6607064900872));
#60763=CARTESIAN_POINT('Ctrl Pts',(-22.3089325549727,-16.9242282724357,
4.36544996647722));
#60764=CARTESIAN_POINT('Ctrl Pts',(-22.5419616872921,-16.6141770101942,
4.66899487999358));
#60765=CARTESIAN_POINT('Ctrl Pts',(-23.0071885556824,-15.9630484519638,
5.14122028307955));
#60766=CARTESIAN_POINT('Ctrl Pts',(-23.2618588909767,-15.5918378185284,
5.3379209922756));
#60767=CARTESIAN_POINT('Ctrl Pts',(-23.7704546538026,-14.8048969177153,
5.59576473572534));
#60768=CARTESIAN_POINT('Ctrl Pts',(-24.0241294590089,-14.3889871693844,
5.65685424949239));
#60769=CARTESIAN_POINT('Ctrl Pts',(-24.4732931529197,-13.6110128306156,
5.65685424949239));
#60770=CARTESIAN_POINT('Ctrl Pts',(-24.7066441580527,-13.1833691308414,
5.59576473572533));
#60771=CARTESIAN_POINT('Ctrl Pts',(-25.1338570880209,-12.3494418295705,
5.33792099227561));
#60772=CARTESIAN_POINT('Ctrl Pts',(-25.3279997590838,-11.9432855328977,
5.14122028307956));
#60773=CARTESIAN_POINT('Ctrl Pts',(-25.6592801974456,-11.2148229672334,
4.66899487999359));
#60774=CARTESIAN_POINT('Ctrl Pts',(-25.8112779008625,-10.8579881877022,
4.36544996647723));
#60775=CARTESIAN_POINT('Ctrl Pts',(-26.0698592113429,-10.2215661705984,
3.66070649008721));
#60776=CARTESIAN_POINT('Ctrl Pts',(-26.1766134886651,-9.94201052675152,
3.25954202901028));
#60777=CARTESIAN_POINT('Ctrl Pts',(-26.428721253068,-9.26052617274729,1.96027825599731));
#60778=CARTESIAN_POINT('Ctrl Pts',(-26.5063081645287,-9.0230608712918,0.960060375520686));
#60779=CARTESIAN_POINT('Ctrl Pts',(-26.5063081645287,-9.0230608712918,-2.77555756156289E-16));
#60780=CARTESIAN_POINT('',(-27.4666666666667,-5.43895414783232,0.));
#60781=CARTESIAN_POINT('Origin',(0.,0.,0.));
#60782=CARTESIAN_POINT('Ctrl Pts',(-27.4666666666667,-5.4389541478323,-2.77555756156289E-16));
#60783=CARTESIAN_POINT('Ctrl Pts',(-27.4666666666667,-5.4389541478323,0.960060375520681));
#60784=CARTESIAN_POINT('Ctrl Pts',(-27.5182070810682,-5.19450970852415,
1.9602782559973));
#60785=CARTESIAN_POINT('Ctrl Pts',(-27.6406175296061,-4.47827306347342,
3.25954202901026));
#60786=CARTESIAN_POINT('Ctrl Pts',(-27.6879434354058,-4.18279363546963,
3.66070649008719));
#60787=CARTESIAN_POINT('Ctrl Pts',(-27.7822164601379,-3.50234534588974,
4.36544996647721));
#60788=CARTESIAN_POINT('Ctrl Pts',(-27.8289999774276,-3.11731851015348,
4.66899487999357));
#60789=CARTESIAN_POINT('Ctrl Pts',(-27.9063339848615,-2.32081120340134,
5.14122028307955));
#60790=CARTESIAN_POINT('Ctrl Pts',(-27.941279648099,-1.87199819704421,5.3379209922756));
#60791=CARTESIAN_POINT('Ctrl Pts',(-27.9882660485567,-0.936189504250084,
5.59576473572533));
#60792=CARTESIAN_POINT('Ctrl Pts',(-28.,-0.449163693910778,5.65685424949238));
#60793=CARTESIAN_POINT('Ctrl Pts',(-28.,3.88578058618805E-15,5.65685424949238));
#60794=CARTESIAN_POINT('Origin',(0.,0.,0.));
#60795=CARTESIAN_POINT('',(20.771851634051,-24.3419428085142,0.));
#60796=CARTESIAN_POINT('Origin',(0.,0.,0.));
#60797=CARTESIAN_POINT('Origin',(15.,-25.9807621135332,0.));
#60798=CARTESIAN_POINT('Origin',(15.,-25.9807621135332,0.));
#60799=CARTESIAN_POINT('',(10.6948150326157,-30.1599226029865,0.));
#60800=CARTESIAN_POINT('Ctrl Pts',(10.6948150326157,-30.1599226029865,2.77555756156289E-16));
#60801=CARTESIAN_POINT('Ctrl Pts',(10.6948150326157,-30.1599226029865,0.650190448083164));
#60802=CARTESIAN_POINT('Ctrl Pts',(10.811636102503,-30.1192963151694,1.34576815070429));
#60803=CARTESIAN_POINT('Ctrl Pts',(11.2845860623018,-29.945310285088,2.63799288444814));
#60804=CARTESIAN_POINT('Ctrl Pts',(11.6401587249113,-29.8110127779048,3.23471700046071));
#60805=CARTESIAN_POINT('Ctrl Pts',(12.2267378431101,-29.5727220114149,3.93620747216806));
#60806=CARTESIAN_POINT('Ctrl Pts',(12.4429603313741,-29.4828111958893,4.15945687249389));
#60807=CARTESIAN_POINT('Ctrl Pts',(12.9054296448663,-29.2833280818651,4.56176656225472));
#60808=CARTESIAN_POINT('Ctrl Pts',(13.1515948772024,-29.1736430103094,4.74086471477473));
#60809=CARTESIAN_POINT('Ctrl Pts',(13.7691022238565,-28.8892863729454,5.12459397949763));
#60810=CARTESIAN_POINT('Ctrl Pts',(14.2110789657823,-28.6758520004508,5.32832509625205));
#60811=CARTESIAN_POINT('Ctrl Pts',(15.116207912957,-28.2092096970821,5.59441429610713));
#60812=CARTESIAN_POINT('Ctrl Pts',(15.5792095317074,-27.9557564112432,5.65685424949238));
#60813=CARTESIAN_POINT('Ctrl Pts',(16.4207904682926,-27.4698694309609,5.65685424949238));
#60814=CARTESIAN_POINT('Ctrl Pts',(16.8717882618769,-27.1956249100491,5.59441429610713));
#60815=CARTESIAN_POINT('Ctrl Pts',(17.7284768246621,-26.6450813997796,5.32832509625205));
#60816=CARTESIAN_POINT('Ctrl Pts',(18.1343047842461,-26.3690354996372,5.12459397949762));
#60817=CARTESIAN_POINT('Ctrl Pts',(18.6893185292651,-25.9764367690933,4.74086471477472));
#60818=CARTESIAN_POINT('Ctrl Pts',(18.9073912038163,-25.8180939601396,4.56176656225471));
#60819=CARTESIAN_POINT('Ctrl Pts',(19.3113833049334,-25.5173253431967,4.15945687249388));
#60820=CARTESIAN_POINT('Ctrl Pts',(19.4973595993855,-25.3750265832533,3.93620747216806));
#60821=CARTESIAN_POINT('Ctrl Pts',(19.9970150157524,-24.9861795488087,3.23471700046071));
#60822=CARTESIAN_POINT('Ctrl Pts',(20.2911063999427,-24.7453933436892,2.63799288444813));
#60823=CARTESIAN_POINT('Ctrl Pts',(20.6782577017963,-24.4227996788253,1.34576815070429));
#60824=CARTESIAN_POINT('Ctrl Pts',(20.771851634051,-24.3419428085141,0.650190448083162));
#60825=CARTESIAN_POINT('Ctrl Pts',(20.771851634051,-24.3419428085141,-1.38777878078145E-16));
#60826=CARTESIAN_POINT('Origin',(15.,-25.9807621135332,0.));
#60827=CARTESIAN_POINT('',(15.,-25.9807621135332,6.));
#60828=CARTESIAN_POINT('Origin',(15.,-25.9807621135332,0.));
#60829=CARTESIAN_POINT('Origin',(0.,0.,0.));
#60830=CARTESIAN_POINT('',(5.81797979447235,-31.4666666666667,0.));
#60831=CARTESIAN_POINT('Origin',(0.,0.,0.));
#60832=CARTESIAN_POINT('Origin',(-5.55111512312578E-15,-30.,0.));
#60833=CARTESIAN_POINT('Origin',(-5.55111512312578E-15,-30.,0.));
#60834=CARTESIAN_POINT('',(-5.81797979447236,-31.4666666666667,0.));
#60835=CARTESIAN_POINT('Ctrl Pts',(-5.81797979447239,-31.4666666666667,
2.77555756156289E-16));
#60836=CARTESIAN_POINT('Ctrl Pts',(-5.81797979447239,-31.4666666666667,
0.650190448083165));
#60837=CARTESIAN_POINT('Ctrl Pts',(-5.69649663634415,-31.4898938042992,
1.34576815070429));
#60838=CARTESIAN_POINT('Ctrl Pts',(-5.1999169413988,-31.5756924622445,2.63799288444814));
#60839=CARTESIAN_POINT('Ctrl Pts',(-4.82483322909613,-31.6371737406638,
3.23471700046071));
#60840=CARTESIAN_POINT('Ctrl Pts',(-4.19769542816151,-31.7240974424956,
3.93620747216806));
#60841=CARTESIAN_POINT('Ctrl Pts',(-3.96548585269262,-31.7543436363075,
4.15945687249389));
#60842=CARTESIAN_POINT('Ctrl Pts',(-3.46523412172557,-31.8128208486826,
4.56176656225472));
#60843=CARTESIAN_POINT('Ctrl Pts',(-3.19720624121618,-31.8409134064675,
4.74086471477473));
#60844=CARTESIAN_POINT('Ctrl Pts',(-2.52025087330818,-31.9034070081026,
5.12459397949763));
#60845=CARTESIAN_POINT('Ctrl Pts',(-2.03077060067128,-31.9395557904444,
5.32832509625205));
#60846=CARTESIAN_POINT('Ctrl Pts',(-1.01358478703292,-31.9879961748339,
5.59441429610713));
#60847=CARTESIAN_POINT('Ctrl Pts',(-0.485886980282349,-32.,5.65685424949238));
#60848=CARTESIAN_POINT('Ctrl Pts',(0.485886980282342,-32.,5.65685424949238));
#60849=CARTESIAN_POINT('Ctrl Pts',(1.01358478703292,-31.9879961748339,5.59441429610713));
#60850=CARTESIAN_POINT('Ctrl Pts',(2.03077060067128,-31.9395557904444,5.32832509625205));
#60851=CARTESIAN_POINT('Ctrl Pts',(2.52025087330817,-31.9034070081026,5.12459397949762));
#60852=CARTESIAN_POINT('Ctrl Pts',(3.19720624121618,-31.8409134064675,4.74086471477472));
#60853=CARTESIAN_POINT('Ctrl Pts',(3.46523412172556,-31.8128208486826,4.56176656225471));
#60854=CARTESIAN_POINT('Ctrl Pts',(3.96548585269262,-31.7543436363075,4.15945687249388));
#60855=CARTESIAN_POINT('Ctrl Pts',(4.19769542816151,-31.7240974424956,3.93620747216805));
#60856=CARTESIAN_POINT('Ctrl Pts',(4.82483322909612,-31.6371737406638,3.2347170004607));
#60857=CARTESIAN_POINT('Ctrl Pts',(5.1999169413988,-31.5756924622445,2.63799288444813));
#60858=CARTESIAN_POINT('Ctrl Pts',(5.69649663634414,-31.4898938042993,1.34576815070429));
#60859=CARTESIAN_POINT('Ctrl Pts',(5.81797979447237,-31.4666666666667,0.650190448083162));
#60860=CARTESIAN_POINT('Ctrl Pts',(5.81797979447237,-31.4666666666667,-1.38777878078145E-16));
#60861=CARTESIAN_POINT('',(-6.00000000000001,-30.,0.));
#60862=CARTESIAN_POINT('Origin',(-5.55111512312578E-15,-30.,0.));
#60863=CARTESIAN_POINT('',(-5.91850916286999E-15,-30.,6.));
#60864=CARTESIAN_POINT('Origin',(-5.55111512312578E-15,-30.,0.));
#60865=CARTESIAN_POINT('Origin',(-5.55111512312578E-15,-30.,0.));
#60866=CARTESIAN_POINT('Origin',(0.,0.,0.));
#60867=CARTESIAN_POINT('',(-10.6948150326157,-30.1599226029865,0.));
#60868=CARTESIAN_POINT('Origin',(0.,0.,0.));
#60869=CARTESIAN_POINT('Origin',(-15.,-25.9807621135332,0.));
#60870=CARTESIAN_POINT('Origin',(-15.,-25.9807621135332,0.));
#60871=CARTESIAN_POINT('',(-20.771851634051,-24.3419428085142,0.));
#60872=CARTESIAN_POINT('',(-18.6815416923826,-25.9807621134925,4.73774743599203));
#60873=CARTESIAN_POINT('Ctrl Pts',(-20.771851634051,-24.3419428085141,-1.38777878078145E-16));
#60874=CARTESIAN_POINT('Ctrl Pts',(-20.771851634051,-24.3419428085141,0.650190448083165));
#60875=CARTESIAN_POINT('Ctrl Pts',(-20.6782577017963,-24.4227996788253,
1.3457681507043));
#60876=CARTESIAN_POINT('Ctrl Pts',(-20.2911063999427,-24.7453933436892,
2.63799288444815));
#60877=CARTESIAN_POINT('Ctrl Pts',(-19.9970150157524,-24.9861795488087,
3.23471700046072));
#60878=CARTESIAN_POINT('Ctrl Pts',(-19.4973595993855,-25.3750265832533,
3.93620747216807));
#60879=CARTESIAN_POINT('Ctrl Pts',(-19.3113833049334,-25.5173253431967,
4.1594568724939));
#60880=CARTESIAN_POINT('Ctrl Pts',(-18.9716143273131,-25.7702804014673,
4.49781089377006));
#60881=CARTESIAN_POINT('Ctrl Pts',(-18.8265576304416,-25.8764879862695,
4.6250605042284));
#60882=CARTESIAN_POINT('Ctrl Pts',(-18.6815416923826,-25.9807621134518,
4.73774743599203));
#60883=CARTESIAN_POINT('Origin',(-15.,-25.9807621135332,0.));
#60884=CARTESIAN_POINT('Ctrl Pts',(-18.6815416923826,-25.9807621134518,
4.73774743599203));
#60885=CARTESIAN_POINT('Ctrl Pts',(-18.6139422249284,-26.0293697048732,
4.79027667297257));
#60886=CARTESIAN_POINT('Ctrl Pts',(-18.5463811126206,-26.0775460638188,
4.83968978042875));
#60887=CARTESIAN_POINT('Ctrl Pts',(-18.1343047842461,-26.3690354996372,
5.12459397949763));
#60888=CARTESIAN_POINT('Ctrl Pts',(-17.7284768246621,-26.6450813997796,
5.32832509625205));
#60889=CARTESIAN_POINT('Ctrl Pts',(-16.8717882618769,-27.1956249100491,
5.59441429610713));
#60890=CARTESIAN_POINT('Ctrl Pts',(-16.4207904682926,-27.4698694309609,
5.65685424949238));
#60891=CARTESIAN_POINT('Ctrl Pts',(-15.5792095317074,-27.9557564112432,
5.65685424949238));
#60892=CARTESIAN_POINT('Ctrl Pts',(-15.116207912957,-28.2092096970821,5.59441429610713));
#60893=CARTESIAN_POINT('Ctrl Pts',(-14.2110789657823,-28.6758520004508,
5.32832509625205));
#60894=CARTESIAN_POINT('Ctrl Pts',(-13.7691022238565,-28.8892863729454,
5.12459397949763));
#60895=CARTESIAN_POINT('Ctrl Pts',(-13.1515948772024,-29.1736430103094,
4.74086471477473));
#60896=CARTESIAN_POINT('Ctrl Pts',(-12.9054296448663,-29.2833280818651,
4.56176656225472));
#60897=CARTESIAN_POINT('Ctrl Pts',(-12.4429603313742,-29.4828111958893,
4.15945687249389));
#60898=CARTESIAN_POINT('Ctrl Pts',(-12.2267378431101,-29.5727220114149,
3.93620747216806));
#60899=CARTESIAN_POINT('Ctrl Pts',(-11.6401587249113,-29.8110127779048,
3.23471700046071));
#60900=CARTESIAN_POINT('Ctrl Pts',(-11.2845860623018,-29.945310285088,2.63799288444814));
#60901=CARTESIAN_POINT('Ctrl Pts',(-10.811636102503,-30.1192963151694,1.3457681507043));
#60902=CARTESIAN_POINT('Ctrl Pts',(-10.6948150326157,-30.1599226029865,
0.650190448083164));
#60903=CARTESIAN_POINT('Ctrl Pts',(-10.6948150326157,-30.1599226029865,
-2.77555756156289E-16));
#60904=CARTESIAN_POINT('',(-15.,-25.9807621135332,6.));
#60905=CARTESIAN_POINT('Origin',(-15.,-25.9807621135332,0.));
#60906=CARTESIAN_POINT('Origin',(0.,0.,0.));
#60907=CARTESIAN_POINT('',(-24.3419428085141,-20.771851634051,0.));
#60908=CARTESIAN_POINT('Origin',(0.,0.,0.));
#60909=CARTESIAN_POINT('Origin',(-25.9807621135332,-15.,0.));
#60910=CARTESIAN_POINT('Origin',(-25.9807621135332,-15.,0.));
#60911=CARTESIAN_POINT('',(-30.1599226029865,-10.6948150326157,0.));
#60912=CARTESIAN_POINT('',(-28.2665880502059,-14.9999999999993,5.54752195013542));
#60913=CARTESIAN_POINT('Ctrl Pts',(-30.1599226029865,-10.6948150326157,
4.16333634234434E-16));
#60914=CARTESIAN_POINT('Ctrl Pts',(-30.1599226029865,-10.6948150326157,
0.650190448083161));
#60915=CARTESIAN_POINT('Ctrl Pts',(-30.1192963151694,-10.811636102503,1.34576815070429));
#60916=CARTESIAN_POINT('Ctrl Pts',(-29.945310285088,-11.2845860623018,2.63799288444813));
#60917=CARTESIAN_POINT('Ctrl Pts',(-29.8110127779048,-11.6401587249113,
3.2347170004607));
#60918=CARTESIAN_POINT('Ctrl Pts',(-29.5727220114149,-12.2267378431101,
3.93620747216805));
#60919=CARTESIAN_POINT('Ctrl Pts',(-29.4828111958893,-12.4429603313741,
4.15945687249388));
#60920=CARTESIAN_POINT('Ctrl Pts',(-29.2833280818651,-12.9054296448663,
4.56176656225471));
#60921=CARTESIAN_POINT('Ctrl Pts',(-29.1736430103094,-13.1515948772024,
4.74086471477472));
#60922=CARTESIAN_POINT('Ctrl Pts',(-28.8892863729454,-13.7691022238565,
5.12459397949763));
#60923=CARTESIAN_POINT('Ctrl Pts',(-28.6758520004509,-14.2110789657823,
5.32832509625205));
#60924=CARTESIAN_POINT('Ctrl Pts',(-28.3849162461088,-14.7753963693311,
5.49422274745779));
#60925=CARTESIAN_POINT('Ctrl Pts',(-28.3261413561496,-14.8877754155893,
5.52298333765861));
#60926=CARTESIAN_POINT('Ctrl Pts',(-28.2665880502059,-14.9999999999986,
5.54752195013542));
#60927=CARTESIAN_POINT('Origin',(-25.9807621135332,-15.,0.));
#60928=CARTESIAN_POINT('Ctrl Pts',(-28.2665880502059,-14.9999999999986,
5.54752195013542));
#60929=CARTESIAN_POINT('Ctrl Pts',(-28.0849690614805,-15.3422499424251,
5.62235705646812));
#60930=CARTESIAN_POINT('Ctrl Pts',(-27.8957657393658,-15.6831164233792,
5.65685424949238));
#60931=CARTESIAN_POINT('Ctrl Pts',(-27.4698694309609,-16.4207904682926,
5.65685424949238));
#60932=CARTESIAN_POINT('Ctrl Pts',(-27.1956249100492,-16.8717882618769,
5.59441429610713));
#60933=CARTESIAN_POINT('Ctrl Pts',(-26.6450813997796,-17.7284768246621,
5.32832509625206));
#60934=CARTESIAN_POINT('Ctrl Pts',(-26.3690354996372,-18.1343047842461,
5.12459397949763));
#60935=CARTESIAN_POINT('Ctrl Pts',(-25.9764367690933,-18.6893185292651,
4.74086471477474));
#60936=CARTESIAN_POINT('Ctrl Pts',(-25.8180939601396,-18.9073912038163,
4.56176656225472));
#60937=CARTESIAN_POINT('Ctrl Pts',(-25.5173253431967,-19.3113833049333,
4.1594568724939));
#60938=CARTESIAN_POINT('Ctrl Pts',(-25.3750265832534,-19.4973595993854,
3.93620747216807));
#60939=CARTESIAN_POINT('Ctrl Pts',(-24.9861795488087,-19.9970150157524,
3.23471700046072));
#60940=CARTESIAN_POINT('Ctrl Pts',(-24.7453933436892,-20.2911063999427,
2.63799288444814));
#60941=CARTESIAN_POINT('Ctrl Pts',(-24.4227996788253,-20.6782577017963,
1.3457681507043));
#60942=CARTESIAN_POINT('Ctrl Pts',(-24.3419428085142,-20.771851634051,0.650190448083165));
#60943=CARTESIAN_POINT('Ctrl Pts',(-24.3419428085142,-20.771851634051,0.));
#60944=CARTESIAN_POINT('',(-25.9807621135332,-15.,6.00000000000001));
#60945=CARTESIAN_POINT('Origin',(-25.9807621135332,-15.,0.));
#60946=CARTESIAN_POINT('Origin',(0.,0.,0.));
#60947=CARTESIAN_POINT('',(-31.4666666666667,-5.81797979447235,0.));
#60948=CARTESIAN_POINT('Origin',(0.,0.,0.));
#60949=CARTESIAN_POINT('Origin',(-30.,3.67394039744206E-15,0.));
#60950=CARTESIAN_POINT('Origin',(-30.,3.67394039744206E-15,0.));
#60951=CARTESIAN_POINT('',(-31.4666666666667,5.81797979447236,0.));
#60952=CARTESIAN_POINT('',(-32.,-2.97773713326802E-16,5.65685424949238));
#60953=CARTESIAN_POINT('Ctrl Pts',(-31.4666666666667,5.81797979447238,0.));
#60954=CARTESIAN_POINT('Ctrl Pts',(-31.4666666666667,5.81797979447238,0.650190448083164));
#60955=CARTESIAN_POINT('Ctrl Pts',(-31.4898938042993,5.69649663634415,1.34576815070429));
#60956=CARTESIAN_POINT('Ctrl Pts',(-31.5756924622445,5.1999169413988,2.63799288444814));
#60957=CARTESIAN_POINT('Ctrl Pts',(-31.6371737406638,4.82483322909612,3.23471700046071));
#60958=CARTESIAN_POINT('Ctrl Pts',(-31.7240974424956,4.19769542816151,3.93620747216806));
#60959=CARTESIAN_POINT('Ctrl Pts',(-31.7543436363075,3.96548585269262,4.15945687249389));
#60960=CARTESIAN_POINT('Ctrl Pts',(-31.8128208486826,3.46523412172556,4.56176656225472));
#60961=CARTESIAN_POINT('Ctrl Pts',(-31.8409134064675,3.19720624121618,4.74086471477473));
#60962=CARTESIAN_POINT('Ctrl Pts',(-31.9034070081026,2.52025087330817,5.12459397949763));
#60963=CARTESIAN_POINT('Ctrl Pts',(-31.9395557904444,2.03077060067128,5.32832509625205));
#60964=CARTESIAN_POINT('Ctrl Pts',(-31.9879961748339,1.01358478703292,5.59441429610713));
#60965=CARTESIAN_POINT('Ctrl Pts',(-32.,0.485886980282341,5.65685424949238));
#60966=CARTESIAN_POINT('Ctrl Pts',(-32.,-4.44089209850063E-15,5.65685424949238));
#60967=CARTESIAN_POINT('Origin',(-30.,3.67394039744206E-15,0.));
#60968=CARTESIAN_POINT('Ctrl Pts',(-32.,-3.88578058618805E-15,5.65685424949238));
#60969=CARTESIAN_POINT('Ctrl Pts',(-32.,-0.485886980282349,5.65685424949238));
#60970=CARTESIAN_POINT('Ctrl Pts',(-31.9879961748339,-1.01358478703293,
5.59441429610713));
#60971=CARTESIAN_POINT('Ctrl Pts',(-31.9395557904444,-2.03077060067129,
5.32832509625205));
#60972=CARTESIAN_POINT('Ctrl Pts',(-31.9034070081026,-2.52025087330818,
5.12459397949762));
#60973=CARTESIAN_POINT('Ctrl Pts',(-31.8409134064675,-3.19720624121619,
4.74086471477472));
#60974=CARTESIAN_POINT('Ctrl Pts',(-31.8128208486826,-3.46523412172557,
4.56176656225471));
#60975=CARTESIAN_POINT('Ctrl Pts',(-31.7543436363075,-3.96548585269263,
4.15945687249388));
#60976=CARTESIAN_POINT('Ctrl Pts',(-31.7240974424956,-4.19769542816152,
3.93620747216804));
#60977=CARTESIAN_POINT('Ctrl Pts',(-31.6371737406638,-4.82483322909613,
3.2347170004607));
#60978=CARTESIAN_POINT('Ctrl Pts',(-31.5756924622445,-5.1999169413988,2.63799288444813));
#60979=CARTESIAN_POINT('Ctrl Pts',(-31.4898938042993,-5.69649663634414,
1.34576815070429));
#60980=CARTESIAN_POINT('Ctrl Pts',(-31.4666666666667,-5.81797979447238,
0.65019044808316));
#60981=CARTESIAN_POINT('Ctrl Pts',(-31.4666666666667,-5.81797979447238,
-1.38777878078145E-16));
#60982=CARTESIAN_POINT('',(-30.,3.67394039744206E-15,6.));
#60983=CARTESIAN_POINT('Origin',(-30.,3.67394039744206E-15,0.));
#60984=CARTESIAN_POINT('Origin',(0.,0.,0.));
#60985=CARTESIAN_POINT('',(-30.1599226029865,10.6948150326157,0.));
#60986=CARTESIAN_POINT('Origin',(0.,0.,0.));
#60987=CARTESIAN_POINT('Origin',(-25.9807621135332,15.,0.));
#60988=CARTESIAN_POINT('Origin',(-25.9807621135332,15.,0.));
#60989=CARTESIAN_POINT('',(-24.3419428085142,20.771851634051,0.));
#60990=CARTESIAN_POINT('',(-28.2665880502059,14.9999999999993,5.54752195013541));
#60991=CARTESIAN_POINT('Ctrl Pts',(-24.3419428085142,20.771851634051,0.));
#60992=CARTESIAN_POINT('Ctrl Pts',(-24.3419428085142,20.771851634051,0.650190448083166));
#60993=CARTESIAN_POINT('Ctrl Pts',(-24.4227996788253,20.6782577017963,1.3457681507043));
#60994=CARTESIAN_POINT('Ctrl Pts',(-24.7453933436892,20.2911063999427,2.63799288444814));
#60995=CARTESIAN_POINT('Ctrl Pts',(-24.9861795488087,19.9970150157524,3.23471700046072));
#60996=CARTESIAN_POINT('Ctrl Pts',(-25.3750265832534,19.4973595993854,3.93620747216807));
#60997=CARTESIAN_POINT('Ctrl Pts',(-25.5173253431967,19.3113833049333,4.1594568724939));
#60998=CARTESIAN_POINT('Ctrl Pts',(-25.8180939601396,18.9073912038163,4.56176656225472));
#60999=CARTESIAN_POINT('Ctrl Pts',(-25.9764367690933,18.6893185292651,4.74086471477473));
#61000=CARTESIAN_POINT('Ctrl Pts',(-26.3690354996372,18.1343047842461,5.12459397949763));
#61001=CARTESIAN_POINT('Ctrl Pts',(-26.6450813997796,17.7284768246621,5.32832509625206));
#61002=CARTESIAN_POINT('Ctrl Pts',(-27.1956249100492,16.8717882618769,5.59441429610713));
#61003=CARTESIAN_POINT('Ctrl Pts',(-27.4698694309609,16.4207904682926,5.65685424949238));
#61004=CARTESIAN_POINT('Ctrl Pts',(-27.8957657393658,15.6831164233792,5.65685424949238));
#61005=CARTESIAN_POINT('Ctrl Pts',(-28.0849690614805,15.3422499424251,5.62235705646811));
#61006=CARTESIAN_POINT('Ctrl Pts',(-28.2665880502059,14.9999999999986,5.54752195013541));
#61007=CARTESIAN_POINT('Origin',(-25.9807621135332,15.,0.));
#61008=CARTESIAN_POINT('Ctrl Pts',(-28.2665880502059,14.9999999999986,5.54752195013541));
#61009=CARTESIAN_POINT('Ctrl Pts',(-28.3261413561496,14.8877754155893,5.52298333765861));
#61010=CARTESIAN_POINT('Ctrl Pts',(-28.3849162461088,14.7753963693311,5.49422274745778));
#61011=CARTESIAN_POINT('Ctrl Pts',(-28.6758520004509,14.2110789657823,5.32832509625205));
#61012=CARTESIAN_POINT('Ctrl Pts',(-28.8892863729454,13.7691022238565,5.12459397949762));
#61013=CARTESIAN_POINT('Ctrl Pts',(-29.1736430103094,13.1515948772024,4.74086471477472));
#61014=CARTESIAN_POINT('Ctrl Pts',(-29.2833280818651,12.9054296448663,4.56176656225471));
#61015=CARTESIAN_POINT('Ctrl Pts',(-29.4828111958893,12.4429603313741,4.15945687249387));
#61016=CARTESIAN_POINT('Ctrl Pts',(-29.5727220114149,12.2267378431101,3.93620747216804));
#61017=CARTESIAN_POINT('Ctrl Pts',(-29.8110127779048,11.6401587249113,3.23471700046069));
#61018=CARTESIAN_POINT('Ctrl Pts',(-29.945310285088,11.2845860623018,2.63799288444812));
#61019=CARTESIAN_POINT('Ctrl Pts',(-30.1192963151694,10.811636102503,1.34576815070429));
#61020=CARTESIAN_POINT('Ctrl Pts',(-30.1599226029865,10.6948150326157,0.650190448083159));
#61021=CARTESIAN_POINT('Ctrl Pts',(-30.1599226029865,10.6948150326157,-5.55111512312578E-16));
#61022=CARTESIAN_POINT('',(-25.9807621135332,15.,6.));
#61023=CARTESIAN_POINT('Origin',(-25.9807621135332,15.,0.));
#61024=CARTESIAN_POINT('Origin',(0.,0.,0.));
#61025=CARTESIAN_POINT('',(-20.771851634051,24.3419428085142,0.));
#61026=CARTESIAN_POINT('Origin',(0.,0.,0.));
#61027=CARTESIAN_POINT('Origin',(-15.,25.9807621135332,0.));
#61028=CARTESIAN_POINT('Origin',(-15.,25.9807621135332,0.));
#61029=CARTESIAN_POINT('',(-10.6948150326157,30.1599226029865,0.));
#61030=CARTESIAN_POINT('',(-18.6815416923826,25.9807621134925,4.73774743599202));
#61031=CARTESIAN_POINT('Ctrl Pts',(-10.6948150326157,30.1599226029865,-1.38777878078145E-16));
#61032=CARTESIAN_POINT('Ctrl Pts',(-10.6948150326157,30.1599226029865,0.650190448083162));
#61033=CARTESIAN_POINT('Ctrl Pts',(-10.811636102503,30.1192963151694,1.34576815070429));
#61034=CARTESIAN_POINT('Ctrl Pts',(-11.2845860623018,29.945310285088,2.63799288444813));
#61035=CARTESIAN_POINT('Ctrl Pts',(-11.6401587249113,29.8110127779048,3.2347170004607));
#61036=CARTESIAN_POINT('Ctrl Pts',(-12.2267378431101,29.5727220114149,3.93620747216805));
#61037=CARTESIAN_POINT('Ctrl Pts',(-12.4429603313741,29.4828111958893,4.15945687249388));
#61038=CARTESIAN_POINT('Ctrl Pts',(-12.9054296448663,29.2833280818651,4.56176656225471));
#61039=CARTESIAN_POINT('Ctrl Pts',(-13.1515948772024,29.1736430103094,4.74086471477472));
#61040=CARTESIAN_POINT('Ctrl Pts',(-13.7691022238565,28.8892863729454,5.12459397949762));
#61041=CARTESIAN_POINT('Ctrl Pts',(-14.2110789657823,28.6758520004509,5.32832509625205));
#61042=CARTESIAN_POINT('Ctrl Pts',(-15.116207912957,28.2092096970821,5.59441429610713));
#61043=CARTESIAN_POINT('Ctrl Pts',(-15.5792095317074,27.9557564112432,5.65685424949238));
#61044=CARTESIAN_POINT('Ctrl Pts',(-16.4207904682926,27.4698694309609,5.65685424949238));
#61045=CARTESIAN_POINT('Ctrl Pts',(-16.8717882618769,27.1956249100492,5.59441429610713));
#61046=CARTESIAN_POINT('Ctrl Pts',(-17.7284768246621,26.6450813997796,5.32832509625206));
#61047=CARTESIAN_POINT('Ctrl Pts',(-18.1343047842461,26.3690354996372,5.12459397949763));
#61048=CARTESIAN_POINT('Ctrl Pts',(-18.5463811126206,26.0775460638188,4.83968978042875));
#61049=CARTESIAN_POINT('Ctrl Pts',(-18.6139422249284,26.0293697048732,4.79027667297257));
#61050=CARTESIAN_POINT('Ctrl Pts',(-18.6815416923826,25.9807621134518,4.73774743599202));
#61051=CARTESIAN_POINT('Origin',(-15.,25.9807621135332,0.));
#61052=CARTESIAN_POINT('Ctrl Pts',(-18.6815416923826,25.9807621134518,4.73774743599202));
#61053=CARTESIAN_POINT('Ctrl Pts',(-18.8265576304416,25.8764879862695,4.6250605042284));
#61054=CARTESIAN_POINT('Ctrl Pts',(-18.9716143273131,25.7702804014673,4.49781089377006));
#61055=CARTESIAN_POINT('Ctrl Pts',(-19.3113833049333,25.5173253431967,4.1594568724939));
#61056=CARTESIAN_POINT('Ctrl Pts',(-19.4973595993854,25.3750265832534,3.93620747216807));
#61057=CARTESIAN_POINT('Ctrl Pts',(-19.9970150157524,24.9861795488087,3.23471700046072));
#61058=CARTESIAN_POINT('Ctrl Pts',(-20.2911063999427,24.7453933436892,2.63799288444815));
#61059=CARTESIAN_POINT('Ctrl Pts',(-20.6782577017962,24.4227996788253,1.3457681507043));
#61060=CARTESIAN_POINT('Ctrl Pts',(-20.771851634051,24.3419428085142,0.650190448083167));
#61061=CARTESIAN_POINT('Ctrl Pts',(-20.771851634051,24.3419428085142,-4.16333634234434E-16));
#61062=CARTESIAN_POINT('',(-15.,25.9807621135332,6.));
#61063=CARTESIAN_POINT('Origin',(-15.,25.9807621135332,0.));
#61064=CARTESIAN_POINT('Origin',(0.,0.,0.));
#61065=CARTESIAN_POINT('',(-5.81797979447235,31.4666666666667,0.));
#61066=CARTESIAN_POINT('Origin',(0.,0.,0.));
#61067=CARTESIAN_POINT('',(-6.,30.,0.));
#61068=CARTESIAN_POINT('Origin',(1.66533453693773E-15,30.,0.));
#61069=CARTESIAN_POINT('Origin',(1.66533453693773E-15,30.,0.));
#61070=CARTESIAN_POINT('Origin',(1.66533453693773E-15,30.,5.55111512312578E-16));
#61071=CARTESIAN_POINT('',(5.81797979447236,31.4666666666667,0.));
#61072=CARTESIAN_POINT('Ctrl Pts',(5.81797979447238,31.4666666666667,5.55111512312578E-16));
#61073=CARTESIAN_POINT('Ctrl Pts',(5.81797979447238,31.4666666666667,0.650190448083162));
#61074=CARTESIAN_POINT('Ctrl Pts',(5.69649663634414,31.4898938042992,1.34576815070429));
#61075=CARTESIAN_POINT('Ctrl Pts',(5.1999169413988,31.5756924622445,2.63799288444813));
#61076=CARTESIAN_POINT('Ctrl Pts',(4.82483322909613,31.6371737406637,3.2347170004607));
#61077=CARTESIAN_POINT('Ctrl Pts',(4.19769542816151,31.7240974424956,3.93620747216805));
#61078=CARTESIAN_POINT('Ctrl Pts',(3.96548585269263,31.7543436363075,4.15945687249388));
#61079=CARTESIAN_POINT('Ctrl Pts',(3.46523412172557,31.8128208486826,4.56176656225471));
#61080=CARTESIAN_POINT('Ctrl Pts',(3.19720624121618,31.8409134064675,4.74086471477472));
#61081=CARTESIAN_POINT('Ctrl Pts',(2.52025087330818,31.9034070081026,5.12459397949762));
#61082=CARTESIAN_POINT('Ctrl Pts',(2.03077060067129,31.9395557904444,5.32832509625205));
#61083=CARTESIAN_POINT('Ctrl Pts',(1.01358478703293,31.9879961748339,5.59441429610713));
#61084=CARTESIAN_POINT('Ctrl Pts',(0.485886980282349,32.,5.65685424949238));
#61085=CARTESIAN_POINT('Ctrl Pts',(-0.485886980282345,32.,5.65685424949238));
#61086=CARTESIAN_POINT('Ctrl Pts',(-1.01358478703292,31.9879961748339,5.59441429610713));
#61087=CARTESIAN_POINT('Ctrl Pts',(-2.03077060067128,31.9395557904444,5.32832509625205));
#61088=CARTESIAN_POINT('Ctrl Pts',(-2.52025087330818,31.9034070081026,5.12459397949762));
#61089=CARTESIAN_POINT('Ctrl Pts',(-3.19720624121618,31.8409134064675,4.74086471477472));
#61090=CARTESIAN_POINT('Ctrl Pts',(-3.46523412172557,31.8128208486826,4.56176656225471));
#61091=CARTESIAN_POINT('Ctrl Pts',(-3.96548585269262,31.7543436363075,4.15945687249388));
#61092=CARTESIAN_POINT('Ctrl Pts',(-4.19769542816151,31.7240974424956,3.93620747216805));
#61093=CARTESIAN_POINT('Ctrl Pts',(-4.82483322909612,31.6371737406638,3.23471700046071));
#61094=CARTESIAN_POINT('Ctrl Pts',(-5.1999169413988,31.5756924622445,2.63799288444813));
#61095=CARTESIAN_POINT('Ctrl Pts',(-5.69649663634414,31.4898938042993,1.34576815070429));
#61096=CARTESIAN_POINT('Ctrl Pts',(-5.81797979447238,31.4666666666667,0.650190448083163));
#61097=CARTESIAN_POINT('Ctrl Pts',(-5.81797979447238,31.4666666666667,1.38777878078145E-16));
#61098=CARTESIAN_POINT('Origin',(1.66533453693773E-15,30.,0.));
#61099=CARTESIAN_POINT('',(1.29794049719353E-15,30.,6.));
#61100=CARTESIAN_POINT('Origin',(1.66533453693773E-15,30.,5.55111512312578E-16));
#61101=CARTESIAN_POINT('Origin',(0.,0.,0.));
#61102=CARTESIAN_POINT('',(10.6948150326157,30.1599226029865,0.));
#61103=CARTESIAN_POINT('Origin',(0.,0.,0.));
#61104=CARTESIAN_POINT('Origin',(15.,25.9807621135332,0.));
#61105=CARTESIAN_POINT('Origin',(15.,25.9807621135332,0.));
#61106=CARTESIAN_POINT('',(20.771851634051,24.3419428085142,0.));
#61107=CARTESIAN_POINT('Ctrl Pts',(20.771851634051,24.3419428085141,-5.55111512312578E-16));
#61108=CARTESIAN_POINT('Ctrl Pts',(20.771851634051,24.3419428085141,0.650190448083163));
#61109=CARTESIAN_POINT('Ctrl Pts',(20.6782577017963,24.4227996788253,1.34576815070429));
#61110=CARTESIAN_POINT('Ctrl Pts',(20.2911063999427,24.7453933436892,2.63799288444813));
#61111=CARTESIAN_POINT('Ctrl Pts',(19.9970150157524,24.9861795488087,3.23471700046071));
#61112=CARTESIAN_POINT('Ctrl Pts',(19.4973595993855,25.3750265832533,3.93620747216806));
#61113=CARTESIAN_POINT('Ctrl Pts',(19.3113833049334,25.5173253431967,4.15945687249388));
#61114=CARTESIAN_POINT('Ctrl Pts',(18.9073912038163,25.8180939601395,4.56176656225471));
#61115=CARTESIAN_POINT('Ctrl Pts',(18.6893185292651,25.9764367690933,4.74086471477473));
#61116=CARTESIAN_POINT('Ctrl Pts',(18.1343047842461,26.3690354996372,5.12459397949762));
#61117=CARTESIAN_POINT('Ctrl Pts',(17.7284768246621,26.6450813997796,5.32832509625205));
#61118=CARTESIAN_POINT('Ctrl Pts',(16.8717882618769,27.1956249100491,5.59441429610713));
#61119=CARTESIAN_POINT('Ctrl Pts',(16.4207904682926,27.4698694309609,5.65685424949238));
#61120=CARTESIAN_POINT('Ctrl Pts',(15.5792095317074,27.9557564112432,5.65685424949238));
#61121=CARTESIAN_POINT('Ctrl Pts',(15.116207912957,28.2092096970821,5.59441429610713));
#61122=CARTESIAN_POINT('Ctrl Pts',(14.2110789657823,28.6758520004508,5.32832509625205));
#61123=CARTESIAN_POINT('Ctrl Pts',(13.7691022238565,28.8892863729454,5.12459397949763));
#61124=CARTESIAN_POINT('Ctrl Pts',(13.1515948772024,29.1736430103094,4.74086471477473));
#61125=CARTESIAN_POINT('Ctrl Pts',(12.9054296448663,29.2833280818651,4.56176656225472));
#61126=CARTESIAN_POINT('Ctrl Pts',(12.4429603313741,29.4828111958893,4.15945687249389));
#61127=CARTESIAN_POINT('Ctrl Pts',(12.2267378431101,29.5727220114149,3.93620747216806));
#61128=CARTESIAN_POINT('Ctrl Pts',(11.6401587249113,29.8110127779048,3.23471700046071));
#61129=CARTESIAN_POINT('Ctrl Pts',(11.2845860623018,29.945310285088,2.63799288444813));
#61130=CARTESIAN_POINT('Ctrl Pts',(10.811636102503,30.1192963151694,1.34576815070429));
#61131=CARTESIAN_POINT('Ctrl Pts',(10.6948150326157,30.1599226029865,0.650190448083163));
#61132=CARTESIAN_POINT('Ctrl Pts',(10.6948150326157,30.1599226029865,1.38777878078145E-16));
#61133=CARTESIAN_POINT('Origin',(15.,25.9807621135332,0.));
#61134=CARTESIAN_POINT('',(15.,25.9807621135332,6.));
#61135=CARTESIAN_POINT('Origin',(15.,25.9807621135332,0.));
#61136=CARTESIAN_POINT('Origin',(0.,0.,0.));
#61137=CARTESIAN_POINT('',(24.3419428085142,20.771851634051,0.));
#61138=CARTESIAN_POINT('Origin',(0.,0.,0.));
#61139=CARTESIAN_POINT('Origin',(25.9807621135332,15.,0.));
#61140=CARTESIAN_POINT('Origin',(25.9807621135332,15.,0.));
#61141=CARTESIAN_POINT('',(30.1599226029865,10.6948150326157,0.));
#61142=CARTESIAN_POINT('Ctrl Pts',(30.1599226029865,10.6948150326157,-4.16333634234434E-16));
#61143=CARTESIAN_POINT('Ctrl Pts',(30.1599226029865,10.6948150326157,0.650190448083162));
#61144=CARTESIAN_POINT('Ctrl Pts',(30.1192963151694,10.811636102503,1.34576815070429));
#61145=CARTESIAN_POINT('Ctrl Pts',(29.945310285088,11.2845860623018,2.63799288444813));
#61146=CARTESIAN_POINT('Ctrl Pts',(29.8110127779048,11.6401587249113,3.23471700046071));
#61147=CARTESIAN_POINT('Ctrl Pts',(29.5727220114149,12.2267378431101,3.93620747216805));
#61148=CARTESIAN_POINT('Ctrl Pts',(29.4828111958893,12.4429603313741,4.15945687249388));
#61149=CARTESIAN_POINT('Ctrl Pts',(29.2833280818651,12.9054296448663,4.56176656225471));
#61150=CARTESIAN_POINT('Ctrl Pts',(29.1736430103094,13.1515948772024,4.74086471477472));
#61151=CARTESIAN_POINT('Ctrl Pts',(28.8892863729454,13.7691022238565,5.12459397949762));
#61152=CARTESIAN_POINT('Ctrl Pts',(28.6758520004509,14.2110789657823,5.32832509625205));
#61153=CARTESIAN_POINT('Ctrl Pts',(28.2092096970821,15.116207912957,5.59441429610713));
#61154=CARTESIAN_POINT('Ctrl Pts',(27.9557564112432,15.5792095317074,5.65685424949238));
#61155=CARTESIAN_POINT('Ctrl Pts',(27.4698694309609,16.4207904682926,5.65685424949238));
#61156=CARTESIAN_POINT('Ctrl Pts',(27.1956249100492,16.8717882618769,5.59441429610713));
#61157=CARTESIAN_POINT('Ctrl Pts',(26.6450813997796,17.7284768246621,5.32832509625205));
#61158=CARTESIAN_POINT('Ctrl Pts',(26.3690354996372,18.1343047842461,5.12459397949763));
#61159=CARTESIAN_POINT('Ctrl Pts',(25.9764367690933,18.6893185292651,4.74086471477473));
#61160=CARTESIAN_POINT('Ctrl Pts',(25.8180939601396,18.9073912038163,4.56176656225471));
#61161=CARTESIAN_POINT('Ctrl Pts',(25.5173253431967,19.3113833049334,4.15945687249389));
#61162=CARTESIAN_POINT('Ctrl Pts',(25.3750265832534,19.4973595993854,3.93620747216806));
#61163=CARTESIAN_POINT('Ctrl Pts',(24.9861795488087,19.9970150157524,3.23471700046071));
#61164=CARTESIAN_POINT('Ctrl Pts',(24.7453933436892,20.2911063999427,2.63799288444814));
#61165=CARTESIAN_POINT('Ctrl Pts',(24.4227996788253,20.6782577017963,1.34576815070429));
#61166=CARTESIAN_POINT('Ctrl Pts',(24.3419428085142,20.771851634051,0.650190448083164));
#61167=CARTESIAN_POINT('Ctrl Pts',(24.3419428085142,20.771851634051,-2.77555756156289E-16));
#61168=CARTESIAN_POINT('Origin',(25.9807621135332,15.,0.));
#61169=CARTESIAN_POINT('',(25.9807621135332,15.,6.));
#61170=CARTESIAN_POINT('Origin',(25.9807621135332,15.,0.));
#61171=CARTESIAN_POINT('Origin',(0.,0.,0.));
#61172=CARTESIAN_POINT('',(31.4666666666667,5.81797979447236,0.));
#61173=CARTESIAN_POINT('Origin',(0.,0.,0.));
#61174=CARTESIAN_POINT('Origin',(30.,0.,0.));
#61175=CARTESIAN_POINT('Origin',(30.,0.,0.));
#61176=CARTESIAN_POINT('',(31.4666666666667,-5.81797979447236,0.));
#61177=CARTESIAN_POINT('Ctrl Pts',(31.4666666666667,-5.81797979447238,1.38777878078145E-16));
#61178=CARTESIAN_POINT('Ctrl Pts',(31.4666666666667,-5.81797979447238,0.650190448083163));
#61179=CARTESIAN_POINT('Ctrl Pts',(31.4898938042993,-5.69649663634414,1.34576815070429));
#61180=CARTESIAN_POINT('Ctrl Pts',(31.5756924622445,-5.1999169413988,2.63799288444813));
#61181=CARTESIAN_POINT('Ctrl Pts',(31.6371737406638,-4.82483322909612,3.23471700046071));
#61182=CARTESIAN_POINT('Ctrl Pts',(31.7240974424956,-4.19769542816151,3.93620747216806));
#61183=CARTESIAN_POINT('Ctrl Pts',(31.7543436363075,-3.96548585269262,4.15945687249389));
#61184=CARTESIAN_POINT('Ctrl Pts',(31.8128208486826,-3.46523412172556,4.56176656225471));
#61185=CARTESIAN_POINT('Ctrl Pts',(31.8409134064675,-3.19720624121618,4.74086471477473));
#61186=CARTESIAN_POINT('Ctrl Pts',(31.9034070081026,-2.52025087330817,5.12459397949763));
#61187=CARTESIAN_POINT('Ctrl Pts',(31.9395557904444,-2.03077060067128,5.32832509625205));
#61188=CARTESIAN_POINT('Ctrl Pts',(31.9879961748339,-1.01358478703292,5.59441429610713));
#61189=CARTESIAN_POINT('Ctrl Pts',(32.,-0.485886980282346,5.65685424949238));
#61190=CARTESIAN_POINT('Ctrl Pts',(32.,0.485886980282346,5.65685424949238));
#61191=CARTESIAN_POINT('Ctrl Pts',(31.9879961748339,1.01358478703292,5.59441429610713));
#61192=CARTESIAN_POINT('Ctrl Pts',(31.9395557904444,2.03077060067128,5.32832509625205));
#61193=CARTESIAN_POINT('Ctrl Pts',(31.9034070081026,2.52025087330817,5.12459397949763));
#61194=CARTESIAN_POINT('Ctrl Pts',(31.8409134064675,3.19720624121618,4.74086471477473));
#61195=CARTESIAN_POINT('Ctrl Pts',(31.8128208486826,3.46523412172556,4.56176656225471));
#61196=CARTESIAN_POINT('Ctrl Pts',(31.7543436363075,3.96548585269262,4.15945687249389));
#61197=CARTESIAN_POINT('Ctrl Pts',(31.7240974424956,4.19769542816151,3.93620747216806));
#61198=CARTESIAN_POINT('Ctrl Pts',(31.6371737406638,4.82483322909612,3.23471700046071));
#61199=CARTESIAN_POINT('Ctrl Pts',(31.5756924622445,5.1999169413988,2.63799288444813));
#61200=CARTESIAN_POINT('Ctrl Pts',(31.4898938042993,5.69649663634414,1.34576815070429));
#61201=CARTESIAN_POINT('Ctrl Pts',(31.4666666666667,5.81797979447238,0.650190448083162));
#61202=CARTESIAN_POINT('Ctrl Pts',(31.4666666666667,5.81797979447238,-2.77555756156289E-16));
#61203=CARTESIAN_POINT('Origin',(30.,0.,0.));
#61204=CARTESIAN_POINT('',(30.,-4.49927934798557E-32,6.));
#61205=CARTESIAN_POINT('Origin',(30.,0.,0.));
#61206=CARTESIAN_POINT('Origin',(0.,0.,0.));
#61207=CARTESIAN_POINT('',(-32.,-3.91886975727153E-15,8.));
#61208=CARTESIAN_POINT('Origin',(0.,0.,8.));
#61209=CARTESIAN_POINT('',(-32.,-3.91886975727153E-15,0.));
#61210=CARTESIAN_POINT('Origin',(0.,0.,0.));
#61211=CARTESIAN_POINT('Origin',(0.,0.,8.));
#61212=CARTESIAN_POINT('Origin',(0.,0.,0.));
#61213=CARTESIAN_POINT('',(0.,0.,0.));
#61214=CARTESIAN_POINT('Origin',(0.,0.,0.));
#61215=CARTESIAN_POINT('',(-6.,-7.34788079488412E-16,2.));
#61216=CARTESIAN_POINT('Origin',(0.,0.,2.));
#61217=CARTESIAN_POINT('',(-6.,-7.34788079488412E-16,0.));
#61218=CARTESIAN_POINT('',(-6.,-7.34788079488412E-16,0.));
#61219=CARTESIAN_POINT('Origin',(0.,0.,0.));
#61220=CARTESIAN_POINT('Origin',(0.,0.,0.));
#61221=CARTESIAN_POINT('',(-12.,-1.46957615897682E-15,2.));
#61222=CARTESIAN_POINT('Origin',(0.,0.,2.));
#61223=CARTESIAN_POINT('',(-12.,-1.46957615897682E-15,0.));
#61224=CARTESIAN_POINT('',(-12.,-1.46957615897682E-15,0.));
#61225=CARTESIAN_POINT('Origin',(0.,0.,0.));
#61226=CARTESIAN_POINT('Origin',(0.,0.,2.));
#61227=CARTESIAN_POINT('Origin',(0.,0.,0.));
#61228=CARTESIAN_POINT('',(0.,0.,0.));
#61229=CARTESIAN_POINT('Origin',(0.,0.,0.));
#61230=CARTESIAN_POINT('',(-1.95633559071744,0.0012731057411345,0.225869692124231));
#61231=CARTESIAN_POINT('',(-1.95587799559821,0.00207186393275607,0.124130307875758));
#61232=CARTESIAN_POINT('',(-1.954,-2.39295984553393E-16,0.));
#61233=CARTESIAN_POINT('',(0.861525859670522,1.75382131162755,0.));
#61234=CARTESIAN_POINT('Ctrl Pts',(-1.95633559071744,0.0012731057411345,
0.225869692124231));
#61235=CARTESIAN_POINT('Ctrl Pts',(-1.95680032440099,0.0682557629313676,
0.222037301306047));
#61236=CARTESIAN_POINT('Ctrl Pts',(-1.95365903766855,0.135191473590706,
0.218204910487863));
#61237=CARTESIAN_POINT('Ctrl Pts',(-1.94676806606145,0.201735328972743,
0.214372519669679));
#61238=CARTESIAN_POINT('Ctrl Pts',(-1.88017193281744,0.844832371344698,
0.1773353028412));
#61239=CARTESIAN_POINT('Ctrl Pts',(-1.46336311091822,1.45133095416213,0.140298086012721));
#61240=CARTESIAN_POINT('Ctrl Pts',(-0.886884671668765,1.7445317403525,0.103260869184242));
#61241=CARTESIAN_POINT('Ctrl Pts',(-0.351138290053491,2.01701592986141,
0.0688405794561611));
#61242=CARTESIAN_POINT('Ctrl Pts',(0.322511385444639,2.01891139473935,0.0344202897280807));
#61243=CARTESIAN_POINT('Ctrl Pts',(0.863567639152679,1.75641488315944,2.92734586571086E-17));
#61244=CARTESIAN_POINT('',(-0.861525859670574,1.75382131162752,1.38777878078145E-16));
#61245=CARTESIAN_POINT('Origin',(0.,0.,0.));
#61246=CARTESIAN_POINT('Ctrl Pts',(-0.861525859670571,1.75382131162752,
2.28983498828939E-15));
#61247=CARTESIAN_POINT('Ctrl Pts',(-1.44496782441851,1.46721837385109,0.0370621399437224));
#61248=CARTESIAN_POINT('Ctrl Pts',(-1.8691020329229,0.869083656944534,0.0741242798874424));
#61249=CARTESIAN_POINT('Ctrl Pts',(-1.94380023116171,0.227435527544788,
0.111186419831163));
#61250=CARTESIAN_POINT('Ctrl Pts',(-1.95249630318745,0.152737362394887,
0.115501049179361));
#61251=CARTESIAN_POINT('Ctrl Pts',(-1.95645657185248,0.0774494727773659,
0.119815678527559));
#61252=CARTESIAN_POINT('Ctrl Pts',(-1.95587799559821,0.00207186393275607,
0.124130307875758));
#61253=CARTESIAN_POINT('Origin',(0.,0.,0.));
#61254=CARTESIAN_POINT('',(-1.95128203910989,0.000979727872364722,0.92586969212423));
#61255=CARTESIAN_POINT('',(-1.95118672945361,0.000916100096969453,0.824130307875757));
#61256=CARTESIAN_POINT('',(-1.954,-2.39295984553393E-16,0.));
#61257=CARTESIAN_POINT('Ctrl Pts',(-1.95128203910989,0.000979727872364722,
0.92586969212423));
#61258=CARTESIAN_POINT('Ctrl Pts',(-1.9524730612105,0.263901717292074,0.910927268943587));
#61259=CARTESIAN_POINT('Ctrl Pts',(-1.90305141123492,0.526394079969068,
0.895984845762944));
#61260=CARTESIAN_POINT('Ctrl Pts',(-1.80089049647467,0.766440059940591,
0.881042422582301));
#61261=CARTESIAN_POINT('Ctrl Pts',(-1.54766811710363,1.36143291361156,0.844005205753822));
#61262=CARTESIAN_POINT('Ctrl Pts',(-0.970428066964404,1.81852045762203,
0.806967988925342));
#61263=CARTESIAN_POINT('Ctrl Pts',(-0.333230591869142,1.92861999489257,
0.769930772096863));
#61264=CARTESIAN_POINT('Ctrl Pts',(0.30396688322612,2.0387195321631,0.732893555268385));
#61265=CARTESIAN_POINT('Ctrl Pts',(1.00112178327742,1.8018310626937,0.695856338439906));
#61266=CARTESIAN_POINT('Ctrl Pts',(1.43930998255098,1.32629143144902,0.658819121611426));
#61267=CARTESIAN_POINT('Ctrl Pts',(1.87749818182454,0.850751800204341,0.621781904782947));
#61268=CARTESIAN_POINT('Ctrl Pts',(2.05671968032037,0.136561007184397,0.584744687954468));
#61269=CARTESIAN_POINT('Ctrl Pts',(1.89499805994521,-0.489512382298273,
0.547707471125989));
#61270=CARTESIAN_POINT('Ctrl Pts',(1.73327643957006,-1.11558577178094,0.51067025429751));
#61271=CARTESIAN_POINT('Ctrl Pts',(1.23061170032392,-1.65354175772633,0.473633037469032));
#61272=CARTESIAN_POINT('Ctrl Pts',(0.616932989107385,-1.8573955796291,0.436595820640553));
#61273=CARTESIAN_POINT('Ctrl Pts',(0.00325427789084558,-2.06124940153187,
0.399558603812074));
#61274=CARTESIAN_POINT('Ctrl Pts',(-0.721438405296094,-1.93100105939202,
0.362521386983595));
#61275=CARTESIAN_POINT('Ctrl Pts',(-1.22559302459517,-1.52602913735885,
0.325484170155115));
#61276=CARTESIAN_POINT('Ctrl Pts',(-1.67758072371516,-1.1629613001496,0.29227934414482));
#61277=CARTESIAN_POINT('Ctrl Pts',(-1.95230901779331,-0.579081973692791,
0.259074518134526));
#61278=CARTESIAN_POINT('Ctrl Pts',(-1.95633559071744,0.0012731057411345,
0.225869692124231));
#61279=CARTESIAN_POINT('Ctrl Pts',(-1.95587799559821,0.00207186393275607,
0.124130307875758));
#61280=CARTESIAN_POINT('Ctrl Pts',(-1.95148667238412,-0.570034995103637,
0.15687781847128));
#61281=CARTESIAN_POINT('Ctrl Pts',(-1.68562951923343,-1.14731024226281,
0.189625329066803));
#61282=CARTESIAN_POINT('Ctrl Pts',(-1.2444215732779,-1.51113938431406,0.222372839662326));
#61283=CARTESIAN_POINT('Ctrl Pts',(-0.745082529182101,-1.92290462488019,
0.259434979606046));
#61284=CARTESIAN_POINT('Ctrl Pts',(-0.0211422530173012,-2.0612735641195,
0.296497119549767));
#61285=CARTESIAN_POINT('Ctrl Pts',(0.595334795120667,-1.86428772433344,
0.333559259493488));
#61286=CARTESIAN_POINT('Ctrl Pts',(1.21181184325864,-1.66730188454737,0.370621399437209));
#61287=CARTESIAN_POINT('Ctrl Pts',(1.72082566336977,-1.13496126573593,0.40768353938093));
#61288=CARTESIAN_POINT('Ctrl Pts',(1.8894870924304,-0.510370283185346,0.444745679324651));
#61289=CARTESIAN_POINT('Ctrl Pts',(2.05814852149104,0.114220699365238,0.481807819268372));
#61290=CARTESIAN_POINT('Ctrl Pts',(1.88645755950116,0.831062045654966,0.518869959212093));
#61291=CARTESIAN_POINT('Ctrl Pts',(1.45292142815886,1.31145007703775,0.555932099155814));
#61292=CARTESIAN_POINT('Ctrl Pts',(1.01938529681656,1.79183810842053,0.592994239099535));
#61293=CARTESIAN_POINT('Ctrl Pts',(0.324003996121834,2.03577282489637,0.630056379043256));
#61294=CARTESIAN_POINT('Ctrl Pts',(-0.314654015224673,1.93172336479658,
0.667118518986976));
#61295=CARTESIAN_POINT('Ctrl Pts',(-0.953312026571179,1.8276739046968,0.704180658930697));
#61296=CARTESIAN_POINT('Ctrl Pts',(-1.53524674856946,1.37564026802139,0.741242798874417));
#61297=CARTESIAN_POINT('Ctrl Pts',(-1.79395555636014,0.782560471576942,
0.778304938818138));
#61298=CARTESIAN_POINT('Ctrl Pts',(-1.90058212652462,0.538123240897563,
0.793580061837345));
#61299=CARTESIAN_POINT('Ctrl Pts',(-1.95230335199157,0.269726953471863,
0.808855184856551));
#61300=CARTESIAN_POINT('Ctrl Pts',(-1.95118672945361,0.000916100096969453,
0.824130307875757));
#61301=CARTESIAN_POINT('Origin',(0.,0.,0.));
#61302=CARTESIAN_POINT('',(-1.95279554503994,-0.00168121501241181,1.62586969212423));
#61303=CARTESIAN_POINT('',(-1.95287184048439,-0.001702989282844,1.52413030787576));
#61304=CARTESIAN_POINT('',(-1.954,-2.39295984553393E-16,0.));
#61305=CARTESIAN_POINT('Ctrl Pts',(-1.95279554503994,-0.00168121501241181,
1.62586969212423));
#61306=CARTESIAN_POINT('Ctrl Pts',(-1.94903656010943,0.455834752155161,
1.59981723658113));
#61307=CARTESIAN_POINT('Ctrl Pts',(-1.78856730317397,0.91572573117829,1.57376478103802));
#61308=CARTESIAN_POINT('Ctrl Pts',(-1.49500760249196,1.26316552728133,1.54771232549492));
#61309=CARTESIAN_POINT('Ctrl Pts',(-1.07767134532899,1.75709989142681,1.51067510866644));
#61310=CARTESIAN_POINT('Ctrl Pts',(-0.39135122029848,2.02376358702057,1.47363789183796));
#61311=CARTESIAN_POINT('Ctrl Pts',(0.249990333148566,1.94116955279127,1.43660067500948));
#61312=CARTESIAN_POINT('Ctrl Pts',(0.891331886595613,1.85857551856197,1.39956345818101));
#61313=CARTESIAN_POINT('Ctrl Pts',(1.4876948684592,1.42672375450961,1.36252624135253));
#61314=CARTESIAN_POINT('Ctrl Pts',(1.76626827046517,0.843167597229759,1.32548902452405));
#61315=CARTESIAN_POINT('Ctrl Pts',(2.04484167247113,0.259611439949913,1.28845180769557));
#61316=CARTESIAN_POINT('Ctrl Pts',(2.00562549461947,-0.475649110557425,
1.25141459086709));
#61317=CARTESIAN_POINT('Ctrl Pts',(1.66655969053473,-1.02626219289756,1.21437737403861));
#61318=CARTESIAN_POINT('Ctrl Pts',(1.32749388644999,-1.57687527523771,1.17734015721013));
#61319=CARTESIAN_POINT('Ctrl Pts',(0.688578456132156,-1.94284088941065,
1.14030294038165));
#61320=CARTESIAN_POINT('Ctrl Pts',(0.0420898544956178,-1.9567474659654,
1.10326572355317));
#61321=CARTESIAN_POINT('Ctrl Pts',(-0.604398747140919,-1.97065404252014,
1.06622850672469));
#61322=CARTESIAN_POINT('Ctrl Pts',(-1.25846052009616,-1.6325015814567,1.02919128989622));
#61323=CARTESIAN_POINT('Ctrl Pts',(-1.62088905227235,-1.09697626925925,
0.992154073067737));
#61324=CARTESIAN_POINT('Ctrl Pts',(-1.83709816073764,-0.777505145902677,
0.970059279419901));
#61325=CARTESIAN_POINT('Ctrl Pts',(-1.94952091996443,-0.387793032173158,
0.947964485772066));
#61326=CARTESIAN_POINT('Ctrl Pts',(-1.95128203910989,0.000979727872364722,
0.92586969212423));
#61327=CARTESIAN_POINT('Ctrl Pts',(-1.95118672945361,0.000916100096969453,
0.824130307875757));
#61328=CARTESIAN_POINT('Ctrl Pts',(-1.94959408276249,-0.382490737583375,
0.845917324800272));
#61329=CARTESIAN_POINT('Ctrl Pts',(-1.84051065227066,-0.766740948347571,
0.867704341724787));
#61330=CARTESIAN_POINT('Ctrl Pts',(-1.62993550876047,-1.0835175828476,0.889491358649302));
#61331=CARTESIAN_POINT('Ctrl Pts',(-1.27172375978704,-1.62238988461419,
0.926553498593023));
#61332=CARTESIAN_POINT('Ctrl Pts',(-0.619817368257128,-1.96600853193387,
0.963615638536743));
#61333=CARTESIAN_POINT('Ctrl Pts',(0.0271864367452719,-1.95701720127518,
1.00067777848046));
#61334=CARTESIAN_POINT('Ctrl Pts',(0.674190241747668,-1.94802587061648,
1.03773991842418));
#61335=CARTESIAN_POINT('Ctrl Pts',(1.31629146022255,-1.5864245619794,1.07480205836791));
#61336=CARTESIAN_POINT('Ctrl Pts',(1.65939903784035,-1.03781956343241,1.11186419831163));
#61337=CARTESIAN_POINT('Ctrl Pts',(2.00250661545815,-0.489214564885407,
1.14892633825535));
#61338=CARTESIAN_POINT('Ctrl Pts',(2.04662055221888,0.246394123571516,1.18598847819907));
#61339=CARTESIAN_POINT('Ctrl Pts',(1.77153295980734,0.832073910176122,1.22305061814279));
#61340=CARTESIAN_POINT('Ctrl Pts',(1.49644536739581,1.41775369678073,1.26011275808651));
#61341=CARTESIAN_POINT('Ctrl Pts',(0.902156245812001,1.85350458153303,1.29717489803023));
#61342=CARTESIAN_POINT('Ctrl Pts',(0.260864347694114,1.93974733338565,1.33423703797395));
#61343=CARTESIAN_POINT('Ctrl Pts',(-0.380427550423769,2.02599008523827,
1.37129917791767));
#61344=CARTESIAN_POINT('Ctrl Pts',(-1.06872222507573,1.76272470419122,1.40836131786139));
#61345=CARTESIAN_POINT('Ctrl Pts',(-1.48876654315921,1.27053027794487,1.44542345780511));
#61346=CARTESIAN_POINT('Ctrl Pts',(-1.78610829781436,0.922114770268632,
1.47165907449533));
#61347=CARTESIAN_POINT('Ctrl Pts',(-1.94903067523895,0.458983666015645,
1.49789469118554));
#61348=CARTESIAN_POINT('Ctrl Pts',(-1.95287184048439,-0.001702989282844,
1.52413030787576));
#61349=CARTESIAN_POINT('Origin',(0.,0.,0.));
#61350=CARTESIAN_POINT('',(-1.9571996697324,4.08272333451705E-5,2.32586969212423));
#61351=CARTESIAN_POINT('',(-1.95720915199432,4.37834080700025E-5,2.22413030787575));
#61352=CARTESIAN_POINT('',(-1.954,-2.39295984553393E-16,0.));
#61353=CARTESIAN_POINT('Ctrl Pts',(-1.9571996697324,4.08272333451412E-5,
2.32586969212423));
#61354=CARTESIAN_POINT('Ctrl Pts',(-1.9572003426898,0.00222795607483405,
2.32574442104715));
#61355=CARTESIAN_POINT('Ctrl Pts',(-1.95719699336635,0.00441508279392128,
2.32561914997006));
#61356=CARTESIAN_POINT('Ctrl Pts',(-1.95718961556757,0.00660219592375261,
2.32549387889298));
#61357=CARTESIAN_POINT('Ctrl Pts',(-1.9550083208942,0.653236559609951,2.2884566620645));
#61358=CARTESIAN_POINT('Ctrl Pts',(-1.60068669068514,1.29868304829585,2.25141944523602));
#61359=CARTESIAN_POINT('Ctrl Pts',(-1.05631192010051,1.64767712566922,2.21438222840754));
#61360=CARTESIAN_POINT('Ctrl Pts',(-0.511937149515876,1.9966712030426,2.17734501157906));
#61361=CARTESIAN_POINT('Ctrl Pts',(0.222490761444335,2.04921286910345,2.14030779475058));
#61362=CARTESIAN_POINT('Ctrl Pts',(0.811002035332165,1.78126653559889,2.10327057792211));
#61363=CARTESIAN_POINT('Ctrl Pts',(1.39951330921999,1.51332020209433,2.06623336109363));
#61364=CARTESIAN_POINT('Ctrl Pts',(1.84210794603544,0.92488586902436,2.02919614426515));
#61365=CARTESIAN_POINT('Ctrl Pts',(1.93631757329266,0.28514740055385,1.99215892743667));
#61366=CARTESIAN_POINT('Ctrl Pts',(2.03052720054988,-0.354591067916664,
1.95512171060819));
#61367=CARTESIAN_POINT('Ctrl Pts',(1.77635181824887,-1.04563367178771,1.91808449377971));
#61368=CARTESIAN_POINT('Ctrl Pts',(1.29006594271768,-1.47185755477259,1.88104727695123));
#61369=CARTESIAN_POINT('Ctrl Pts',(0.803780067186484,-1.89808143775746,
1.84401006012275));
#61370=CARTESIAN_POINT('Ctrl Pts',(0.0853836984250916,-2.05948659985616,
1.80697284329427));
#61371=CARTESIAN_POINT('Ctrl Pts',(-0.536487147273854,-1.88223703762279,
1.76993562646579));
#61372=CARTESIAN_POINT('Ctrl Pts',(-1.1583579929728,-1.70498747538942,1.73289840963732));
#61373=CARTESIAN_POINT('Ctrl Pts',(-1.68370331560931,-1.18908318882399,
1.69586119280884));
#61374=CARTESIAN_POINT('Ctrl Pts',(-1.87219978227984,-0.570528529192665,
1.65882397598036));
#61375=CARTESIAN_POINT('Ctrl Pts',(-1.92810540551016,-0.387073187246384,
1.64783921469498));
#61376=CARTESIAN_POINT('Ctrl Pts',(-1.95438048401311,-0.194588316428208,
1.63685445340961));
#61377=CARTESIAN_POINT('Ctrl Pts',(-1.95279554503994,-0.00168121501241192,
1.62586969212423));
#61378=CARTESIAN_POINT('Ctrl Pts',(-1.95287184048439,-0.00170298928284375,
1.52413030787576));
#61379=CARTESIAN_POINT('Ctrl Pts',(-1.95445695530526,-0.191812291650776,
1.53495683112926));
#61380=CARTESIAN_POINT('Ctrl Pts',(-1.92895173588402,-0.381505322742495,
1.54578335438277));
#61381=CARTESIAN_POINT('Ctrl Pts',(-1.87462310228398,-0.562548805321496,
1.55660987763628));
#61382=CARTESIAN_POINT('Ctrl Pts',(-1.68864138181028,-1.18230999089587,
1.59367201758));
#61383=CARTESIAN_POINT('Ctrl Pts',(-1.16488397934787,-1.70070889059895,
1.63073415752372));
#61384=CARTESIAN_POINT('Ctrl Pts',(-0.543243355780667,-1.88030816136644,
1.66779629746744));
#61385=CARTESIAN_POINT('Ctrl Pts',(0.0783972677865321,-2.05990743213392,
1.70485843741116));
#61386=CARTESIAN_POINT('Ctrl Pts',(0.797921112458524,-1.90070707396579,
1.74192057735488));
#61387=CARTESIAN_POINT('Ctrl Pts',(1.28577075941843,-1.47562399010748,1.7789827172986));
#61388=CARTESIAN_POINT('Ctrl Pts',(1.77362040637834,-1.05054090624917,1.81604485724232));
#61389=CARTESIAN_POINT('Ctrl Pts',(2.02979585562615,-0.359575096700667,
1.85310699718604));
#61390=CARTESIAN_POINT('Ctrl Pts',(1.93696313672928,0.28079594435252,1.89016913712977));
#61391=CARTESIAN_POINT('Ctrl Pts',(1.84413041783241,0.921166985405712,1.92723127707349));
#61392=CARTESIAN_POINT('Ctrl Pts',(1.40228953079084,1.51094325796358,1.96429341701721));
#61393=CARTESIAN_POINT('Ctrl Pts',(0.813813216582781,1.77999452248681,2.00135555696093));
#61394=CARTESIAN_POINT('Ctrl Pts',(0.225336902374724,2.04904578701004,2.03841769690465));
#61395=CARTESIAN_POINT('Ctrl Pts',(-0.509774838999831,1.99737204349863,
2.07547983684837));
#61396=CARTESIAN_POINT('Ctrl Pts',(-1.05482489992153,1.64864094185095,2.11254197679209));
#61397=CARTESIAN_POINT('Ctrl Pts',(-1.59987496084323,1.29990984020327,2.14960411673581));
#61398=CARTESIAN_POINT('Ctrl Pts',(-1.95486334131209,0.654121380419318,
2.18666625667953));
#61399=CARTESIAN_POINT('Ctrl Pts',(-1.95719765431867,0.0070607094029605,
2.22372839662325));
#61400=CARTESIAN_POINT('Ctrl Pts',(-1.95720609227958,0.00472174601940803,
2.22386236704075));
#61401=CARTESIAN_POINT('Ctrl Pts',(-1.95720992231195,0.00238276601260064,
2.22399633745825));
#61402=CARTESIAN_POINT('Ctrl Pts',(-1.95720915199432,4.37834080701142E-5,
2.22413030787575));
#61403=CARTESIAN_POINT('Origin',(0.,0.,0.));
#61404=CARTESIAN_POINT('',(-1.95267691385146,0.00165493661177622,3.02586969212423));
#61405=CARTESIAN_POINT('',(-1.95274315056508,0.00167675988910205,2.92413030787576));
#61406=CARTESIAN_POINT('',(-1.954,-2.39295984553393E-16,0.));
#61407=CARTESIAN_POINT('Ctrl Pts',(-1.95267691385146,0.00165493661177622,
3.02586969212423));
#61408=CARTESIAN_POINT('Ctrl Pts',(-1.95426560914452,0.198992208020636,
3.01463438868469));
#61409=CARTESIAN_POINT('Ctrl Pts',(-1.92675342506316,0.395896803504792,
3.00339908524515));
#61410=CARTESIAN_POINT('Ctrl Pts',(-1.86830808103941,0.583146374609883,
2.9921637818056));
#61411=CARTESIAN_POINT('Ctrl Pts',(-1.67564280138135,1.20041523640586,2.95512656497712));
#61412=CARTESIAN_POINT('Ctrl Pts',(-1.14682887836242,1.71276357431471,2.91808934814864));
#61413=CARTESIAN_POINT('Ctrl Pts',(-0.523776367443795,1.8858136432031,2.88105213132016));
#61414=CARTESIAN_POINT('Ctrl Pts',(0.0992761434748341,2.0588637120915,2.84401491449168));
#61415=CARTESIAN_POINT('Ctrl Pts',(0.816567242293159,1.89261551195942,2.80697769766321));
#61416=CARTESIAN_POINT('Ctrl Pts',(1.29996651882171,1.46312057934516,2.76994048083473));
#61417=CARTESIAN_POINT('Ctrl Pts',(1.78336579535026,1.03362564673089,2.73290326400625));
#61418=CARTESIAN_POINT('Ctrl Pts',(2.03287324958903,0.340883981634439,2.69586604717777));
#61419=CARTESIAN_POINT('Ctrl Pts',(1.93434974962867,-0.298204336020968,
2.65882883034929));
#61420=CARTESIAN_POINT('Ctrl Pts',(1.83582624966831,-0.937292653676373,
2.62179161352081));
#61421=CARTESIAN_POINT('Ctrl Pts',(1.38927179550881,-1.52272762389073,2.58475439669233));
#61422=CARTESIAN_POINT('Ctrl Pts',(0.798966206784796,-1.78669745083631,
2.54771717986385));
#61423=CARTESIAN_POINT('Ctrl Pts',(0.208660618060775,-2.05066727778188,
2.51067996303538));
#61424=CARTESIAN_POINT('Ctrl Pts',(-0.525396105227766,-1.99317196145866,
2.4736427462069));
#61425=CARTESIAN_POINT('Ctrl Pts',(-1.0674039873032,-1.6405131839538,2.43660552937842));
#61426=CARTESIAN_POINT('Ctrl Pts',(-1.60757863467609,-1.28904720517098,
2.39969358362702));
#61427=CARTESIAN_POINT('Ctrl Pts',(-1.95700137841649,-0.644411052866131,
2.36278163787563));
#61428=CARTESIAN_POINT('Ctrl Pts',(-1.9571996697324,4.08272333451705E-5,
2.32586969212423));
#61429=CARTESIAN_POINT('Ctrl Pts',(-1.95720915199432,4.37834080700025E-5,
2.22413030787575));
#61430=CARTESIAN_POINT('Ctrl Pts',(-1.95699681840184,-0.644683222376,2.26105847740198));
#61431=CARTESIAN_POINT('Ctrl Pts',(-1.60725113883781,-1.28960760246236,
2.2979866469282));
#61432=CARTESIAN_POINT('Ctrl Pts',(-1.06669244200308,-1.64098742623895,
2.33491481645442));
#61433=CARTESIAN_POINT('Ctrl Pts',(-0.524172671136578,-1.99364200861572,
2.37197695639814));
#61434=CARTESIAN_POINT('Ctrl Pts',(0.210547116140745,-2.05061829112049,
2.40903909634186));
#61435=CARTESIAN_POINT('Ctrl Pts',(0.800949322066953,-1.78581989384044,
2.44610123628558));
#61436=CARTESIAN_POINT('Ctrl Pts',(1.39135152799316,-1.52102149656038,2.4831633762293));
#61437=CARTESIAN_POINT('Ctrl Pts',(1.83743615256826,-0.934448419495488,
2.52022551617302));
#61438=CARTESIAN_POINT('Ctrl Pts',(1.93488676008295,-0.294763859316313,
2.55728765611674));
#61439=CARTESIAN_POINT('Ctrl Pts',(2.03233736759764,0.344920700862864,2.59434979606046));
#61440=CARTESIAN_POINT('Ctrl Pts',(1.78115395805193,1.03771674415633,2.63141193600418));
#61441=CARTESIAN_POINT('Ctrl Pts',(1.29638398231036,1.46630865646616,2.6684740759479));
#61442=CARTESIAN_POINT('Ctrl Pts',(0.811614006568792,1.894900568776,2.70553621589162));
#61443=CARTESIAN_POINT('Ctrl Pts',(0.0932574646313782,2.05928835010221,
2.74259835583535));
#61444=CARTESIAN_POINT('Ctrl Pts',(-0.529662765081927,1.88417882975093,
2.77966049577907));
#61445=CARTESIAN_POINT('Ctrl Pts',(-1.15258299479523,1.70906930939964,2.81672263572279));
#61446=CARTESIAN_POINT('Ctrl Pts',(-1.68006691228442,1.19446248737086,2.85378477566651));
#61447=CARTESIAN_POINT('Ctrl Pts',(-1.87051544101399,0.576059451476712,
2.89084691561023));
#61448=CARTESIAN_POINT('Ctrl Pts',(-1.92752575844056,0.390941962730205,
2.90194137969874));
#61449=CARTESIAN_POINT('Ctrl Pts',(-1.95433466869055,0.196523398123763,
2.91303584378725));
#61450=CARTESIAN_POINT('Ctrl Pts',(-1.95274315056508,0.00167675988910205,
2.92413030787576));
#61451=CARTESIAN_POINT('Origin',(0.,0.,0.));
#61452=CARTESIAN_POINT('',(-1.95135107115213,-0.00103745302926256,3.72586969212423));
#61453=CARTESIAN_POINT('',(-1.95125983814034,-0.000967513988672578,3.62413030787576));
#61454=CARTESIAN_POINT('',(-1.954,-2.39295984553393E-16,0.));
#61455=CARTESIAN_POINT('Ctrl Pts',(-1.95135107115213,-0.00103745302926256,
3.72586969212423));
#61456=CARTESIAN_POINT('Ctrl Pts',(-1.9494564270682,0.392108141373472,3.70352435632223));
#61457=CARTESIAN_POINT('Ctrl Pts',(-1.83428685915158,0.78627490539017,3.68117902052023));
#61458=CARTESIAN_POINT('Ctrl Pts',(-1.61345116677478,1.10788542383069,3.65883368471823));
#61459=CARTESIAN_POINT('Ctrl Pts',(-1.24741775852795,1.64095230684139,3.62179646788975));
#61460=CARTESIAN_POINT('Ctrl Pts',(-0.591089924893776,1.97468687095231,
3.58475925106126));
#61461=CARTESIAN_POINT('Ctrl Pts',(0.0552900452708404,1.95641963566092,
3.54772203423278));
#61462=CARTESIAN_POINT('Ctrl Pts',(0.701670015435453,1.93815240036952,3.51068481740431));
#61463=CARTESIAN_POINT('Ctrl Pts',(1.3381021221305,1.56788336567581,3.47364760057583));
#61464=CARTESIAN_POINT('Ctrl Pts',(1.6734455320356,1.01499499073225,3.43661038374735));
#61465=CARTESIAN_POINT('Ctrl Pts',(2.0087889419407,0.462106615788698,3.39957316691887));
#61466=CARTESIAN_POINT('Ctrl Pts',(2.04304365505584,-0.273401099404705,
3.36253595009039));
#61467=CARTESIAN_POINT('Ctrl Pts',(1.76053958557416,-0.855064411333041,
3.32549873326191));
#61468=CARTESIAN_POINT('Ctrl Pts',(1.47803551609248,-1.43672772326139,3.28846151643343));
#61469=CARTESIAN_POINT('Ctrl Pts',(0.878772664013962,-1.86454663192466,
3.25142429960495));
#61470=CARTESIAN_POINT('Ctrl Pts',(0.236888497103484,-1.94281203925035,
3.21438708277648));
#61471=CARTESIAN_POINT('Ctrl Pts',(-0.404995669806982,-2.02107744657604,
3.177349865948));
#61472=CARTESIAN_POINT('Ctrl Pts',(-1.08950115154941,-1.74978935256416,
3.14031264911952));
#61473=CARTESIAN_POINT('Ctrl Pts',(-1.50349557427203,-1.25305061271667,
3.10327543229104));
#61474=CARTESIAN_POINT('Ctrl Pts',(-1.79190407667273,-0.906998424134863,
3.0774735189021));
#61475=CARTESIAN_POINT('Ctrl Pts',(-1.94902846959061,-0.451530792879088,
3.05167160551317));
#61476=CARTESIAN_POINT('Ctrl Pts',(-1.95267691385146,0.00165493661177622,
3.02586969212423));
#61477=CARTESIAN_POINT('Ctrl Pts',(-1.95274315056508,0.00167675988910205,
2.92413030787576));
#61478=CARTESIAN_POINT('Ctrl Pts',(-1.94901804708373,-0.45438081105706,
2.95009798373097));
#61479=CARTESIAN_POINT('Ctrl Pts',(-1.78970412039892,-0.912783539307832,
2.97606565958618));
#61480=CARTESIAN_POINT('Ctrl Pts',(-1.49789482266332,-1.25975537577289,
3.00203333544139));
#61481=CARTESIAN_POINT('Ctrl Pts',(-1.08141253561316,-1.75496791736879,
3.03909547538511));
#61482=CARTESIAN_POINT('Ctrl Pts',(-0.3950348215429,-2.02319375080107,3.07615761532883));
#61483=CARTESIAN_POINT('Ctrl Pts',(0.246862437687336,-1.94157962588032,
3.11321975527255));
#61484=CARTESIAN_POINT('Ctrl Pts',(0.888759696917571,-1.85996550095957,
3.15028189521628));
#61485=CARTESIAN_POINT('Ctrl Pts',(1.48617650130778,-1.4285114176858,3.18734403516));
#61486=CARTESIAN_POINT('Ctrl Pts',(1.76548299529208,-0.84483270534745,3.22440617510372));
#61487=CARTESIAN_POINT('Ctrl Pts',(2.04478948927638,-0.261153993009101,
3.26146831504744));
#61488=CARTESIAN_POINT('Ctrl Pts',(2.00598567285476,0.474749348393822,3.29853045499116));
#61489=CARTESIAN_POINT('Ctrl Pts',(1.66684453569178,1.02581762536563,3.33559259493488));
#61490=CARTESIAN_POINT('Ctrl Pts',(1.3277033985288,1.57688590233743,3.3726547348786));
#61491=CARTESIAN_POINT('Ctrl Pts',(0.688224940624468,1.94311911487812,3.40971687482232));
#61492=CARTESIAN_POINT('Ctrl Pts',(0.0413041672205065,1.95677450731496,
3.44677901476604));
#61493=CARTESIAN_POINT('Ctrl Pts',(-0.605616606183457,1.9704298997518,3.48384115470976));
#61494=CARTESIAN_POINT('Ctrl Pts',(-1.25997969508704,1.63150747208479,3.52090329465349));
#61495=CARTESIAN_POINT('Ctrl Pts',(-1.62207261036362,1.09524104808107,3.55796543459721));
#61496=CARTESIAN_POINT('Ctrl Pts',(-1.83754705311226,0.776119342016343,
3.58002039235672));
#61497=CARTESIAN_POINT('Ctrl Pts',(-1.94952253842872,0.387114015523011,
3.60207535011624));
#61498=CARTESIAN_POINT('Ctrl Pts',(-1.95125983814034,-0.000967513988672578,
3.62413030787576));
#61499=CARTESIAN_POINT('Origin',(0.,0.,0.));
#61500=CARTESIAN_POINT('',(-1.95645574651684,-0.00107576288577632,4.42586969212423));
#61501=CARTESIAN_POINT('',(-1.95628130950281,-0.00119277919923279,4.32413030787576));
#61502=CARTESIAN_POINT('',(-1.954,-2.39295984553393E-16,0.));
#61503=CARTESIAN_POINT('Ctrl Pts',(-1.95645574651684,-0.00107576288577632,
4.42586969212423));
#61504=CARTESIAN_POINT('Ctrl Pts',(-1.95258201164419,0.583617837825317,
4.39241432395977));
#61505=CARTESIAN_POINT('Ctrl Pts',(-1.67312331125722,1.17152394520949,4.35895895579531));
#61506=CARTESIAN_POINT('Ctrl Pts',(-1.21525966387556,1.53420296221226,4.32550358763085));
#61507=CARTESIAN_POINT('Ctrl Pts',(-0.70837553387317,1.93571166257503,4.28846637080237));
#61508=CARTESIAN_POINT('Ctrl Pts',(0.0171598407939347,2.06118438706562,
4.25142915397389));
#61509=CARTESIAN_POINT('Ctrl Pts',(0.629444641593513,1.8532226587955,4.21439193714541));
#61510=CARTESIAN_POINT('Ctrl Pts',(1.24172944239309,1.64526093052537,4.17735472031693));
#61511=CARTESIAN_POINT('Ctrl Pts',(1.74076366932515,1.10386474949453,4.14031750348845));
#61512=CARTESIAN_POINT('Ctrl Pts',(1.89826022128925,0.476700023258525,4.10328028665997));
#61513=CARTESIAN_POINT('Ctrl Pts',(2.05575677325334,-0.150464702977478,
4.06624306983149));
#61514=CARTESIAN_POINT('Ctrl Pts',(1.87171565024948,-0.86339797441863,4.02920585300301));
#61515=CARTESIAN_POINT('Ctrl Pts',(1.43032790007833,-1.33596290298842,3.99216863617453));
#61516=CARTESIAN_POINT('Ctrl Pts',(0.988940149907184,-1.80852783155821,
3.95513141934605));
#61517=CARTESIAN_POINT('Ctrl Pts',(0.290205772568748,-2.04072441725662,
3.91809420251758));
#61518=CARTESIAN_POINT('Ctrl Pts',(-0.346233738762281,-1.92633252011348,
3.8810569856891));
#61519=CARTESIAN_POINT('Ctrl Pts',(-0.982673250093302,-1.81194062297035,
3.84401976886062));
#61520=CARTESIAN_POINT('Ctrl Pts',(-1.55681789541692,-1.35096024298568,
3.80698255203214));
#61521=CARTESIAN_POINT('Ctrl Pts',(-1.806020726649,-0.754270452038098,3.76994533520366));
#61522=CARTESIAN_POINT('Ctrl Pts',(-1.90487422217158,-0.517576224744695,
3.75525345417718));
#61523=CARTESIAN_POINT('Ctrl Pts',(-1.9525967846073,-0.259527562563923,
3.74056157315071));
#61524=CARTESIAN_POINT('Ctrl Pts',(-1.95135107115213,-0.00103745302926256,
3.72586969212423));
#61525=CARTESIAN_POINT('Ctrl Pts',(-1.95125983814034,-0.000967513988672578,
3.62413030787576));
#61526=CARTESIAN_POINT('Ctrl Pts',(-1.95244197476311,-0.265035587897937,
3.63913749005996));
#61527=CARTESIAN_POINT('Ctrl Pts',(-1.90258326051973,-0.528675939020291,
3.65414467224416));
#61528=CARTESIAN_POINT('Ctrl Pts',(-1.799560505048,-0.769580726996389,3.66915185442837));
#61529=CARTESIAN_POINT('Ctrl Pts',(-1.54513274280624,-1.36452565772967,
3.70621399437209));
#61530=CARTESIAN_POINT('Ctrl Pts',(-0.966454476673152,-1.8208050988558,
3.74327613431581));
#61531=CARTESIAN_POINT('Ctrl Pts',(-0.328572905191125,-1.92943316874967,
3.78033827425953));
#61532=CARTESIAN_POINT('Ctrl Pts',(0.309308666290907,-2.03806123864353,
3.81740041420325));
#61533=CARTESIAN_POINT('Ctrl Pts',(1.00639354312189,-1.79903793730513,3.85446255414697));
#61534=CARTESIAN_POINT('Ctrl Pts',(1.44340173058911,-1.32184112162819,3.89152469409069));
#61535=CARTESIAN_POINT('Ctrl Pts',(1.88040991805633,-0.844644305951239,
3.92858683403441));
#61536=CARTESIAN_POINT('Ctrl Pts',(2.05734141615979,-0.129273975935752,
3.96564897397814));
#61537=CARTESIAN_POINT('Ctrl Pts',(1.89315776078089,0.496614739501458,4.00271111392186));
#61538=CARTESIAN_POINT('Ctrl Pts',(1.72897410540198,1.12250345493866,4.03977325386558));
#61539=CARTESIAN_POINT('Ctrl Pts',(1.22367529654071,1.65891055579759,4.0768353938093));
#61540=CARTESIAN_POINT('Ctrl Pts',(0.608699149567017,1.86014995417357,4.11389753375302));
#61541=CARTESIAN_POINT('Ctrl Pts',(-0.00627699740667481,2.06138935254956,
4.15095967369674));
#61542=CARTESIAN_POINT('Ctrl Pts',(-0.730930482492791,1.9274610484426,4.18802181364046));
#61543=CARTESIAN_POINT('Ctrl Pts',(-1.23335429038162,1.51970711029871,4.22508395358418));
#61544=CARTESIAN_POINT('Ctrl Pts',(-1.68092015819396,1.15647443240051,4.25809940501471));
#61545=CARTESIAN_POINT('Ctrl Pts',(-1.95213599025838,0.575947822566119,
4.29111485644523));
#61546=CARTESIAN_POINT('Ctrl Pts',(-1.95628130950281,-0.00119277919923279,
4.32413030787576));
#61547=CARTESIAN_POINT('Origin',(0.,0.,0.));
#61548=CARTESIAN_POINT('',(-1.95458266482996,0.00173443779922018,5.12586969212423));
#61549=CARTESIAN_POINT('',(-1.95491180920002,0.00168629508682236,5.02413030787576));
#61550=CARTESIAN_POINT('',(-1.954,-2.39295984553393E-16,0.));
#61551=CARTESIAN_POINT('Ctrl Pts',(-1.95458266482996,0.00173443779922018,
5.12586969212423));
#61552=CARTESIAN_POINT('Ctrl Pts',(-1.95579683437623,0.13363129532035,5.11834150842579));
#61553=CARTESIAN_POINT('Ctrl Pts',(-1.94358523444966,0.265304620125551,
5.11081332472735));
#61554=CARTESIAN_POINT('Ctrl Pts',(-1.91712292268468,0.394048828472761,
5.10328514102891));
#61555=CARTESIAN_POINT('Ctrl Pts',(-1.78693343503641,1.0274455880328,5.06624792420043));
#61556=CARTESIAN_POINT('Ctrl Pts',(-1.31181246839585,1.58994452273665,5.02921070737195));
#61557=CARTESIAN_POINT('Ctrl Pts',(-0.709107816346671,1.8242261056952,4.99217349054347));
#61558=CARTESIAN_POINT('Ctrl Pts',(-0.106403164297495,2.05850768865374,
4.95513627371499));
#61559=CARTESIAN_POINT('Ctrl Pts',(0.623885173160298,1.96457191986698,4.91809905688651));
#61560=CARTESIAN_POINT('Ctrl Pts',(1.14768109757825,1.58539044975217,4.88106184005803));
#61561=CARTESIAN_POINT('Ctrl Pts',(1.67147702199619,1.20620897963737,4.84402462322955));
#61562=CARTESIAN_POINT('Ctrl Pts',(1.9887805333743,0.541781808194522,4.80698740640107));
#61563=CARTESIAN_POINT('Ctrl Pts',(1.95443866449662,-0.103943670439598,
4.76995018957259));
#61564=CARTESIAN_POINT('Ctrl Pts',(1.92009679561895,-0.749669149073727,
4.73291297274411));
#61565=CARTESIAN_POINT('Ctrl Pts',(1.53410954648549,-1.37669293489913,4.69587575591563));
#61566=CARTESIAN_POINT('Ctrl Pts',(0.973049796091196,-1.69817810439032,
4.65883853908716));
#61567=CARTESIAN_POINT('Ctrl Pts',(0.411990045696909,-2.0196632738815,4.62180132225868));
#61568=CARTESIAN_POINT('Ctrl Pts',(-0.324142205958206,-2.03560982703848,
4.5847641054302));
#61569=CARTESIAN_POINT('Ctrl Pts',(-0.898597516275757,-1.7387228886878,
4.54772688860172));
#61570=CARTESIAN_POINT('Ctrl Pts',(-1.47305282659331,-1.44183595033712,
4.51068967177324));
#61571=CARTESIAN_POINT('Ctrl Pts',(-1.8858311955733,-0.832115520478776,
4.47365245494476));
#61572=CARTESIAN_POINT('Ctrl Pts',(-1.94810393739446,-0.188482967432129,
4.43661523811628));
#61573=CARTESIAN_POINT('Ctrl Pts',(-1.9541262996613,-0.126237620787308,
4.43303338945226));
#61574=CARTESIAN_POINT('Ctrl Pts',(-1.95687048211354,-0.0636751036633503,
4.42945154078825));
#61575=CARTESIAN_POINT('Ctrl Pts',(-1.95645574651684,-0.00107576288577632,
4.42586969212423));
#61576=CARTESIAN_POINT('Ctrl Pts',(-1.95628130950281,-0.00119277919923279,
4.32413030787576));
#61577=CARTESIAN_POINT('Ctrl Pts',(-1.95678939935296,-0.0719326340995119,
4.32817699638895));
#61578=CARTESIAN_POINT('Ctrl Pts',(-1.95328521122814,-0.14262162001596,
4.33222368490215));
#61579=CARTESIAN_POINT('Ctrl Pts',(-1.94560169264522,-0.212853377401693,
4.33627037341534));
#61580=CARTESIAN_POINT('Ctrl Pts',(-1.87523115632842,-0.856080354777335,
4.37333251335906));
#61581=CARTESIAN_POINT('Ctrl Pts',(-1.45429595300328,-1.46095473734778,
4.41039465330279));
#61582=CARTESIAN_POINT('Ctrl Pts',(-0.875593536694013,-1.75043093699665,
4.44745679324651));
#61583=CARTESIAN_POINT('Ctrl Pts',(-0.296891120384743,-2.03990713664554,
4.48451893319023));
#61584=CARTESIAN_POINT('Ctrl Pts',(0.439578508908652,-2.01398515337285,
4.52158107313395));
#61585=CARTESIAN_POINT('Ctrl Pts',(0.9964962855145,-1.68453781781564,4.55864321307767));
#61586=CARTESIAN_POINT('Ctrl Pts',(1.55341406212034,-1.35509048225843,4.59570535302139));
#61587=CARTESIAN_POINT('Ctrl Pts',(1.93077998603865,-0.72211779441669,4.63276749296511));
#61588=CARTESIAN_POINT('Ctrl Pts',(1.95575227831571,-0.0755349757277263,
4.66982963290883));
#61589=CARTESIAN_POINT('Ctrl Pts',(1.98072457059277,0.571047842961237,4.70689177285256));
#61590=CARTESIAN_POINT('Ctrl Pts',(1.6533032312286,1.23124079249743,4.74395391279628));
#61591=CARTESIAN_POINT('Ctrl Pts',(1.12345433605614,1.60266118112717,4.78101605273999));
#61592=CARTESIAN_POINT('Ctrl Pts',(0.59360544088369,1.97408156975691,4.81807819268371));
#61593=CARTESIAN_POINT('Ctrl Pts',(-0.138671010097046,2.05672939748021,
4.85514033262744));
#61594=CARTESIAN_POINT('Ctrl Pts',(-0.737976517839776,1.81275016640803,
4.89220247257116));
#61595=CARTESIAN_POINT('Ctrl Pts',(-1.33728202558251,1.56877093533586,4.92926461251488));
#61596=CARTESIAN_POINT('Ctrl Pts',(-1.80361659008724,0.998164645468222,
4.9663267524586));
#61597=CARTESIAN_POINT('Ctrl Pts',(-1.92338886510923,0.362281355122108,
5.00338889240232));
#61598=CARTESIAN_POINT('Ctrl Pts',(-1.94573194011967,0.243659678682544,
5.01030269756014));
#61599=CARTESIAN_POINT('Ctrl Pts',(-1.95601481281436,0.122766393772507,
5.01721650271795));
#61600=CARTESIAN_POINT('Ctrl Pts',(-1.95491180920002,0.00168629508682236,
5.02413030787576));
#61601=CARTESIAN_POINT('Origin',(0.,0.,0.));
#61602=CARTESIAN_POINT('',(-1.9507978584999,-3.45334863967226E-5,5.82586969212423));
#61603=CARTESIAN_POINT('',(-1.95080468396925,0.00018981806121043,5.72413030787576));
#61604=CARTESIAN_POINT('',(-1.954,-2.39295984553393E-16,0.));
#61605=CARTESIAN_POINT('Ctrl Pts',(-1.95079815420139,-3.45302974047446E-5,
5.82586969212423));
#61606=CARTESIAN_POINT('Ctrl Pts',(-1.95074640707532,0.328120037045956,
5.80723147606333));
#61607=CARTESIAN_POINT('Ctrl Pts',(-1.87237758907749,0.656297824114404,
5.78859326000243));
#61608=CARTESIAN_POINT('Ctrl Pts',(-1.715829951129,0.941574404236039,5.76995504394152));
#61609=CARTESIAN_POINT('Ctrl Pts',(-1.4047439120071,1.50846613462089,5.73291782711304));
#61610=CARTESIAN_POINT('Ctrl Pts',(-0.784943311216198,1.90594846094957,
5.69588061028457));
#61611=CARTESIAN_POINT('Ctrl Pts',(-0.139960769924853,1.95218999146749,
5.65884339345609));
#61612=CARTESIAN_POINT('Ctrl Pts',(0.505021771366483,1.99843152198542,5.62180617662761));
#61613=CARTESIAN_POINT('Ctrl Pts',(1.17518625315826,1.69343225669258,5.58476895979913));
#61614=CARTESIAN_POINT('Ctrl Pts',(1.56396070392606,1.17671648942254,5.54773174297065));
#61615=CARTESIAN_POINT('Ctrl Pts',(1.95273515469386,0.660000722152496,5.51069452614217));
#61616=CARTESIAN_POINT('Ctrl Pts',(2.06011957443768,-0.0684315470947738,
5.47365730931369));
#61617=CARTESIAN_POINT('Ctrl Pts',(1.83699012241942,-0.675353292756691,
5.43662009248521));
#61618=CARTESIAN_POINT('Ctrl Pts',(1.61386067040115,-1.28227503841861,5.39958287565673));
#61619=CARTESIAN_POINT('Ctrl Pts',(1.06021734662079,-1.76768626049519,5.36254565882826));
#61620=CARTESIAN_POINT('Ctrl Pts',(0.429328609649713,-1.90953180775813,
5.32550844199978));
#61621=CARTESIAN_POINT('Ctrl Pts',(-0.201560127321352,-2.05137735502108,
5.2884712251713));
#61622=CARTESIAN_POINT('Ctrl Pts',(-0.909694277483132,-1.84965722747041,
5.25143400834282));
#61623=CARTESIAN_POINT('Ctrl Pts',(-1.37113234823603,-1.39664987148696,
5.21439679151434));
#61624=CARTESIAN_POINT('Ctrl Pts',(-1.73877852911313,-1.03572077852157,
5.1848877583843));
#61625=CARTESIAN_POINT('Ctrl Pts',(-1.94982335358017,-0.515275892214865,
5.15537872525427));
#61626=CARTESIAN_POINT('Ctrl Pts',(-1.95458266482996,0.00173443779922018,
5.12586969212423));
#61627=CARTESIAN_POINT('Ctrl Pts',(-1.95491180920002,0.00168629508682236,
5.02413030787576));
#61628=CARTESIAN_POINT('Ctrl Pts',(-1.95010205227512,-0.526295513449078,
5.05427864266167));
#61629=CARTESIAN_POINT('Ctrl Pts',(-1.72879182329996,-1.05782955367232,
5.08442697744757));
#61630=CARTESIAN_POINT('Ctrl Pts',(-1.34689356786549,-1.42005289462677,
5.11457531223348));
#61631=CARTESIAN_POINT('Ctrl Pts',(-0.877416010060499,-1.86534356320495,
5.1516374521772));
#61632=CARTESIAN_POINT('Ctrl Pts',(-0.165250908911267,-2.05476460953673,
5.18869959212092));
#61633=CARTESIAN_POINT('Ctrl Pts',(0.463414671012952,-1.90155708549211,
5.22576173206464));
#61634=CARTESIAN_POINT('Ctrl Pts',(1.09208025093718,-1.74834956144749,5.26282387200837));
#61635=CARTESIAN_POINT('Ctrl Pts',(1.63724630963639,-1.25251346702646,5.29988601195209));
#61636=CARTESIAN_POINT('Ctrl Pts',(1.84921496651671,-0.641152489120857,
5.33694815189581));
#61637=CARTESIAN_POINT('Ctrl Pts',(2.06118362339704,-0.0297915112152539,
5.37401029183953));
#61638=CARTESIAN_POINT('Ctrl Pts',(1.93995487845847,0.697094350174917,5.41107243178325));
#61639=CARTESIAN_POINT('Ctrl Pts',(1.54105412656959,1.20657560296821,5.44813457172697));
#61640=CARTESIAN_POINT('Ctrl Pts',(1.14215337468071,1.71605685576151,5.48519671167069));
#61641=CARTESIAN_POINT('Ctrl Pts',(0.465580615841514,2.00813349995792,5.52225885161441));
#61642=CARTESIAN_POINT('Ctrl Pts',(-0.178779150223708,1.94902809680635,
5.55932099155813));
#61643=CARTESIAN_POINT('Ctrl Pts',(-0.823138916288934,1.88992269365477,
5.59638313150186));
#61644=CARTESIAN_POINT('Ctrl Pts',(-1.43528568958019,1.4796352431552,5.63344527144558));
#61645=CARTESIAN_POINT('Ctrl Pts',(-1.73484296927877,0.906086297567352,
5.6705074113893));
#61646=CARTESIAN_POINT('Ctrl Pts',(-1.87931321146693,0.629475576708828,
5.68838171021812));
#61647=CARTESIAN_POINT('Ctrl Pts',(-1.95107725773013,0.31489133949035,5.70625600904694));
#61648=CARTESIAN_POINT('Ctrl Pts',(-1.95080468396925,0.00018981806121043,
5.72413030787576));
#61649=CARTESIAN_POINT('Origin',(0.,0.,0.));
#61650=CARTESIAN_POINT('',(-1.95470932084261,-0.00171584046685047,6.52586969212424));
#61651=CARTESIAN_POINT('',(-1.95421427783755,-0.00177812761388513,6.42413030787576));
#61652=CARTESIAN_POINT('',(-1.954,-2.39295984553393E-16,0.));
#61653=CARTESIAN_POINT('Ctrl Pts',(-1.95470932084261,-0.00171584046685047,
6.52586969212424));
#61654=CARTESIAN_POINT('Ctrl Pts',(-1.94992946923152,0.519398730151351,
6.49612144370087));
#61655=CARTESIAN_POINT('Ctrl Pts',(-1.73506994162404,1.04399306729571,6.46637319527751));
#61656=CARTESIAN_POINT('Ctrl Pts',(-1.36210733975536,1.40545308526766,6.43662494685414));
#61657=CARTESIAN_POINT('Ctrl Pts',(-0.897760782010601,1.85547867567989,
6.39958773002566));
#61658=CARTESIAN_POINT('Ctrl Pts',(-0.188341937200331,2.05263315093338,
6.36255051319719));
#61659=CARTESIAN_POINT('Ctrl Pts',(0.441620008484366,1.90672665791667,6.32551329636871));
#61660=CARTESIAN_POINT('Ctrl Pts',(1.07158195416906,1.76082016489995,6.28847607954023));
#61661=CARTESIAN_POINT('Ctrl Pts',(1.62208700072817,1.27185270361303,6.25143886271175));
#61662=CARTESIAN_POINT('Ctrl Pts',(1.84130231899333,0.663506254660481,6.21440164588327));
#61663=CARTESIAN_POINT('Ctrl Pts',(2.0605176372585,0.0551598057079281,6.17736442905479));
#61664=CARTESIAN_POINT('Ctrl Pts',(1.94844322722972,-0.672565630910262,
6.14032721222632));
#61665=CARTESIAN_POINT('Ctrl Pts',(1.55634840229719,-1.18676637573315,6.10328999539784));
#61666=CARTESIAN_POINT('Ctrl Pts',(1.16425357736466,-1.70096712055603,6.06625277856936));
#61667=CARTESIAN_POINT('Ctrl Pts',(0.492138337528384,-2.00164317358361,
6.02921556174087));
#61668=CARTESIAN_POINT('Ctrl Pts',(-0.152532956197894,-1.95124792816734,
5.9921783449124));
#61669=CARTESIAN_POINT('Ctrl Pts',(-0.797204249924167,-1.90085268275106,
5.95514112808392));
#61670=CARTESIAN_POINT('Ctrl Pts',(-1.41443159754043,-1.49938613889095,
5.91810391125544));
#61671=CARTESIAN_POINT('Ctrl Pts',(-1.72185953262212,-0.930502299740384,
5.88106669442696));
#61672=CARTESIAN_POINT('Ctrl Pts',(-1.87458069522289,-0.647897528391999,
5.86266769365939));
#61673=CARTESIAN_POINT('Ctrl Pts',(-1.95084923717034,-0.323977343102287,
5.84426869289181));
#61674=CARTESIAN_POINT('Ctrl Pts',(-1.95079815420139,-3.45302974047446E-5,
5.82586969212423));
#61675=CARTESIAN_POINT('Ctrl Pts',(-1.95080468396925,0.00018981806121043,
5.72413030787576));
#61676=CARTESIAN_POINT('Ctrl Pts',(-1.95051207937167,-0.337638415069996,
5.74331814899066));
#61677=CARTESIAN_POINT('Ctrl Pts',(-1.86720620393942,-0.675601803708791,
5.76250599010555));
#61678=CARTESIAN_POINT('Ctrl Pts',(-1.70171536425399,-0.966869859783203,
5.78169383122045));
#61679=CARTESIAN_POINT('Ctrl Pts',(-1.38206269342473,-1.5294666308698,5.81875597116418));
#61680=CARTESIAN_POINT('Ctrl Pts',(-0.755789565660301,-1.91784973236686,
5.85581811110791));
#61681=CARTESIAN_POINT('Ctrl Pts',(-0.109742658556152,-1.95413127900566,
5.89288025105163));
#61682=CARTESIAN_POINT('Ctrl Pts',(0.536304248547996,-1.99041282564447,
5.92994239099535));
#61683=CARTESIAN_POINT('Ctrl Pts',(1.20212493499187,-1.674592817425,5.96700453093906));
#61684=CARTESIAN_POINT('Ctrl Pts',(1.58275908344154,-1.15132366886058,6.00406667088278));
#61685=CARTESIAN_POINT('Ctrl Pts',(1.9633932318912,-0.628054520296152,6.0411288108265));
#61686=CARTESIAN_POINT('Ctrl Pts',(2.05884084234667,0.102663768613233,6.07819095077022));
#61687=CARTESIAN_POINT('Ctrl Pts',(1.82538483877546,0.706146370849535,6.11525309071394));
#61688=CARTESIAN_POINT('Ctrl Pts',(1.59192883520425,1.30962897308584,6.15231523065767));
#61689=CARTESIAN_POINT('Ctrl Pts',(1.02956921760636,1.78587588864905,6.18937737060139));
#61690=CARTESIAN_POINT('Ctrl Pts',(0.395878889512919,1.91675569949154,6.22643951054511));
#61691=CARTESIAN_POINT('Ctrl Pts',(-0.237811438580523,2.04763551033402,
6.26350165048883));
#61692=CARTESIAN_POINT('Ctrl Pts',(-0.942832477169518,1.83314821645578,
6.30056379043255));
#61693=CARTESIAN_POINT('Ctrl Pts',(-1.39626929730598,1.37153365109863,6.33762593037627));
#61694=CARTESIAN_POINT('Ctrl Pts',(-1.7490486198241,1.01239194403086,6.3664607228761));
#61695=CARTESIAN_POINT('Ctrl Pts',(-1.94954331224527,0.503663409317413,
6.39529551537593));
#61696=CARTESIAN_POINT('Ctrl Pts',(-1.95421427783755,-0.00177812761388513,
6.42413030787576));
#61697=CARTESIAN_POINT('Origin',(0.,0.,0.));
#61698=CARTESIAN_POINT('',(-1.95636369417486,0.00113518110994186,7.22586969212423));
#61699=CARTESIAN_POINT('',(-1.95675615924934,0.000851174274233985,7.12413030787576));
#61700=CARTESIAN_POINT('',(-1.954,-2.39295984553393E-16,0.));
#61701=CARTESIAN_POINT('Ctrl Pts',(-1.95636369417486,0.00113518110994186,
7.22586969212423));
#61702=CARTESIAN_POINT('Ctrl Pts',(-1.95682546989371,0.0679235189129894,
7.22204862816689));
#61703=CARTESIAN_POINT('Ctrl Pts',(-1.95370156992351,0.134668159558925,
7.21822756420955));
#61704=CARTESIAN_POINT('Ctrl Pts',(-1.94684940168549,0.201027826582277,
7.2144065002522));
#61705=CARTESIAN_POINT('Ctrl Pts',(-1.88043197355288,0.844245894546327,
7.17736928342373));
#61706=CARTESIAN_POINT('Ctrl Pts',(-1.46373463610807,1.45129475044757,7.14033206659525));
#61707=CARTESIAN_POINT('Ctrl Pts',(-0.887378837876281,1.74447515831938,
7.10329484976677));
#61708=CARTESIAN_POINT('Ctrl Pts',(-0.31102303964449,2.03765556619118,7.06625763293829));
#61709=CARTESIAN_POINT('Ctrl Pts',(0.424991219374283,2.01696752603353,7.02922041610981));
#61710=CARTESIAN_POINT('Ctrl Pts',(0.983968473233738,1.69187494324663,6.99218319928133));
#61711=CARTESIAN_POINT('Ctrl Pts',(1.54294572709319,1.36678236045973,6.95514598245285));
#61712=CARTESIAN_POINT('Ctrl Pts',(1.92488597579333,0.737285235043576,6.91810876562437));
#61713=CARTESIAN_POINT('Ctrl Pts',(1.95506767226643,0.0913519390189264,
6.8810715487959));
#61714=CARTESIAN_POINT('Ctrl Pts',(1.98524936873952,-0.554581357005719,
6.84403433196742));
#61715=CARTESIAN_POINT('Ctrl Pts',(1.66367251298559,-1.21695082363886,6.80699711513894));
#61716=CARTESIAN_POINT('Ctrl Pts',(1.13744494695038,-1.59275037986524,6.76995989831046));
#61717=CARTESIAN_POINT('Ctrl Pts',(0.611217380915185,-1.96854993609162,
6.73292268148198));
#61718=CARTESIAN_POINT('Ctrl Pts',(-0.119660895401274,-2.05777958191125,
6.69588546465349));
#61719=CARTESIAN_POINT('Ctrl Pts',(-0.72084391141631,-1.81962051958034,
6.65884824782502));
#61720=CARTESIAN_POINT('Ctrl Pts',(-1.32202692743135,-1.58146145724943,
6.62181103099654));
#61721=CARTESIAN_POINT('Ctrl Pts',(-1.79351468314497,-1.01591368676797,
6.58477381416807));
#61722=CARTESIAN_POINT('Ctrl Pts',(-1.91962142566216,-0.381691448741754,
6.54773659733959));
#61723=CARTESIAN_POINT('Ctrl Pts',(-1.9444393828574,-0.256875756563692,
6.54044762893447));
#61724=CARTESIAN_POINT('Ctrl Pts',(-1.95588048853217,-0.129400253566584,
6.53315866052935));
#61725=CARTESIAN_POINT('Ctrl Pts',(-1.95470932084261,-0.00171584046685047,
6.52586969212424));
#61726=CARTESIAN_POINT('Ctrl Pts',(-1.95421427783755,-0.00177812761388513,
6.42413030787576));
#61727=CARTESIAN_POINT('Ctrl Pts',(-1.95554703085897,-0.145994290672205,
6.43235765531965));
#61728=CARTESIAN_POINT('Ctrl Pts',(-1.94093747105224,-0.289942854151266,
6.44058500276354));
#61729=CARTESIAN_POINT('Ctrl Pts',(-1.90937423221194,-0.430072724152966,
6.44881235020743));
#61730=CARTESIAN_POINT('Ctrl Pts',(-1.7671897452975,-1.06132269721135,6.48587449015115));
#61731=CARTESIAN_POINT('Ctrl Pts',(-1.28096816978468,-1.61508080649208,
6.52293663009487));
#61732=CARTESIAN_POINT('Ctrl Pts',(-0.67340953434779,-1.83771382585667,
6.55999877003859));
#61733=CARTESIAN_POINT('Ctrl Pts',(-0.0658508989108841,-2.06034684522128,
6.59706090998232));
#61734=CARTESIAN_POINT('Ctrl Pts',(0.663044796450101,-1.95185477466974,
6.63412304992604));
#61735=CARTESIAN_POINT('Ctrl Pts',(1.17942751209788,-1.56192933591821,6.67118518986976));
#61736=CARTESIAN_POINT('Ctrl Pts',(1.69581022774564,-1.17200389716668,6.70824732981348));
#61737=CARTESIAN_POINT('Ctrl Pts',(1.9996799636802,-0.500645090215166,6.7453094697572));
#61738=CARTESIAN_POINT('Ctrl Pts',(1.95185778931935,0.144650188277344,6.78237160970092));
#61739=CARTESIAN_POINT('Ctrl Pts',(1.90403561495849,0.789945466769872,6.81943374964464));
#61740=CARTESIAN_POINT('Ctrl Pts',(1.5045215303022,1.4091772168034,6.85649588958836));
#61741=CARTESIAN_POINT('Ctrl Pts',(0.936301652358751,1.71872386452436,6.89355802953208));
#61742=CARTESIAN_POINT('Ctrl Pts',(0.368081774415317,2.02827051224532,6.9306201694758));
#61743=CARTESIAN_POINT('Ctrl Pts',(-0.368843896815252,2.02813205765373,
6.96768230941953));
#61744=CARTESIAN_POINT('Ctrl Pts',(-0.936947418561655,1.71837191595589,
7.00474444936325));
#61745=CARTESIAN_POINT('Ctrl Pts',(-1.50505094030807,1.40861177425805,7.04180658930697));
#61746=CARTESIAN_POINT('Ctrl Pts',(-1.90433231257031,0.78922994545395,7.07886872925069));
#61747=CARTESIAN_POINT('Ctrl Pts',(-1.95191200566454,0.143916742729559,
7.11593086919441));
#61748=CARTESIAN_POINT('Ctrl Pts',(-1.95542076848464,0.0963281429343837,
7.11866401542153));
#61749=CARTESIAN_POINT('Ctrl Pts',(-1.95701686505733,0.0485985200318871,
7.12139716164864));
#61750=CARTESIAN_POINT('Ctrl Pts',(-1.95675615924934,0.000851174274233985,
7.12413030787576));
#61751=CARTESIAN_POINT('Origin',(0.,0.,0.));
#61752=CARTESIAN_POINT('',(-1.95128545551857,0.000980157954364874,7.92586969212424));
#61753=CARTESIAN_POINT('',(-1.95166123101285,0.00126544742759004,7.82413030787576));
#61754=CARTESIAN_POINT('',(-1.954,-2.39295984553393E-16,0.));
#61755=CARTESIAN_POINT('Ctrl Pts',(-1.95128545551857,0.000980157954364874,
7.92586969212424));
#61756=CARTESIAN_POINT('Ctrl Pts',(-1.95247914943593,0.263701155015296,
7.91093859580443));
#61757=CARTESIAN_POINT('Ctrl Pts',(-1.90313505751618,0.525992349613935,
7.89600749948463));
#61758=CARTESIAN_POINT('Ctrl Pts',(-1.80112460177197,0.765888339627252,
7.88107640316483));
#61759=CARTESIAN_POINT('Ctrl Pts',(-1.54808334564134,1.36096050365993,7.84403918633635));
#61760=CARTESIAN_POINT('Ctrl Pts',(-0.970981193167941,1.81823294990903,
7.80700196950786));
#61761=CARTESIAN_POINT('Ctrl Pts',(-0.333818027149729,1.92852282969788,
7.76996475267938));
#61762=CARTESIAN_POINT('Ctrl Pts',(0.303345138868501,2.03881270948674,7.73292753585091));
#61763=CARTESIAN_POINT('Ctrl Pts',(1.00056931843154,1.80212002281537,7.69589031902244));
#61764=CARTESIAN_POINT('Ctrl Pts',(1.43890387011628,1.32672168613705,7.65885310219396));
#61765=CARTESIAN_POINT('Ctrl Pts',(1.87723842180101,0.851323349458752,7.62181588536548));
#61766=CARTESIAN_POINT('Ctrl Pts',(2.05668334560742,0.13721936277351,7.58477866853699));
#61767=CARTESIAN_POINT('Ctrl Pts',(1.8951501609247,-0.488917833023672,7.54774145170851));
#61768=CARTESIAN_POINT('Ctrl Pts',(1.73361697624198,-1.11505502882086,7.51070423488003));
#61769=CARTESIAN_POINT('Ctrl Pts',(1.23110568307013,-1.65322543373001,7.47366701805156));
#61770=CARTESIAN_POINT('Ctrl Pts',(0.61749399359133,-1.85723879665063,7.43662980122308));
#61771=CARTESIAN_POINT('Ctrl Pts',(0.00388230411252383,-2.06125215957126,
7.3995925843946));
#61772=CARTESIAN_POINT('Ctrl Pts',(-0.72082978167322,-1.93110848050335,
7.36255536756612));
#61773=CARTESIAN_POINT('Ctrl Pts',(-1.22511706515588,-1.52634300095596,
7.32551815073764));
#61774=CARTESIAN_POINT('Ctrl Pts',(-1.6773779241913,-1.16333645789233,7.2923019978665));
#61775=CARTESIAN_POINT('Ctrl Pts',(-1.95234952088687,-0.579449614967985,
7.25908584499537));
#61776=CARTESIAN_POINT('Ctrl Pts',(-1.95636369417486,0.00113518110994186,
7.22586969212423));
#61777=CARTESIAN_POINT('Ctrl Pts',(-1.95675615924934,0.000851174274233985,
7.12413030787576));
#61778=CARTESIAN_POINT('Ctrl Pts',(-1.95348162971424,-0.598867317271105,
7.15845930159236));
#61779=CARTESIAN_POINT('Ctrl Pts',(-1.65727828481393,-1.20138176331325,
7.19278829530897));
#61780=CARTESIAN_POINT('Ctrl Pts',(-1.17884051406102,-1.56237241050387,
7.22711728902557));
#61781=CARTESIAN_POINT('Ctrl Pts',(-0.662311315437018,-1.95210378436822,
7.2641794289693));
#61782=CARTESIAN_POINT('Ctrl Pts',(0.0666250957372189,-2.06032195545224,
7.30124156891302));
#61783=CARTESIAN_POINT('Ctrl Pts',(0.674100031098693,-1.83746065393738,
7.33830370885674));
#61784=CARTESIAN_POINT('Ctrl Pts',(1.28157496646017,-1.61459935242253,7.37536584880046));
#61785=CARTESIAN_POINT('Ctrl Pts',(1.76758842600887,-1.0606585783088,7.41242798874417));
#61786=CARTESIAN_POINT('Ctrl Pts',(1.9095357026966,-0.429355222190436,7.44949012868789));
#61787=CARTESIAN_POINT('Ctrl Pts',(2.05148297938434,0.201948133927931,7.48655226863161));
#61788=CARTESIAN_POINT('Ctrl Pts',(1.84936407321109,0.910614072050953,7.52361440857534));
#61789=CARTESIAN_POINT('Ctrl Pts',(1.39575382755531,1.37205822017881,7.56067654851907));
#61790=CARTESIAN_POINT('Ctrl Pts',(0.942143581899539,1.83350236830666,7.59773868846279));
#61791=CARTESIAN_POINT('Ctrl Pts',(0.237041996761252,2.04772472643938,7.6348008284065));
#61792=CARTESIAN_POINT('Ctrl Pts',(-0.396599106844383,1.91660680765389,
7.67186296835022));
#61793=CARTESIAN_POINT('Ctrl Pts',(-1.03024021045003,1.78548888886839,7.70892510829394));
#61794=CARTESIAN_POINT('Ctrl Pts',(-1.59242083252301,1.30903069316467,7.74598724823766));
#61795=CARTESIAN_POINT('Ctrl Pts',(-1.82565005336597,0.705460409477194,
7.78304938818139));
#61796=CARTESIAN_POINT('Ctrl Pts',(-1.9118230851659,0.482454556858425,7.79674302807951));
#61797=CARTESIAN_POINT('Ctrl Pts',(-1.95308968355645,0.242096139413284,
7.81043666797764));
#61798=CARTESIAN_POINT('Ctrl Pts',(-1.95166123101285,0.00126544742759004,
7.82413030787576));
#61799=CARTESIAN_POINT('Origin',(0.,0.,0.));
#61800=CARTESIAN_POINT('',(-1.95279013340439,-0.00168009551267251,8.62586969212423));
#61801=CARTESIAN_POINT('',(-1.95215444869335,-0.00150235120299324,8.52413030787576));
#61802=CARTESIAN_POINT('',(-1.954,-2.39295984553393E-16,0.));
#61803=CARTESIAN_POINT('Ctrl Pts',(-1.95279013340439,-0.00168009551267251,
8.62586969212423));
#61804=CARTESIAN_POINT('Ctrl Pts',(-1.94903607268958,0.455640131522026,
8.59982856344197));
#61805=CARTESIAN_POINT('Ctrl Pts',(-1.78871895344458,0.915331173731693,
8.57378743475971));
#61806=CARTESIAN_POINT('Ctrl Pts',(-1.49539281844263,1.26270942713959,8.54774630607745));
#61807=CARTESIAN_POINT('Ctrl Pts',(-1.07820722729247,1.75677110357261,8.51070908924897));
#61808=CARTESIAN_POINT('Ctrl Pts',(-0.391968436807465,2.02364430724413,
8.47367187242049));
#61809=CARTESIAN_POINT('Ctrl Pts',(0.24939826400162,1.94124580780539,8.43663465559201));
#61810=CARTESIAN_POINT('Ctrl Pts',(0.890764964810705,1.85884730836666,8.39959743876353));
#61811=CARTESIAN_POINT('Ctrl Pts',(1.48725957594388,1.42717710581768,8.36256022193505));
#61812=CARTESIAN_POINT('Ctrl Pts',(1.76601098282085,0.843706103134459,8.32552300510657));
#61813=CARTESIAN_POINT('Ctrl Pts',(2.04476238969783,0.260235100451228,8.28848578827809));
#61814=CARTESIAN_POINT('Ctrl Pts',(2.00577059231861,-0.475036702366233,
8.25144857144961));
#61815=CARTESIAN_POINT('Ctrl Pts',(1.66687269277466,-1.02575348200379,8.21441135462113));
#61816=CARTESIAN_POINT('Ctrl Pts',(1.32797479323072,-1.57647026164133,8.17737413779266));
#61817=CARTESIAN_POINT('Ctrl Pts',(0.689170791522051,-1.94263201809897,
8.14033692096418));
#61818=CARTESIAN_POINT('Ctrl Pts',(0.0426865627857745,-1.95673519857469,
8.1032997041357));
#61819=CARTESIAN_POINT('Ctrl Pts',(-0.60379766595052,-1.97083837905041,
8.06626248730722));
#61820=CARTESIAN_POINT('Ctrl Pts',(-1.25796212171444,-1.6328829835442,8.02922527047874));
#61821=CARTESIAN_POINT('Ctrl Pts',(-1.62055416970245,-1.09746934488294,
7.99218805365026));
#61822=CARTESIAN_POINT('Ctrl Pts',(-1.83697171385623,-0.777901098892797,
7.97008193314158));
#61823=CARTESIAN_POINT('Ctrl Pts',(-1.94951814111497,-0.387989405753114,
7.94797581263291));
#61824=CARTESIAN_POINT('Ctrl Pts',(-1.95128545551857,0.000980157954364874,
7.92586969212424));
#61825=CARTESIAN_POINT('Ctrl Pts',(-1.95166123101285,0.00126544742759004,
7.82413030787576));
#61826=CARTESIAN_POINT('Ctrl Pts',(-1.94922354508138,-0.409717467160323,
7.84749880792136));
#61827=CARTESIAN_POINT('Ctrl Pts',(-1.82244856716882,-0.822075748123473,
7.87086730796695));
#61828=CARTESIAN_POINT('Ctrl Pts',(-1.58232634722073,-1.15191832939155,
7.89423580801255));
#61829=CARTESIAN_POINT('Ctrl Pts',(-1.20149560061961,-1.67504441290151,
7.93129794795627));
#61830=CARTESIAN_POINT('Ctrl Pts',(-0.535556287804454,-1.99061420825021,
7.96836008789999));
#61831=CARTESIAN_POINT('Ctrl Pts',(0.110476940437387,-1.95408990384897,
8.00542222784371));
#61832=CARTESIAN_POINT('Ctrl Pts',(0.756510168679237,-1.91756559944773,
8.04248436778743));
#61833=CARTESIAN_POINT('Ctrl Pts',(1.38263731234777,-1.52894719529654,8.07954650773116));
#61834=CARTESIAN_POINT('Ctrl Pts',(1.70207855773424,-0.966230350379699,
8.11660864767487));
#61835=CARTESIAN_POINT('Ctrl Pts',(2.02151980312072,-0.403513505462853,
8.1536707876186));
#61836=CARTESIAN_POINT('Ctrl Pts',(2.03427515022513,0.333301780219651,8.19073292756232));
#61837=CARTESIAN_POINT('Ctrl Pts',(1.73450237337761,0.906738122863988,8.22779506750604));
#61838=CARTESIAN_POINT('Ctrl Pts',(1.43472959653009,1.48017446550833,8.26485720744976));
#61839=CARTESIAN_POINT('Ctrl Pts',(0.822428695730641,1.89023186511451,8.30191934739348));
#61840=CARTESIAN_POINT('Ctrl Pts',(0.178046765554912,1.94909513773745,8.3389814873372));
#61841=CARTESIAN_POINT('Ctrl Pts',(-0.466335164620799,2.00795841036038,
8.37604362728092));
#61842=CARTESIAN_POINT('Ctrl Pts',(-1.14279812417278,1.71562755600011,8.41310576722464));
#61843=CARTESIAN_POINT('Ctrl Pts',(-1.54150740386038,1.20599644714809,8.45016790716836));
#61844=CARTESIAN_POINT('Ctrl Pts',(-1.80673309918174,0.866984359672774,
8.47482204073749));
#61845=CARTESIAN_POINT('Ctrl Pts',(-1.94905131081074,0.431815751432988,
8.49947617430663));
#61846=CARTESIAN_POINT('Ctrl Pts',(-1.95215444869335,-0.00150235120299324,
8.52413030787576));
#61847=CARTESIAN_POINT('Origin',(0.,0.,0.));
#61848=CARTESIAN_POINT('',(-1.95719986784682,3.71606954582295E-5,9.32586969212424));
#61849=CARTESIAN_POINT('',(-1.95707453392556,-0.000466568259871601,9.22413030787576));
#61850=CARTESIAN_POINT('',(-1.954,-2.39295984553393E-16,0.));
#61851=CARTESIAN_POINT('Ctrl Pts',(-1.95719986784682,3.71606954581456E-5,
9.32586969212423));
#61852=CARTESIAN_POINT('Ctrl Pts',(-1.95720042510874,0.00202653151786848,
9.32575574790799));
#61853=CARTESIAN_POINT('Ctrl Pts',(-1.95719765412071,0.00401590074103218,
9.32564180369175));
#61854=CARTESIAN_POINT('Ctrl Pts',(-1.95719155021855,0.00600525973720184,
9.32552785947551));
#61855=CARTESIAN_POINT('Ctrl Pts',(-1.95520749560565,0.65264027922361,9.28849064264703));
#61856=CARTESIAN_POINT('Ctrl Pts',(-1.60108272580438,1.29819476052309,9.25145342581855));
#61857=CARTESIAN_POINT('Ctrl Pts',(-1.0568144211536,1.64735485073218,9.21441620899007));
#61858=CARTESIAN_POINT('Ctrl Pts',(-0.512546116502833,1.99651494094127,
9.17737899216159));
#61859=CARTESIAN_POINT('Ctrl Pts',(0.221865722997436,2.04928064005996,9.14034177533311));
#61860=CARTESIAN_POINT('Ctrl Pts',(0.810458692323854,1.78151382429043,9.10330455850463));
#61861=CARTESIAN_POINT('Ctrl Pts',(1.39905166165026,1.51374700852089,9.06626734167615));
#61862=CARTESIAN_POINT('Ctrl Pts',(1.84182576080283,0.925447677863139,9.02923012484767));
#61863=CARTESIAN_POINT('Ctrl Pts',(1.93623051178265,0.285737974246437,8.99219290801919));
#61864=CARTESIAN_POINT('Ctrl Pts',(2.03063526276248,-0.353971729370283,
8.95515569119071));
#61865=CARTESIAN_POINT('Ctrl Pts',(1.77667066556955,-1.04509180594595,8.91811847436223));
#61866=CARTESIAN_POINT('Ctrl Pts',(1.29051481285208,-1.47146399547075,8.88108125753376));
#61867=CARTESIAN_POINT('Ctrl Pts',(0.804358960134614,-1.89783618499555,
8.84404404070528));
#61868=CARTESIAN_POINT('Ctrl Pts',(0.0860118518926114,-2.05946048746948,
8.8070068238768));
#61869=CARTESIAN_POINT('Ctrl Pts',(-0.535913025040727,-1.88240059832962,
8.76996960704832));
#61870=CARTESIAN_POINT('Ctrl Pts',(-1.15783790197406,-1.70534070918976,
8.73293239021984));
#61871=CARTESIAN_POINT('Ctrl Pts',(-1.68334054759872,-1.18959662843613,
8.69589517339136));
#61872=CARTESIAN_POINT('Ctrl Pts',(-1.87202567450341,-0.571099513462055,
8.65885795656288));
#61873=CARTESIAN_POINT('Ctrl Pts',(-1.92804495632289,-0.387472087407564,
8.64786186841667));
#61874=CARTESIAN_POINT('Ctrl Pts',(-1.95437531748109,-0.194787452297348,
8.63686578027045));
#61875=CARTESIAN_POINT('Ctrl Pts',(-1.95279013340439,-0.00168009551267234,
8.62586969212424));
#61876=CARTESIAN_POINT('Ctrl Pts',(-1.95215444869335,-0.00150235120299324,
8.52413030787576));
#61877=CARTESIAN_POINT('Ctrl Pts',(-1.95371620524508,-0.21958398707372,
8.53653831425035));
#61878=CARTESIAN_POINT('Ctrl Pts',(-1.92001564940553,-0.437196901383431,
8.54894632062494));
#61879=CARTESIAN_POINT('Ctrl Pts',(-1.84897391479539,-0.641847309864828,
8.56135432699953));
#61880=CARTESIAN_POINT('Ctrl Pts',(-1.63677554621959,-1.25312859468192,
8.59841646694325));
#61881=CARTESIAN_POINT('Ctrl Pts',(-1.0914232092448,-1.74875980097234,8.63547860688697));
#61882=CARTESIAN_POINT('Ctrl Pts',(-0.462700104058479,-1.90173108515756,
8.67254074683069));
#61883=CARTESIAN_POINT('Ctrl Pts',(0.166023001127845,-2.05470236934278,
8.70960288677441));
#61884=CARTESIAN_POINT('Ctrl Pts',(0.878116874525705,-1.86501373142281,
8.74666502671813));
#61885=CARTESIAN_POINT('Ctrl Pts',(1.34742707561642,-1.41954668207959,8.78372716666185));
#61886=CARTESIAN_POINT('Ctrl Pts',(1.81673727670714,-0.974079632736377,
8.82078930660557));
#61887=CARTESIAN_POINT('Ctrl Pts',(2.04326380549072,-0.272834171969915,
8.85785144654929));
#61888=CARTESIAN_POINT('Ctrl Pts',(1.92325259761237,0.363004067433246,8.89491358649301));
#61889=CARTESIAN_POINT('Ctrl Pts',(1.80324138973402,0.998842306836407,8.93197572643673));
#61890=CARTESIAN_POINT('Ctrl Pts',(1.33669244519374,1.56927332487627,8.96903786638045));
#61891=CARTESIAN_POINT('Ctrl Pts',(0.737295301650971,1.81302734225987,9.00610000632417));
#61892=CARTESIAN_POINT('Ctrl Pts',(0.137898158108199,2.05678135964346,9.0431621462679));
#61893=CARTESIAN_POINT('Ctrl Pts',(-0.59434718443707,1.9738583763708,9.08022428621162));
#61894=CARTESIAN_POINT('Ctrl Pts',(-1.12405647662483,1.60223891616111,9.11728642615534));
#61895=CARTESIAN_POINT('Ctrl Pts',(-1.63307724594775,1.24513356361944,9.15290105339548));
#61896=CARTESIAN_POINT('Ctrl Pts',(-1.95507366281261,0.621442230158499,
9.18851568063562));
#61897=CARTESIAN_POINT('Ctrl Pts',(-1.95707453392556,-0.000466568259871601,
9.22413030787576));
#61898=CARTESIAN_POINT('Origin',(0.,0.,0.));
#61899=CARTESIAN_POINT('',(-1.95268202714777,0.00165579016441021,10.0258696921242));
#61900=CARTESIAN_POINT('',(-1.9535343393295,0.00178280253715055,9.92413030787576));
#61901=CARTESIAN_POINT('',(-1.954,-2.39295984553393E-16,0.));
#61902=CARTESIAN_POINT('Ctrl Pts',(-1.95268202714777,0.00165579016441021,
10.0258696921242));
#61903=CARTESIAN_POINT('Ctrl Pts',(-1.9542709496717,0.198793394721131,10.0146457155455));
#61904=CARTESIAN_POINT('Ctrl Pts',(-1.92681564478375,0.395498739780043,
10.0034217389668));
#61905=CARTESIAN_POINT('Ctrl Pts',(-1.86848643290836,0.582577638715851,
9.99219776238813));
#61906=CARTESIAN_POINT('Ctrl Pts',(-1.67600993827966,1.1999062383733,9.95516054555966));
#61907=CARTESIAN_POINT('Ctrl Pts',(-1.14735119634562,1.71241362792136,9.91812332873117));
#61908=CARTESIAN_POINT('Ctrl Pts',(-0.524351231736321,1.8856531990772,9.88108611190269));
#61909=CARTESIAN_POINT('Ctrl Pts',(0.0986487328729629,2.05889277023303,
9.84404889507421));
#61910=CARTESIAN_POINT('Ctrl Pts',(0.815989920157508,1.89286452299667,9.80701167824573));
#61911=CARTESIAN_POINT('Ctrl Pts',(1.29952003507049,1.46351732792493,9.76997446141725));
#61912=CARTESIAN_POINT('Ctrl Pts',(1.78305014998348,1.03417013285319,9.73293724458878));
#61913=CARTESIAN_POINT('Ctrl Pts',(2.0327691925249,0.341503989946047,9.69590002776029));
#61914=CARTESIAN_POINT('Ctrl Pts',(1.9344406978275,-0.297614493697593,9.65886281093182));
#61915=CARTESIAN_POINT('Ctrl Pts',(1.8361122031301,-0.936732977341234,9.62182559410334));
#61916=CARTESIAN_POINT('Ctrl Pts',(1.38973617119388,-1.52230380172138,9.58478837727486));
#61917=CARTESIAN_POINT('Ctrl Pts',(0.799511084736072,-1.78645358874384,
9.54775116044638));
#61918=CARTESIAN_POINT('Ctrl Pts',(0.209285998278261,-2.0506033757663,9.5107139436179));
#61919=CARTESIAN_POINT('Ctrl Pts',(-0.524788142701144,-1.99333212543108,
9.47367672678942));
#61920=CARTESIAN_POINT('Ctrl Pts',(-1.06690354347858,-1.6408387214268,9.43663950996094));
#61921=CARTESIAN_POINT('Ctrl Pts',(-1.60735113766186,-1.28942975594381,
9.3997162373487));
#61922=CARTESIAN_POINT('Ctrl Pts',(-1.95701928883641,-0.644612332051665,
9.36279296473647));
#61923=CARTESIAN_POINT('Ctrl Pts',(-1.95719986784682,3.71606954582295E-5,
9.32586969212424));
#61924=CARTESIAN_POINT('Ctrl Pts',(-1.95707453392556,-0.000466568259871601,
9.22413030787576));
#61925=CARTESIAN_POINT('Ctrl Pts',(-1.95715585687005,-0.0257432861687418,
9.22557782057934));
#61926=CARTESIAN_POINT('Ctrl Pts',(-1.95670857405052,-0.0510170594794435,
9.22702533328292));
#61927=CARTESIAN_POINT('Ctrl Pts',(-1.95572375776859,-0.0762698699047084,
9.2284728459865));
#61928=CARTESIAN_POINT('Ctrl Pts',(-1.93050850489432,-0.722843258614067,
9.26553498593022));
#61929=CARTESIAN_POINT('Ctrl Pts',(-1.55290475731554,-1.35567409888606,
9.30259712587394));
#61930=CARTESIAN_POINT('Ctrl Pts',(-0.995863227266852,-1.68491214354887,
9.33965926581766));
#61931=CARTESIAN_POINT('Ctrl Pts',(-0.438821697218168,-2.01415018821168,
9.37672140576139));
#61932=CARTESIAN_POINT('Ctrl Pts',(0.297657615300397,-2.03979543726533,
9.4137835457051));
#61933=CARTESIAN_POINT('Ctrl Pts',(0.876251218790847,-1.75010180082627,
9.45084568564882));
#61934=CARTESIAN_POINT('Ctrl Pts',(1.45484482228131,-1.46040816438721,9.48790782559255));
#61935=CARTESIAN_POINT('Ctrl Pts',(1.87555271674363,-0.855375642455424,
9.52496996553627));
#61936=CARTESIAN_POINT('Ctrl Pts',(1.94568154283725,-0.21212227253196,9.56203210547999));
#61937=CARTESIAN_POINT('Ctrl Pts',(2.01581036893087,0.431131097391505,9.59909424542371));
#61938=CARTESIAN_POINT('Ctrl Pts',(1.73536012665579,1.11260531530666,9.63615638536743));
#61939=CARTESIAN_POINT('Ctrl Pts',(1.23278314419194,1.52017044141902,9.67321852531115));
#61940=CARTESIAN_POINT('Ctrl Pts',(0.730206161728088,1.92773556753138,9.71028066525487));
#61941=CARTESIAN_POINT('Ctrl Pts',(0.00550243907548716,2.06139160184095,
9.74734280519859));
#61942=CARTESIAN_POINT('Ctrl Pts',(-0.609398062732146,1.85992111567971,
9.78440494514231));
#61943=CARTESIAN_POINT('Ctrl Pts',(-1.22429856453979,1.65845062951848,9.82146708508603));
#61944=CARTESIAN_POINT('Ctrl Pts',(-1.72939584550245,1.12185362288641,9.85852922502976));
#61945=CARTESIAN_POINT('Ctrl Pts',(-1.89334427223443,0.495903289718102,
9.89559136497348));
#61946=CARTESIAN_POINT('Ctrl Pts',(-1.93542598326109,0.335236538822793,
9.90510434594091));
#61947=CARTESIAN_POINT('Ctrl Pts',(-1.95503184094814,0.168682937546108,
9.91461732690834));
#61948=CARTESIAN_POINT('Ctrl Pts',(-1.9535343393295,0.00178280253715055,
9.92413030787576));
#61949=CARTESIAN_POINT('Origin',(0.,0.,0.));
#61950=CARTESIAN_POINT('',(-1.95129684289216,-0.00113636086278679,10.7258696921242));
#61951=CARTESIAN_POINT('',(-1.95093054978418,-0.000550606481354719,10.6241303078758));
#61952=CARTESIAN_POINT('',(-1.954,-2.39295984553393E-16,0.));
#61953=CARTESIAN_POINT('Ctrl Pts',(-1.95129684289216,-0.00113636086278679,
10.7258696921242));
#61954=CARTESIAN_POINT('Ctrl Pts',(-1.94942963316978,0.391854106201406,
10.7035356831831));
#61955=CARTESIAN_POINT('Ctrl Pts',(-1.83442754086643,0.785903964976412,
10.6812016742419));
#61956=CARTESIAN_POINT('Ctrl Pts',(-1.61381630858742,1.10744756631717,10.6588676653008));
#61957=CARTESIAN_POINT('Ctrl Pts',(-1.24796949325566,1.64067382739912,10.6218304484723));
#61958=CARTESIAN_POINT('Ctrl Pts',(-0.591690439027595,1.97450300329055,
10.5847932316438));
#61959=CARTESIAN_POINT('Ctrl Pts',(0.0547076636758263,1.95640786233593,
10.5477560148153));
#61960=CARTESIAN_POINT('Ctrl Pts',(0.701105766379276,1.9383127213813,10.5107187979868));
#61961=CARTESIAN_POINT('Ctrl Pts',(1.33762291755807,1.56829326358058,10.4736815811584));
#61962=CARTESIAN_POINT('Ctrl Pts',(1.67312833478204,1.01552035674769,10.4366443643299));
#61963=CARTESIAN_POINT('Ctrl Pts',(2.00863375200599,0.462747449914819,10.3996071475014));
#61964=CARTESIAN_POINT('Ctrl Pts',(2.04312743527515,-0.272778905950186,
10.3625699306729));
#61965=CARTESIAN_POINT('Ctrl Pts',(1.7608042651717,-0.854535269464722,10.3255327138444));
#61966=CARTESIAN_POINT('Ctrl Pts',(1.47848109506825,-1.43629163297926,10.288495497016));
#61967=CARTESIAN_POINT('Ctrl Pts',(0.879341071592168,-1.86427800414334,
10.2514582801875));
#61968=CARTESIAN_POINT('Ctrl Pts',(0.237478981470821,-1.94273555725334,
10.214421063359));
#61969=CARTESIAN_POINT('Ctrl Pts',(-0.404383108650536,-2.02119311036335,
10.1773838465305));
#61970=CARTESIAN_POINT('Ctrl Pts',(-1.08896726541717,-1.75012184541928,
10.140346629702));
#61971=CARTESIAN_POINT('Ctrl Pts',(-1.5031122201388,-1.25351130806383,10.1033094128736));
#61972=CARTESIAN_POINT('Ctrl Pts',(-1.7917522457641,-0.907396556226723,
10.0774961726238));
#61973=CARTESIAN_POINT('Ctrl Pts',(-1.94902777514884,-0.451727225472274,
10.051682932374));
#61974=CARTESIAN_POINT('Ctrl Pts',(-1.95268202714777,0.00165579016441021,
10.0258696921242));
#61975=CARTESIAN_POINT('Ctrl Pts',(-1.9535343393295,0.00178280253715055,
9.92413030787576));
#61976=CARTESIAN_POINT('Ctrl Pts',(-1.94919764294582,-0.481552375812319,
9.95167946685205));
#61977=CARTESIAN_POINT('Ctrl Pts',(-1.76787653021499,-0.967793777264111,
9.97922862582834));
#61978=CARTESIAN_POINT('Ctrl Pts',(-1.44290486192301,-1.32238333502052,
10.0067777848046));
#61979=CARTESIAN_POINT('Ctrl Pts',(-1.00571745237828,-1.79941596688631,
10.0438399247484));
#61980=CARTESIAN_POINT('Ctrl Pts',(-0.308543060787511,-2.03817757091334,
10.0809020646921));
#61981=CARTESIAN_POINT('Ctrl Pts',(0.329297761185238,-1.92930969998698,
10.1179642046358));
#61982=CARTESIAN_POINT('Ctrl Pts',(0.967138583157977,-1.82044182906063,
10.1550263445795));
#61983=CARTESIAN_POINT('Ctrl Pts',(1.5456458355127,-1.36394448318089,10.1920884845232));
#61984=CARTESIAN_POINT('Ctrl Pts',(1.79984980484802,-0.76890421197536,10.229150624467));
#61985=CARTESIAN_POINT('Ctrl Pts',(2.05405377418334,-0.173863940769825,
10.2662127644107));
#61986=CARTESIAN_POINT('Ctrl Pts',(1.98395446049928,0.5597192557615,10.3032749043544));
#61987=CARTESIAN_POINT('Ctrl Pts',(1.62166047466929,1.09585000349956,10.3403370442981));
#61988=CARTESIAN_POINT('Ctrl Pts',(1.2593664888393,1.63198075123761,10.3773991842419));
#61989=CARTESIAN_POINT('Ctrl Pts',(0.604877830863377,1.9706590501824,10.4144613241856));
#61990=CARTESIAN_POINT('Ctrl Pts',(-0.042038551539475,1.95675976549601,
10.4515234641293));
#61991=CARTESIAN_POINT('Ctrl Pts',(-0.688954933942345,1.94286048080962,
10.488585604073));
#61992=CARTESIAN_POINT('Ctrl Pts',(-1.32829904077215,1.57638361249205,10.5256477440167));
#61993=CARTESIAN_POINT('Ctrl Pts',(-1.66723158702796,1.02518946943711,10.5627098839605));
#61994=CARTESIAN_POINT('Ctrl Pts',(-1.85446111291195,0.720704641366568,
10.5831833585989));
#61995=CARTESIAN_POINT('Ctrl Pts',(-1.95001820365716,0.359852200961074,
10.6036568332373));
#61996=CARTESIAN_POINT('Ctrl Pts',(-1.95093054978418,-0.000550606481354719,
10.6241303078758));
#61997=CARTESIAN_POINT('Origin',(0.,0.,-1.29405622560369));
#61998=CARTESIAN_POINT('',(-1.55334812646815,-0.000904610707407963,10.9559437743963));
#61999=CARTESIAN_POINT('',(-1.55659711405804,-0.00105088068675666,11.0940562256037));
#62000=CARTESIAN_POINT('',(-1.5555,-2.01987159101623E-13,-1.29405622560369));
#62001=CARTESIAN_POINT('',(0.499806597877791,1.47301514408978,11.4445));
#62002=CARTESIAN_POINT('Ctrl Pts',(-1.55334812646815,-0.000904610707408108,
10.9559437743963));
#62003=CARTESIAN_POINT('Ctrl Pts',(-1.55432667860164,-0.206859868644216,
10.9706469822836));
#62004=CARTESIAN_POINT('Ctrl Pts',(-1.42041322258558,-0.930327919713715,
11.0223874069994));
#62005=CARTESIAN_POINT('Ctrl Pts',(-0.324962964057439,-1.80887727526569,
11.1111650485437));
#62006=CARTESIAN_POINT('Ctrl Pts',(1.34445241673909,-1.25560970886474,11.2222766990291));
#62007=CARTESIAN_POINT('Ctrl Pts',(1.78171768593789,0.450698535437549,11.3333883495146));
#62008=CARTESIAN_POINT('Ctrl Pts',(0.989503531151977,1.30685679928735,11.4074627831715));
#62009=CARTESIAN_POINT('Ctrl Pts',(0.499806597877626,1.47301514408983,11.4445));
#62010=CARTESIAN_POINT('',(1.55548765964692,0.00619602180124784,11.4445));
#62011=CARTESIAN_POINT('Origin',(0.,0.,11.4445));
#62012=CARTESIAN_POINT('Ctrl Pts',(-1.55659711405804,-0.0010508806867568,
11.0940562256037));
#62013=CARTESIAN_POINT('Ctrl Pts',(-1.55726922058417,-0.079449137192624,
11.099684397238));
#62014=CARTESIAN_POINT('Ctrl Pts',(-1.51630179095532,-0.673453815214831,
11.142374708816));
#62015=CARTESIAN_POINT('Ctrl Pts',(-0.75277483453787,-1.67898453189698,
11.2221271603377));
#62016=CARTESIAN_POINT('Ctrl Pts',(1.00462758039806,-1.53944373403644,11.3333135801688));
#62017=CARTESIAN_POINT('Ctrl Pts',(1.55754888396286,-0.511266487217653,
11.4074378600563));
#62018=CARTESIAN_POINT('Ctrl Pts',(1.55548765964692,0.00619602180124784,
11.4445));
#62019=CARTESIAN_POINT('Origin',(0.,0.,-1.29405622560369));
#62020=CARTESIAN_POINT('',(-1.55445081536763,0.00131810726739325,10.2559437743963));
#62021=CARTESIAN_POINT('',(-1.55305653540906,-0.000438315446397164,10.3940562256037));
#62022=CARTESIAN_POINT('',(-1.5555,-2.01987159101623E-13,-1.29405622560369));
#62023=CARTESIAN_POINT('Ctrl Pts',(-1.55445081536763,0.00131810726739319,
10.2559437743963));
#62024=CARTESIAN_POINT('Ctrl Pts',(-1.55154181384031,-0.359601688445403,
10.2817570146461));
#62025=CARTESIAN_POINT('Ctrl Pts',(-1.24670140973274,-1.24280598265434,
10.3446074717243));
#62026=CARTESIAN_POINT('Ctrl Pts',(0.223056668548975,-1.82477852394609,
10.4444951456311));
#62027=CARTESIAN_POINT('Ctrl Pts',(1.65390974917898,-0.802670846854376,
10.5556067961165));
#62028=CARTESIAN_POINT('Ctrl Pts',(1.57153269033781,0.953897085409752,10.6667184466019));
#62029=CARTESIAN_POINT('Ctrl Pts',(0.0514163720288116,1.83756944970195,
10.7778300970874));
#62030=CARTESIAN_POINT('Ctrl Pts',(-1.30849536725084,1.14582374749785,10.8742385396855));
#62031=CARTESIAN_POINT('Ctrl Pts',(-1.55186171668149,0.311939131113674,
10.9336097654551));
#62032=CARTESIAN_POINT('Ctrl Pts',(-1.55334812646815,-0.000904610707408108,
10.9559437743963));
#62033=CARTESIAN_POINT('Ctrl Pts',(-1.55305653540906,-0.000438315446397077,
10.3940562256037));
#62034=CARTESIAN_POINT('Ctrl Pts',(-1.55364500629154,-0.232901140548306,
10.410644890909));
#62035=CARTESIAN_POINT('Ctrl Pts',(-1.39557528484751,-0.983968830408974,
10.464295696158));
#62036=CARTESIAN_POINT('Ctrl Pts',(-0.231259578302998,-1.82421227428175,
10.5550086413507));
#62037=CARTESIAN_POINT('Ctrl Pts',(1.40774638007895,-1.1829694620695,10.6661950611819));
#62038=CARTESIAN_POINT('Ctrl Pts',(1.75706993010233,0.541796064983141,10.7773814810131));
#62039=CARTESIAN_POINT('Ctrl Pts',(0.497080432048737,1.77049779856472,10.8885679008442));
#62040=CARTESIAN_POINT('Ctrl Pts',(-1.13185991314487,1.39680492671116,10.9941261490411));
#62041=CARTESIAN_POINT('Ctrl Pts',(-1.55284332390808,0.436812153822664,
11.0626222572943));
#62042=CARTESIAN_POINT('Ctrl Pts',(-1.55659711405804,-0.0010508806867568,
11.0940562256037));
#62043=CARTESIAN_POINT('Origin',(0.,0.,-1.29405622560369));
#62044=CARTESIAN_POINT('',(-1.55804728476752,2.95821195149996E-5,9.5559437743963));
#62045=CARTESIAN_POINT('',(-1.55512930646214,0.00141921665610299,9.69405622560371));
#62046=CARTESIAN_POINT('',(-1.5555,-2.01987159101623E-13,-1.29405622560369));
#62047=CARTESIAN_POINT('Ctrl Pts',(-1.55804728476752,2.95821195150548E-5,
9.5559437743963));
#62048=CARTESIAN_POINT('Ctrl Pts',(-1.55790353315504,-0.513149683984934,
9.59286704700854));
#62049=CARTESIAN_POINT('Ctrl Pts',(-1.00033131917675,-1.54135965233235,
9.66682753644926));
#62050=CARTESIAN_POINT('Ctrl Pts',(0.750970673805211,-1.67799333720618,
9.77782524271844));
#62051=CARTESIAN_POINT('Ctrl Pts',(1.81699613594968,-0.279545920640164,
9.88893689320389));
#62052=CARTESIAN_POINT('Ctrl Pts',(1.22062258834496,1.37466418983892,10.0000485436893));
#62053=CARTESIAN_POINT('Ctrl Pts',(-0.492515922639386,1.77116921324136,
10.1111601941748));
#62054=CARTESIAN_POINT('Ctrl Pts',(-1.46173837715872,0.831558022400444,
10.1964586044104));
#62055=CARTESIAN_POINT('Ctrl Pts',(-1.55571569202373,0.15825134364817,10.2447197978176));
#62056=CARTESIAN_POINT('Ctrl Pts',(-1.55445081536763,0.00131810726739319,
10.2559437743963));
#62057=CARTESIAN_POINT('Ctrl Pts',(-1.55512930646214,0.00141921665610296,
9.69405622560371));
#62058=CARTESIAN_POINT('Ctrl Pts',(-1.55167703869094,-0.383344278698275,
9.72160538457999));
#62059=CARTESIAN_POINT('Ctrl Pts',(-1.21314953523015,-1.29115961930375,
9.7862166835));
#62060=CARTESIAN_POINT('Ctrl Pts',(0.309373610575528,-1.81257875466721,
9.88789012236375));
#62061=CARTESIAN_POINT('Ctrl Pts',(1.69095195914933,-0.722381792257861,
9.99907654219489));
#62062=CARTESIAN_POINT('Ctrl Pts',(1.52354231364944,1.0295455294481,10.1102629620261));
#62063=CARTESIAN_POINT('Ctrl Pts',(-0.0394931635484403,1.83836962465064,
10.2214493818572));
#62064=CARTESIAN_POINT('Ctrl Pts',(-1.33855689695156,1.09373648628768,10.3160471363831));
#62065=CARTESIAN_POINT('Ctrl Pts',(-1.5523302537302,0.286463714736223,10.3735827509653));
#62066=CARTESIAN_POINT('Ctrl Pts',(-1.55305653540906,-0.000438315446397077,
10.3940562256037));
#62067=CARTESIAN_POINT('Origin',(0.,0.,-1.29405622560369));
#62068=CARTESIAN_POINT('',(-1.55453687436568,-0.00133745576774406,8.85594377439631));
#62069=CARTESIAN_POINT('',(-1.55794751152569,-0.000371416033132788,8.99405622560372));
#62070=CARTESIAN_POINT('',(-1.5555,-2.01987159101623E-13,-1.29405622560369));
#62071=CARTESIAN_POINT('Ctrl Pts',(-1.55453687436568,-0.00133745576774402,
8.85594377439631));
#62072=CARTESIAN_POINT('Ctrl Pts',(-1.55579877499581,-0.155062375664632,
8.86693986254252));
#62073=CARTESIAN_POINT('Ctrl Pts',(-1.46423861786649,-0.825096309536398,
8.91497316751722));
#62074=CARTESIAN_POINT('Ctrl Pts',(-0.503376402892206,-1.7681153483915,
9.00004368932038));
#62075=CARTESIAN_POINT('Ctrl Pts',(1.2121644264892,-1.38212772940753,9.11115533980582));
#62076=CARTESIAN_POINT('Ctrl Pts',(1.81867711471885,0.26839009932345,9.22226699029127));
#62077=CARTESIAN_POINT('Ctrl Pts',(0.761253709552246,1.67335367481701,9.33337864077668));
#62078=CARTESIAN_POINT('Ctrl Pts',(-0.99265255914171,1.54733978795034,9.44449029126215));
#62079=CARTESIAN_POINT('Ctrl Pts',(-1.55732851093913,0.517959404958592,
9.51867866913534));
#62080=CARTESIAN_POINT('Ctrl Pts',(-1.55804772838109,0.00161323939398619,
9.55582983018006));
#62081=CARTESIAN_POINT('Ctrl Pts',(-1.55804728476752,2.95821195150548E-5,
9.5559437743963));
#62082=CARTESIAN_POINT('Ctrl Pts',(-1.55794751152569,-0.000371416033132616,
8.99405622560372));
#62083=CARTESIAN_POINT('Ctrl Pts',(-1.55801224941728,-0.020493184051098,
8.99550373830729));
#62084=CARTESIAN_POINT('Ctrl Pts',(-1.54853952527048,-0.55575068168544,
9.03401339095459));
#62085=CARTESIAN_POINT('Ctrl Pts',(-0.935609375970031,-1.5829679799695,
9.1095851835456));
#62086=CARTESIAN_POINT('Ctrl Pts',(0.823234386500799,-1.64421340203127,
9.22077160337675));
#62087=CARTESIAN_POINT('Ctrl Pts',(1.82795976495949,-0.199287985657338,
9.33195802320793));
#62088=CARTESIAN_POINT('Ctrl Pts',(1.15819463928053,1.42819381470141,9.44314444303908));
#62089=CARTESIAN_POINT('Ctrl Pts',(-0.572526917402423,1.74738822826618,
9.55433086287024));
#62090=CARTESIAN_POINT('Ctrl Pts',(-1.47990815776177,0.783419353749631,
9.63796812372513));
#62091=CARTESIAN_POINT('Ctrl Pts',(-1.5563214066504,0.1342816322173,9.68454324463628));
#62092=CARTESIAN_POINT('Ctrl Pts',(-1.55512930646214,0.00141921665610296,
9.69405622560371));
#62093=CARTESIAN_POINT('Origin',(0.,0.,-1.29405622560369));
#62094=CARTESIAN_POINT('',(-1.55333906144275,0.000780263919018194,8.15594377439631));
#62095=CARTESIAN_POINT('',(-1.55403083159801,-0.00119596074553197,8.29405622560371));
#62096=CARTESIAN_POINT('',(-1.5555,-2.01987159101623E-13,-1.29405622560369));
#62097=CARTESIAN_POINT('Ctrl Pts',(-1.55333906144275,0.000780263919018167,
8.15594377439631));
#62098=CARTESIAN_POINT('Ctrl Pts',(-1.55193217426013,-0.308862600127516,
8.17804989490498));
#62099=CARTESIAN_POINT('Ctrl Pts',(-1.3122308335565,-1.13929638534857,8.23719323224213));
#62100=CARTESIAN_POINT('Ctrl Pts',(0.0400949547363229,-1.83793690702293,
8.33337378640777));
#62101=CARTESIAN_POINT('Ctrl Pts',(1.56567267939011,-0.963477420579929,
8.44448543689319));
#62102=CARTESIAN_POINT('Ctrl Pts',(1.65879203582308,0.792482593671729,8.55559708737864));
#62103=CARTESIAN_POINT('Ctrl Pts',(0.234256671005791,1.82338791618694,8.66670873786407));
#62104=CARTESIAN_POINT('Ctrl Pts',(-1.24241507899534,1.24912116508194,8.7668243002033));
#62105=CARTESIAN_POINT('Ctrl Pts',(-1.55154841917538,0.362716593952071,
8.82990264571404));
#62106=CARTESIAN_POINT('Ctrl Pts',(-1.55453687436568,-0.00133745576774402,
8.85594377439631));
#62107=CARTESIAN_POINT('Ctrl Pts',(-1.55403083159801,-0.00119596074553188,
8.29405622560371));
#62108=CARTESIAN_POINT('Ctrl Pts',(-1.55527408252746,-0.17480188940304,
8.30646423197829));
#62109=CARTESIAN_POINT('Ctrl Pts',(-1.4483135129372,-0.865473027753662,
8.3559343782966));
#62110=CARTESIAN_POINT('Ctrl Pts',(-0.434704832044991,-1.78666848096071,
8.44246666455862));
#62111=CARTESIAN_POINT('Ctrl Pts',(1.26590215885116,-1.33365823077974,8.55365308438979));
#62112=CARTESIAN_POINT('Ctrl Pts',(1.8068878531032,0.341040818691465,8.66483950422094));
#62113=CARTESIAN_POINT('Ctrl Pts',(0.69268588294083,1.70333168137465,8.77602592405212));
#62114=CARTESIAN_POINT('Ctrl Pts',(-1.03328002592178,1.50787500329959,8.88576483117969));
#62115=CARTESIAN_POINT('Ctrl Pts',(-1.55635469933735,0.494704907375218,
8.95844159836357));
#62116=CARTESIAN_POINT('Ctrl Pts',(-1.55794751152569,-0.000371416033132616,
8.99405622560372));
#62117=CARTESIAN_POINT('Origin',(0.,0.,-1.29405622560369));
#62118=CARTESIAN_POINT('',(-1.55738164088485,0.00090367155389158,7.45594377439631));
#62119=CARTESIAN_POINT('',(-1.55363820104426,0.00100737127591941,7.59405622560371));
#62120=CARTESIAN_POINT('',(-1.5555,-2.01987159101623E-13,-1.29405622560369));
#62121=CARTESIAN_POINT('Ctrl Pts',(-1.55738164088485,0.000903671553891608,
7.45594377439631));
#62122=CARTESIAN_POINT('Ctrl Pts',(-1.55418612064456,-0.461276292775272,
7.48915992726744));
#62123=CARTESIAN_POINT('Ctrl Pts',(-1.09121796390773,-1.44436334125619,
7.55941329696705));
#62124=CARTESIAN_POINT('Ctrl Pts',(0.580004387659595,-1.74448118065669,
7.66670388349515));
#62125=CARTESIAN_POINT('Ctrl Pts',(1.7800908511122,-0.459234407622611,7.77781553398057));
#62126=CARTESIAN_POINT('Ctrl Pts',(1.35154441460109,1.24617309179735,7.88892718446602));
#62127=CARTESIAN_POINT('Ctrl Pts',(-0.313551099181417,1.81143738163968,
8.00003883495145));
#62128=CARTESIAN_POINT('Ctrl Pts',(-1.41757073229054,0.936656796997624,
8.08904436492822));
#62129=CARTESIAN_POINT('Ctrl Pts',(-1.55428931266511,0.209921774117757,
8.1410126780765));
#62130=CARTESIAN_POINT('Ctrl Pts',(-1.55333906144275,0.000780263919018167,
8.15594377439631));
#62131=CARTESIAN_POINT('Ctrl Pts',(-1.55363820104426,0.00100737127591942,
7.59405622560371));
#62132=CARTESIAN_POINT('Ctrl Pts',(-1.55169765832855,-0.326159426902871,
7.6174247256493));
#62133=CARTESIAN_POINT('Ctrl Pts',(-1.29071878250434,-1.17503987929593,
7.67785536563862));
#62134=CARTESIAN_POINT('Ctrl Pts',(0.103792628149562,-1.8358593744105,7.77534814557165));
#62135=CARTESIAN_POINT('Ctrl Pts',(1.59909575810308,-0.907769413831382,
7.8865345654028));
#62136=CARTESIAN_POINT('Ctrl Pts',(1.62955779866738,0.851876712390422,7.99772098523398));
#62137=CARTESIAN_POINT('Ctrl Pts',(0.167274199086701,1.83116681231986,8.10890740506512));
#62138=CARTESIAN_POINT('Ctrl Pts',(-1.26795424285233,1.21093838634352,8.20768581852172));
#62139=CARTESIAN_POINT('Ctrl Pts',(-1.55156054962447,0.343750973057136,
8.26940209203457));
#62140=CARTESIAN_POINT('Ctrl Pts',(-1.55403083159801,-0.00119596074553188,
8.29405622560371));
#62141=CARTESIAN_POINT('Origin',(0.,0.,-1.29405622560369));
#62142=CARTESIAN_POINT('',(-1.55606466149984,-0.00136591087330588,6.7559437743963));
#62143=CARTESIAN_POINT('',(-1.55769406638298,0.000677585252333857,6.89405622560371));
#62144=CARTESIAN_POINT('',(-1.5555,-2.01987159101623E-13,-1.29405622560369));
#62145=CARTESIAN_POINT('Ctrl Pts',(-1.55606466149984,-0.00136591087330577,
6.7559437743963));
#62146=CARTESIAN_POINT('Ctrl Pts',(-1.55699698050756,-0.10301028373747,
6.76323274280142));
#62147=CARTESIAN_POINT('Ctrl Pts',(-1.50160999329305,-0.720125819190329,
6.80755892803501));
#62148=CARTESIAN_POINT('Ctrl Pts',(-0.677079673289082,-1.70914680334463,
6.8889223300971));
#62149=CARTESIAN_POINT('Ctrl Pts',(1.06838781720774,-1.49605051766532,7.00003398058251));
#62150=CARTESIAN_POINT('Ctrl Pts',(1.83637062036826,0.0858057341481814,
7.11114563106797));
#62151=CARTESIAN_POINT('Ctrl Pts',(0.924229284360448,1.589156980696,7.22225728155339));
#62152=CARTESIAN_POINT('Ctrl Pts',(-0.833503847528551,1.63856370505402,
7.33336893203883));
#62153=CARTESIAN_POINT('Ctrl Pts',(-1.53115801604342,0.622214122864029,
7.41126442965314));
#62154=CARTESIAN_POINT('Ctrl Pts',(-1.55774924177056,0.0540711533618156,
7.45212271043896));
#62155=CARTESIAN_POINT('Ctrl Pts',(-1.55738164088485,0.000903671553891608,
7.45594377439631));
#62156=CARTESIAN_POINT('Ctrl Pts',(-1.55769406638298,0.000677585252333878,
6.89405622560371));
#62157=CARTESIAN_POINT('Ctrl Pts',(-1.55508734647919,-0.476733936548398,
6.92838521932031));
#62158=CARTESIAN_POINT('Ctrl Pts',(-1.06472330039144,-1.47419539900055,
6.99977635298063));
#62159=CARTESIAN_POINT('Ctrl Pts',(0.633314188332071,-1.72628667698419,
7.10822962658467));
#62160=CARTESIAN_POINT('Ctrl Pts',(1.7940008868909,-0.403377453646542,7.21941604641583));
#62161=CARTESIAN_POINT('Ctrl Pts',(1.31130494233742,1.28904301731096,7.33060246624699));
#62162=CARTESIAN_POINT('Ctrl Pts',(-0.372603218894873,1.80064416072257,
7.44178888607816));
#62163=CARTESIAN_POINT('Ctrl Pts',(-1.43301362666466,0.901927254173143,
7.52960680586373));
#62164=CARTESIAN_POINT('Ctrl Pts',(-1.55477533406966,0.192722899107996,
7.58036258570558));
#62165=CARTESIAN_POINT('Ctrl Pts',(-1.55363820104426,0.00100737127591942,
7.59405622560371));
#62166=CARTESIAN_POINT('Origin',(0.,0.,-1.29405622560369));
#62167=CARTESIAN_POINT('',(-1.55295085115974,-2.74912889200857E-5,6.0559437743963));
#62168=CARTESIAN_POINT('',(-1.55567057787938,-0.00141549514015751,6.19405622560371));
#62169=CARTESIAN_POINT('',(-1.5555,-2.01987159101623E-13,-1.29405622560369));
#62170=CARTESIAN_POINT('Ctrl Pts',(-1.55295114066544,-2.74881667468134E-5,
6.0559437743963));
#62171=CARTESIAN_POINT('Ctrl Pts',(-1.55299180574127,-0.257905198155464,
6.07434277516388));
#62172=CARTESIAN_POINT('Ctrl Pts',(-1.37005956536857,-1.03483686203599,
6.12977899275993));
#62173=CARTESIAN_POINT('Ctrl Pts',(-0.143272298638598,-1.83278278249422,
6.22225242718446));
#62174=CARTESIAN_POINT('Ctrl Pts',(1.46185859526926,-1.11471481859797,6.33336407766989));
#62175=CARTESIAN_POINT('Ctrl Pts',(1.72951224644592,0.623223129190563,6.44447572815534));
#62176=CARTESIAN_POINT('Ctrl Pts',(0.414808152398764,1.79096450999678,6.55558737864077));
#62177=CARTESIAN_POINT('Ctrl Pts',(-1.1682689842466,1.35101180160119,6.6594100607211));
#62178=CARTESIAN_POINT('Ctrl Pts',(-1.55225961585962,0.413472223515983,
6.72619552597294));
#62179=CARTESIAN_POINT('Ctrl Pts',(-1.55606466149984,-0.00136591087330577,
6.7559437743963));
#62180=CARTESIAN_POINT('Ctrl Pts',(-1.55567057787938,-0.00141549514015748,
6.19405622560371));
#62181=CARTESIAN_POINT('Ctrl Pts',(-1.55673152840384,-0.11622012238534,
6.2022835730476));
#62182=CARTESIAN_POINT('Ctrl Pts',(-1.49271086742403,-0.747018195902368,
6.2475730604352));
#62183=CARTESIAN_POINT('Ctrl Pts',(-0.632665469493242,-1.72652453095426,
6.32992468776653));
#62184=CARTESIAN_POINT('Ctrl Pts',(1.10806726459172,-1.46742614445027,6.44111110759769));
#62185=CARTESIAN_POINT('Ctrl Pts',(1.83376231205259,0.135898253011021,6.55229752742886));
#62186=CARTESIAN_POINT('Ctrl Pts',(0.879651525947856,1.61473395492061,6.66348394726001));
#62187=CARTESIAN_POINT('Ctrl Pts',(-0.880258220622017,1.61440330069759,
6.77467036709119));
#62188=CARTESIAN_POINT('Ctrl Pts',(-1.53940153309356,0.591912849892102,
6.85152779320574));
#62189=CARTESIAN_POINT('Ctrl Pts',(-1.55790160368306,0.0386873070159844,
6.89132307937659));
#62190=CARTESIAN_POINT('Ctrl Pts',(-1.55769406638298,0.000677585252333878,
6.89405622560371));
#62191=CARTESIAN_POINT('Origin',(0.,0.,-1.29405622560369));
#62192=CARTESIAN_POINT('',(-1.55596383579478,0.00138071545366175,5.3559437743963));
#62193=CARTESIAN_POINT('',(-1.5529563387483,0.000151106445085702,5.49405622560371));
#62194=CARTESIAN_POINT('',(-1.5555,-2.01987159101623E-13,-1.29405622560369));
#62195=CARTESIAN_POINT('Ctrl Pts',(-1.55596383579478,0.00138071545366179,
5.3559437743963));
#62196=CARTESIAN_POINT('Ctrl Pts',(-1.55217514150148,-0.410190199764792,
5.38545280752634));
#62197=CARTESIAN_POINT('Ctrl Pts',(-1.17330640529453,-1.34449549172498,
5.45199905748485));
#62198=CARTESIAN_POINT('Ctrl Pts',(0.403262995152723,-1.79359935217008,
5.55558252427184));
#62199=CARTESIAN_POINT('Ctrl Pts',(1.72546185411942,-0.634350903950841,
5.66669417475728));
#62200=CARTESIAN_POINT('Ctrl Pts',(1.46900873501267,1.1052750860401,5.77780582524271));
#62201=CARTESIAN_POINT('Ctrl Pts',(-0.13146340126236,1.83366765077345,5.88891747572816));
#62202=CARTESIAN_POINT('Ctrl Pts',(-1.36655195880861,1.04159698732297,5.98163012544601));
#62203=CARTESIAN_POINT('Ctrl Pts',(-1.55290994688111,0.261203028467153,
6.0373055583354));
#62204=CARTESIAN_POINT('Ctrl Pts',(-1.55295114066544,-2.74881667468134E-5,
6.0559437743963));
#62205=CARTESIAN_POINT('Ctrl Pts',(-1.5529563387483,0.000151106445085633,
5.49405622560371));
#62206=CARTESIAN_POINT('Ctrl Pts',(-1.55272340811799,-0.268780222436924,
5.5132440667186));
#62207=CARTESIAN_POINT('Ctrl Pts',(-1.35831396530156,-1.05747938365068,
5.56949404777722));
#62208=CARTESIAN_POINT('Ctrl Pts',(-0.103102773360761,-1.83589824620028,
5.66280616877956));
#62209=CARTESIAN_POINT('Ctrl Pts',(1.4869956060099,-1.08166382022474,5.77399258861071));
#62210=CARTESIAN_POINT('Ctrl Pts',(1.71494149863546,0.663421591850831,5.88517900844189));
#62211=CARTESIAN_POINT('Ctrl Pts',(0.371926577693494,1.80078404398782,5.99636542827304));
#62212=CARTESIAN_POINT('Ctrl Pts',(-1.18720103315053,1.32645343006727,6.09932450066032));
#62213=CARTESIAN_POINT('Ctrl Pts',(-1.55195221197423,0.40094597399841,6.16522143310387));
#62214=CARTESIAN_POINT('Ctrl Pts',(-1.55567057787938,-0.00141549514015748,
6.19405622560371));
#62215=CARTESIAN_POINT('Origin',(0.,0.,-1.29405622560369));
#62216=CARTESIAN_POINT('',(-1.55745492001379,-0.000856371120316566,4.6559437743963));
#62217=CARTESIAN_POINT('',(-1.55622585425313,0.00134239099646036,4.79405622560371));
#62218=CARTESIAN_POINT('',(-1.5555,-2.01987159101623E-13,-1.29405622560369));
#62219=CARTESIAN_POINT('Ctrl Pts',(-1.55745492001379,-0.000856371120316864,
4.65594377439631));
#62220=CARTESIAN_POINT('Ctrl Pts',(-1.5577850741697,-0.0506891626144068,
4.65952562306032));
#62221=CARTESIAN_POINT('Ctrl Pts',(-1.53301192978291,-0.615473136307116,
4.70014468855281));
#62222=CARTESIAN_POINT('Ctrl Pts',(-0.844041411881997,-1.63316067010957,
4.77780097087378));
#62223=CARTESIAN_POINT('Ctrl Pts',(0.913973507436636,-1.59507746114991,
4.88891262135923));
#62224=CARTESIAN_POINT('Ctrl Pts',(1.83577980123458,-0.0976329900371924,
5.00002427184466));
#62225=CARTESIAN_POINT('Ctrl Pts',(1.0780025055099,1.48913742733129,5.1111359223301));
#62226=CARTESIAN_POINT('Ctrl Pts',(-0.666056105926533,1.7134727727987,5.22224757281553));
#62227=CARTESIAN_POINT('Ctrl Pts',(-1.49938299705611,0.726891414718789,
5.30385019017093));
#62228=CARTESIAN_POINT('Ctrl Pts',(-1.55693038683329,0.106378444150779,
5.34841559069786));
#62229=CARTESIAN_POINT('Ctrl Pts',(-1.55596383579478,0.00138071545366179,
5.3559437743963));
#62230=CARTESIAN_POINT('Ctrl Pts',(-1.55622585425313,0.00134239099646029,
4.79405622560371));
#62231=CARTESIAN_POINT('Ctrl Pts',(-1.55239700220769,-0.418962472451577,
4.82420456038961));
#62232=CARTESIAN_POINT('Ctrl Pts',(-1.15964303797854,-1.36226320639006,
4.89141503511923));
#62233=CARTESIAN_POINT('Ctrl Pts',(0.435376164803608,-1.7865050090601,4.99568764979258));
#62234=CARTESIAN_POINT('Ctrl Pts',(1.73732980498774,-0.602360109052031,
5.10687406962374));
#62235=CARTESIAN_POINT('Ctrl Pts',(1.44781397169404,1.13357278356683,5.21806048945491));
#62236=CARTESIAN_POINT('Ctrl Pts',(-0.167962271460079,1.83110382765203,
5.32924690928607));
#62237=CARTESIAN_POINT('Ctrl Pts',(-1.37758975876034,1.02035875886683,5.42124548800234));
#62238=CARTESIAN_POINT('Ctrl Pts',(-1.55317332364345,0.250672199885809,
5.47618192677488));
#62239=CARTESIAN_POINT('Ctrl Pts',(-1.5529563387483,0.000151106445085633,
5.49405622560371));
#62240=CARTESIAN_POINT('Origin',(0.,0.,-1.29405622560369));
#62241=CARTESIAN_POINT('',(-1.55339129538237,-0.00082587420025254,3.9559437743963));
#62242=CARTESIAN_POINT('',(-1.5573160577951,-0.00094952305265919,4.09405622560371));
#62243=CARTESIAN_POINT('',(-1.5555,-2.01987159101623E-13,-1.29405622560369));
#62244=CARTESIAN_POINT('Ctrl Pts',(-1.55339129538237,-0.000825874200252562,
3.9559437743963));
#62245=CARTESIAN_POINT('Ctrl Pts',(-1.55438295724494,-0.206599346759669,
3.97063565542278));
#62246=CARTESIAN_POINT('Ctrl Pts',(-1.42062281789543,-0.929876204718288,
4.02236475327773));
#62247=CARTESIAN_POINT('Ctrl Pts',(-0.325213021862407,-1.80938005122649,
4.11113106796117));
#62248=CARTESIAN_POINT('Ctrl Pts',(1.34348911316817,-1.25485325124609,4.2222427184466));
#62249=CARTESIAN_POINT('Ctrl Pts',(1.78301209192838,0.447758371671112,4.33335436893204));
#62250=CARTESIAN_POINT('Ctrl Pts',(0.591229481908682,1.74070887258225,4.44446601941748));
#62251=CARTESIAN_POINT('Ctrl Pts',(-1.0856218085317,1.45071736103991,4.55199582123889));
#62252=CARTESIAN_POINT('Ctrl Pts',(-1.55437119708937,0.464594445617744,
4.62248840623184));
#62253=CARTESIAN_POINT('Ctrl Pts',(-1.55745492001379,-0.000856371120316864,
4.65594377439631));
#62254=CARTESIAN_POINT('Ctrl Pts',(-1.5573160577951,-0.000949523052659442,
4.0940562256037));
#62255=CARTESIAN_POINT('Ctrl Pts',(-1.55772052747877,-0.0572626470532979,
4.0981029141169));
#62256=CARTESIAN_POINT('Ctrl Pts',(-1.52938259291224,-0.628915705084586,
4.13921174257381));
#62257=CARTESIAN_POINT('Ctrl Pts',(-0.822616502622442,-1.64452261823584,
4.21738271097444));
#62258=CARTESIAN_POINT('Ctrl Pts',(0.936204134582059,-1.58261630557358,
4.3285691308056));
#62259=CARTESIAN_POINT('Ctrl Pts',(1.83742116834086,-0.0709647969689106,
4.43975555063676));
#62260=CARTESIAN_POINT('Ctrl Pts',(1.0554806974386,1.50569354438759,4.55094197046793));
#62261=CARTESIAN_POINT('Ctrl Pts',(-0.693325883166112,1.70307127625589,
4.66212839029909));
#62262=CARTESIAN_POINT('Ctrl Pts',(-1.50503746143118,0.709862178387775,
4.74316647534435));
#62263=CARTESIAN_POINT('Ctrl Pts',(-1.55710391061042,0.0977293375193425,
4.78714242044589));
#62264=CARTESIAN_POINT('Ctrl Pts',(-1.55622585425313,0.00134239099646029,
4.79405622560371));
#62265=CARTESIAN_POINT('Origin',(0.,0.,-1.29405622560369));
#62266=CARTESIAN_POINT('',(-1.55444674488022,0.00131742778884735,3.2559437743963));
#62267=CARTESIAN_POINT('',(-1.5533186684889,-0.000770198572060954,3.39405622560371));
#62268=CARTESIAN_POINT('',(-1.5555,-2.01987159101623E-13,-1.29405622560369));
#62269=CARTESIAN_POINT('Ctrl Pts',(-1.55444674488022,0.00131742778884739,
3.2559437743963));
#62270=CARTESIAN_POINT('Ctrl Pts',(-1.55154236665719,-0.359445316439912,
3.28174568778523));
#62271=CARTESIAN_POINT('Ctrl Pts',(-1.24691611905359,-1.24248704432008,
3.34458481800264));
#62272=CARTESIAN_POINT('Ctrl Pts',(0.222506403513669,-1.8248590575151,3.44446116504855));
#62273=CARTESIAN_POINT('Ctrl Pts',(1.65365282072159,-0.803151310699741,
3.55557281553397));
#62274=CARTESIAN_POINT('Ctrl Pts',(1.57184646516792,0.953372104320743,3.66668446601942));
#62275=CARTESIAN_POINT('Ctrl Pts',(0.0519332482321354,1.83764050268212,
3.77779611650485));
#62276=CARTESIAN_POINT('Ctrl Pts',(-1.30823935507303,1.14600960175539,3.87421588596382));
#62277=CARTESIAN_POINT('Ctrl Pts',(-1.55188304621527,0.312141358191517,
3.9335984385943));
#62278=CARTESIAN_POINT('Ctrl Pts',(-1.55339129538237,-0.000825874200252562,
3.9559437743963));
#62279=CARTESIAN_POINT('Ctrl Pts',(-1.5533186684889,-0.000770198572060919,
3.39405622560371));
#62280=CARTESIAN_POINT('Ctrl Pts',(-1.5542597194186,-0.210984061911746,
3.4090634077879));
#62281=CARTESIAN_POINT('Ctrl Pts',(-1.41654850766895,-0.939166341982764,
3.46113272991582));
#62282=CARTESIAN_POINT('Ctrl Pts',(-0.308692884081366,-1.81269447386996,
3.55026419198746));
#62283=CARTESIAN_POINT('Ctrl Pts',(1.35606994996762,-1.24186426112907,3.66145061181863));
#62284=CARTESIAN_POINT('Ctrl Pts',(1.77861387826841,0.466567491694538,3.77263703164979));
#62285=CARTESIAN_POINT('Ctrl Pts',(0.571870330903418,1.74760318061885,3.88382345148095));
#62286=CARTESIAN_POINT('Ctrl Pts',(-1.09574509035902,1.43939945308724,3.99096318279893));
#62287=CARTESIAN_POINT('Ctrl Pts',(-1.55401613758806,0.458488658137791,
4.06104077417318));
#62288=CARTESIAN_POINT('Ctrl Pts',(-1.5573160577951,-0.000949523052659442,
4.0940562256037));
#62289=CARTESIAN_POINT('Origin',(0.,0.,-1.29405622560369));
#62290=CARTESIAN_POINT('',(-1.55804712705668,3.25009013604671E-5,2.5559437743963));
#62291=CARTESIAN_POINT('',(-1.55449947323643,0.00133480041304715,2.69405622560371));
#62292=CARTESIAN_POINT('',(-1.5555,-2.01987159101623E-13,-1.29405622560369));
#62293=CARTESIAN_POINT('Ctrl Pts',(-1.55804712705668,3.25009013604029E-5,
2.5559437743963));
#62294=CARTESIAN_POINT('Ctrl Pts',(-1.55788927539753,-0.512989453804214,
2.59285572014769));
#62295=CARTESIAN_POINT('Ctrl Pts',(-1.0006227616332,-1.54106832868198,2.66680488272757));
#62296=CARTESIAN_POINT('Ctrl Pts',(0.750458968510211,-1.67822257683237,
2.77779126213592));
#62297=CARTESIAN_POINT('Ctrl Pts',(1.81691053470019,-0.280099604209337,
2.88890291262136));
#62298=CARTESIAN_POINT('Ctrl Pts',(1.22104229764526,1.37429086670804,3.0000145631068));
#62299=CARTESIAN_POINT('Ctrl Pts',(-0.491976593161155,1.77132117679823,
3.11112621359223));
#62300=CARTESIAN_POINT('Ctrl Pts',(-1.46161229246342,0.831876851886141,
3.19643595068874));
#62301=CARTESIAN_POINT('Ctrl Pts',(-1.55571144064704,0.158409610837222,
3.24470847095676));
#62302=CARTESIAN_POINT('Ctrl Pts',(-1.55444674488022,0.00131742778884739,
3.2559437743963));
#62303=CARTESIAN_POINT('Ctrl Pts',(-1.55449947323643,0.00133480041304701,
2.69405622560371));
#62304=CARTESIAN_POINT('Ctrl Pts',(-1.55153406972295,-0.361714100102126,
2.72002390145891));
#62305=CARTESIAN_POINT('Ctrl Pts',(-1.2437032104418,-1.24745277135715,2.78305371725784));
#62306=CARTESIAN_POINT('Ctrl Pts',(0.231926238140432,-1.82410602009977,
2.88314567300049));
#62307=CARTESIAN_POINT('Ctrl Pts',(1.65866396469461,-0.793716828903688,
2.99433209283165));
#62308=CARTESIAN_POINT('Ctrl Pts',(1.56599354026699,0.96375141196464,3.10551851266282));
#62309=CARTESIAN_POINT('Ctrl Pts',(0.0388050940998321,1.83838154825996,
3.21670493249398));
#62310=CARTESIAN_POINT('Ctrl Pts',(-1.31300314367493,1.13822266482633,3.31288417014094));
#62311=CARTESIAN_POINT('Ctrl Pts',(-1.55193567478298,0.308165737536199,
3.37200126784418));
#62312=CARTESIAN_POINT('Ctrl Pts',(-1.5533186684889,-0.000770198572060919,
3.39405622560371));
#62313=CARTESIAN_POINT('Origin',(0.,0.,-1.29405622560369));
#62314=CARTESIAN_POINT('',(-1.55454118234884,-0.00133834695600709,1.8559437743963));
#62315=CARTESIAN_POINT('',(-1.55805467550008,3.4854191793785E-5,1.9940562256037));
#62316=CARTESIAN_POINT('',(-1.5555,-2.01987159101623E-13,-1.29405622560369));
#62317=CARTESIAN_POINT('Ctrl Pts',(-1.55454118234884,-0.00133834695600729,
1.8559437743963));
#62318=CARTESIAN_POINT('Ctrl Pts',(-1.55580288786201,-0.154903851691022,
1.86692853568168));
#62319=CARTESIAN_POINT('Ctrl Pts',(-1.46436232298065,-0.824775316270878,
1.91495051379553));
#62320=CARTESIAN_POINT('Ctrl Pts',(-0.503915664640746,-1.76796168665343,
2.00000970873786));
#62321=CARTESIAN_POINT('Ctrl Pts',(1.21174280763407,-1.38249741391359,2.1111213592233));
#62322=CARTESIAN_POINT('Ctrl Pts',(1.81875888824183,0.267835396201195,2.22223300970874));
#62323=CARTESIAN_POINT('Ctrl Pts',(0.761764071097843,1.67312138149853,2.33334466019417));
#62324=CARTESIAN_POINT('Ctrl Pts',(-0.992180579104728,1.54764252547341,
2.44445631067961));
#62325=CARTESIAN_POINT('Ctrl Pts',(-1.55725669913861,0.518277207581445,
2.51865601541365));
#62326=CARTESIAN_POINT('Ctrl Pts',(-1.55804766277071,0.0017735852989955,
2.55581850331921));
#62327=CARTESIAN_POINT('Ctrl Pts',(-1.55804712705668,3.25009013604029E-5,
2.5559437743963));
#62328=CARTESIAN_POINT('Ctrl Pts',(-1.55805467550008,3.48541917938314E-5,
1.9940562256037));
#62329=CARTESIAN_POINT('Ctrl Pts',(-1.55788564535512,-0.513206116891616,
2.03098439512992));
#62330=CARTESIAN_POINT('Ctrl Pts',(-1.00003893378143,-1.54186484140614,
2.10497470459985));
#62331=CARTESIAN_POINT('Ctrl Pts',(0.752488571272716,-1.67777039880966,
2.21602715401351));
#62332=CARTESIAN_POINT('Ctrl Pts',(1.81781810074028,-0.276929424335053,
2.32721357384467));
#62333=CARTESIAN_POINT('Ctrl Pts',(1.21794738393109,1.37759091140133,2.43839999367584));
#62334=CARTESIAN_POINT('Ctrl Pts',(-0.497615974795104,1.77017821004958,
2.549586413507));
#62335=CARTESIAN_POINT('Ctrl Pts',(-1.46313162187878,0.828233020270418,
2.63480515748296));
#62336=CARTESIAN_POINT('Ctrl Pts',(-1.55576641614544,0.156444291597347,
2.68296176151519));
#62337=CARTESIAN_POINT('Ctrl Pts',(-1.55449947323643,0.00133480041304701,
2.69405622560371));
#62338=CARTESIAN_POINT('Origin',(0.,0.,-1.29405622560369));
#62339=CARTESIAN_POINT('',(-1.55333634177863,0.000779921548230329,1.1559437743963));
#62340=CARTESIAN_POINT('',(-1.55460191805193,-0.00135568056800359,1.2940562256037));
#62341=CARTESIAN_POINT('',(-1.5555,-2.01987159101623E-13,-1.29405622560369));
#62342=CARTESIAN_POINT('Ctrl Pts',(-1.55333634177863,0.000779921548230561,
1.1559437743963));
#62343=CARTESIAN_POINT('Ctrl Pts',(-1.55193438638927,-0.308706275100063,
1.17803856804414));
#62344=CARTESIAN_POINT('Ctrl Pts',(-1.31241956589738,-1.1389814578602,1.23717057852045));
#62345=CARTESIAN_POINT('Ctrl Pts',(0.0395347168138628,-1.83794704008407,
1.33333980582524));
#62346=CARTESIAN_POINT('Ctrl Pts',(1.56537855283131,-0.963955976349113,
1.44445145631068));
#62347=CARTESIAN_POINT('Ctrl Pts',(1.65903376979378,0.791977165381959,1.55556310679611));
#62348=CARTESIAN_POINT('Ctrl Pts',(0.234812759114929,1.82331608910266,1.66667475728155));
#62349=CARTESIAN_POINT('Ctrl Pts',(-1.24220109658982,1.24943524423025,1.76680164648161));
#62350=CARTESIAN_POINT('Ctrl Pts',(-1.55154880719052,0.362871523529771,
1.8298913188532));
#62351=CARTESIAN_POINT('Ctrl Pts',(-1.55454118234884,-0.00133834695600729,
1.8559437743963));
#62352=CARTESIAN_POINT('Ctrl Pts',(-1.55460191805193,-0.00135568056800364,
1.2940562256037));
#62353=CARTESIAN_POINT('Ctrl Pts',(-1.5558637635503,-0.152693971168416,
1.30488274885721));
#62354=CARTESIAN_POINT('Ctrl Pts',(-1.46605510259419,-0.820638709603335,
1.35277141205443));
#62355=CARTESIAN_POINT('Ctrl Pts',(-0.510374815939226,-1.76654153931159,
1.43772221519537));
#62356=CARTESIAN_POINT('Ctrl Pts',(1.20797626960931,-1.38634273102519,1.54890863502654));
#62357=CARTESIAN_POINT('Ctrl Pts',(1.81976886629041,0.263806680570579,1.6600950548577));
#62358=CARTESIAN_POINT('Ctrl Pts',(0.764574137846417,1.67229745635935,1.77128147468886));
#62359=CARTESIAN_POINT('Ctrl Pts',(-0.991003621173195,1.54889135395602,
1.88246789452002));
#62360=CARTESIAN_POINT('Ctrl Pts',(-1.5572087700955,0.518861158146894,1.95672614482497));
#62361=CARTESIAN_POINT('Ctrl Pts',(-1.55805528871865,0.00189682319971778,
1.9939222551862));
#62362=CARTESIAN_POINT('Ctrl Pts',(-1.55805467550008,3.48541917938314E-5,
1.9940562256037));
#62363=CARTESIAN_POINT('Origin',(0.,0.,-1.29405622560369));
#62364=CARTESIAN_POINT('',(-1.55735926886437,0.00101346774827271,0.455943774396301));
#62365=CARTESIAN_POINT('',(-1.55326046963413,0.000729270061605516,0.594056225603705));
#62366=CARTESIAN_POINT('',(-1.5555,-2.01987159101623E-13,-1.29405622560369));
#62367=CARTESIAN_POINT('Ctrl Pts',(-1.55735926886437,0.00101346774827265,
0.455943774396301));
#62368=CARTESIAN_POINT('Ctrl Pts',(-1.5541538777776,-0.460983628495037,
0.489148600406595));
#62369=CARTESIAN_POINT('Ctrl Pts',(-1.09151218308356,-1.44423481489054,
0.559390643245367));
#62370=CARTESIAN_POINT('Ctrl Pts',(0.579488995883613,-1.74456230311225,
0.666669902912619));
#62371=CARTESIAN_POINT('Ctrl Pts',(1.77994191588978,-0.459827600750814,
0.777781553398056));
#62372=CARTESIAN_POINT('Ctrl Pts',(1.35192905881154,1.24578720765632,0.888893203883492));
#62373=CARTESIAN_POINT('Ctrl Pts',(-0.313001003158473,1.81151906168851,
1.00000485436893));
#62374=CARTESIAN_POINT('Ctrl Pts',(-1.41742497137191,0.93698092273704,1.08902171120653));
#62375=CARTESIAN_POINT('Ctrl Pts',(-1.55428446607623,0.210081433596544,
1.14100135121566));
#62376=CARTESIAN_POINT('Ctrl Pts',(-1.55333634177863,0.000779921548230561,
1.1559437743963));
#62377=CARTESIAN_POINT('Ctrl Pts',(-1.55326046963413,0.000729270061605551,
0.594056225603705));
#62378=CARTESIAN_POINT('Ctrl Pts',(-1.55199262831984,-0.304485333833814,
0.615843242528215));
#62379=CARTESIAN_POINT('Ctrl Pts',(-1.31743653601245,-1.13071739766558,
0.674692399396446));
#62380=CARTESIAN_POINT('Ctrl Pts',(0.0255447675030308,-1.83860034663711,
0.770603696208398));
#62381=CARTESIAN_POINT('Ctrl Pts',(1.55899683301632,-0.975032021788082,
0.881790116039561));
#62382=CARTESIAN_POINT('Ctrl Pts',(1.66434877052597,0.781732535368643,0.992976535870723));
#62383=CARTESIAN_POINT('Ctrl Pts',(0.245080507541896,1.82238325373942,1.10416295570189));
#62384=CARTESIAN_POINT('Ctrl Pts',(-1.23863138927055,1.25487925833816,1.20452285227955));
#62385=CARTESIAN_POINT('Ctrl Pts',(-1.55154412248428,0.365378245899198,
1.26782060891349));
#62386=CARTESIAN_POINT('Ctrl Pts',(-1.55460191805193,-0.00135568056800364,
1.2940562256037));
#62387=CARTESIAN_POINT('Origin',(0.,0.,11.5));
#62388=CARTESIAN_POINT('',(-1.77892626630995,-0.0012009523392913,11.2223275485995));
#62389=CARTESIAN_POINT('Ctrl Pts',(1.55548765964692,0.00619602180104861,
11.4445));
#62390=CARTESIAN_POINT('Ctrl Pts',(1.55843889773201,-0.053546881811892,
11.4417867591843));
#62391=CARTESIAN_POINT('Ctrl Pts',(1.55766805736304,-0.113278156040886,
11.439086160746));
#62392=CARTESIAN_POINT('Ctrl Pts',(1.55338999746751,-0.172741258360748,
11.4363936568093));
#62393=CARTESIAN_POINT('Ctrl Pts',(1.54917978268939,-0.231261344159722,
11.4337438528932));
#62394=CARTESIAN_POINT('Ctrl Pts',(1.54157226362346,-0.289522447371128,
11.4311018887755));
#62395=CARTESIAN_POINT('Ctrl Pts',(1.5307259163647,-0.347284232316321,11.4284634295395));
#62396=CARTESIAN_POINT('Ctrl Pts',(1.52490021612,-0.37830876404678,11.427046282158));
#62397=CARTESIAN_POINT('Ctrl Pts',(1.51813939227042,-0.409189253639797,
11.4256301458963));
#62398=CARTESIAN_POINT('Ctrl Pts',(1.51046300038634,-0.439887833717896,
11.4242143490555));
#62399=CARTESIAN_POINT('Ctrl Pts',(1.50749771858011,-0.451746261786366,
11.4236674467248));
#62400=CARTESIAN_POINT('Ctrl Pts',(1.50439653465153,-0.463574222421597,
11.4231207471528));
#62401=CARTESIAN_POINT('Ctrl Pts',(1.50116353235453,-0.47535996619676,11.4225746575513));
#62402=CARTESIAN_POINT('Ctrl Pts',(1.48455611813741,-0.535901441503565,
11.4197694828629));
#62403=CARTESIAN_POINT('Ctrl Pts',(1.46445634965142,-0.595403551134085,
11.4169769764437));
#62404=CARTESIAN_POINT('Ctrl Pts',(1.4410621824655,-0.653580209875647,11.414192092755));
#62405=CARTESIAN_POINT('Ctrl Pts',(1.41747802435967,-0.712229338392404,
11.4113845922059));
#62406=CARTESIAN_POINT('Ctrl Pts',(1.39054537943373,-0.769532412755046,
11.4085848387028));
#62407=CARTESIAN_POINT('Ctrl Pts',(1.36041578548535,-0.825184282227088,
11.4057876627772));
#62408=CARTESIAN_POINT('Ctrl Pts',(1.35261592294621,-0.839591277975912,
11.4050635379265));
#62409=CARTESIAN_POINT('Ctrl Pts',(1.34460155997405,-0.853887506909652,
11.4043395858183));
#62410=CARTESIAN_POINT('Ctrl Pts',(1.33637481784576,-0.868067413704247,
11.4036157167661));
#62411=CARTESIAN_POINT('Ctrl Pts',(1.33123141939554,-0.87693275912219,11.4031631503791));
#62412=CARTESIAN_POINT('Ctrl Pts',(1.32600576325494,-0.885751206456736,
11.4027106878625));
#62413=CARTESIAN_POINT('Ctrl Pts',(1.32070341258855,-0.894513477947337,
11.4022587210796));
#62414=CARTESIAN_POINT('Ctrl Pts',(1.28755838481391,-0.949286492822766,
11.3994334738427));
#62415=CARTESIAN_POINT('Ctrl Pts',(1.25136992677528,-1.00195372283142,11.3966231054397));
#62416=CARTESIAN_POINT('Ctrl Pts',(1.21232687524415,-1.05222079285711,11.3938225048748));
#62417=CARTESIAN_POINT('Ctrl Pts',(1.17352218779371,-1.10218097437215,11.3910390024248));
#62418=CARTESIAN_POINT('Ctrl Pts',(1.13189715922074,-1.14977118940024,11.3882651489085));
#62419=CARTESIAN_POINT('Ctrl Pts',(1.08759128036108,-1.19468014867466,11.3854959263702));
#62420=CARTESIAN_POINT('Ctrl Pts',(1.05692354853581,-1.22576532190738,11.3835791203762));
#62421=CARTESIAN_POINT('Ctrl Pts',(1.0249704261144,-1.25556541150052,11.3816645331574));
#62422=CARTESIAN_POINT('Ctrl Pts',(0.991767007145199,-1.28396712328559,
11.379750500582));
#62423=CARTESIAN_POINT('Ctrl Pts',(0.971829282858114,-1.30102155672743,
11.378601177562));
#62424=CARTESIAN_POINT('Ctrl Pts',(0.951440575196337,-1.31757160665078,
11.3774520545279));
#62425=CARTESIAN_POINT('Ctrl Pts',(0.930607078503626,-1.33359088746794,
11.3763027711782));
#62426=CARTESIAN_POINT('Ctrl Pts',(0.921822018225176,-1.34034589118487,
11.3758181418501));
#62427=CARTESIAN_POINT('Ctrl Pts',(0.912957575551233,-1.34700657088378,
11.3753334724466));
#62428=CARTESIAN_POINT('Ctrl Pts',(0.904026617991894,-1.35356212132308,
11.3748494000991));
#62429=CARTESIAN_POINT('Ctrl Pts',(0.898865665597572,-1.35735039189889,
11.3745696681303));
#62430=CARTESIAN_POINT('Ctrl Pts',(0.893681522170691,-1.36110432047063,
11.3742900812105));
#62431=CARTESIAN_POINT('Ctrl Pts',(0.888474357058895,-1.36482361432558,
11.3740106343829));
#62432=CARTESIAN_POINT('Ctrl Pts',(0.838811308516624,-1.4002961732508,11.3713454257582));
#62433=CARTESIAN_POINT('Ctrl Pts',(0.787057395286918,-1.43262124116857,
11.368692960317));
#62434=CARTESIAN_POINT('Ctrl Pts',(0.733560484100527,-1.46184200007972,
11.3660489378073));
#62435=CARTESIAN_POINT('Ctrl Pts',(0.677705393253366,-1.49235082960671,
11.3632883650152));
#62436=CARTESIAN_POINT('Ctrl Pts',(0.619949541746925,-1.51947609806138,
11.3605369959002));
#62437=CARTESIAN_POINT('Ctrl Pts',(0.560651932851881,-1.54322365588157,
11.3577899361005));
#62438=CARTESIAN_POINT('Ctrl Pts',(0.511114145446654,-1.56306259192994,
11.3554950161722));
#62439=CARTESIAN_POINT('Ctrl Pts',(0.460499386969577,-1.58054347420583,
11.3532031037542));
#62440=CARTESIAN_POINT('Ctrl Pts',(0.409004561176526,-1.5956447160272,11.3509113452381));
#62441=CARTESIAN_POINT('Ctrl Pts',(0.394571471762801,-1.59987732717035,
11.3502690058367));
#62442=CARTESIAN_POINT('Ctrl Pts',(0.38006920116156,-1.60392285642947,11.3496266785255));
#62443=CARTESIAN_POINT('Ctrl Pts',(0.365502000908426,-1.60778049339754,
11.3489843004725));
#62444=CARTESIAN_POINT('Ctrl Pts',(0.352945849497182,-1.61110557117631,
11.3484306047756));
#62445=CARTESIAN_POINT('Ctrl Pts',(0.340339686983491,-1.61429135213649,
11.3478767954507));
#62446=CARTESIAN_POINT('Ctrl Pts',(0.327707338901135,-1.61733252206154,
11.3473237518226));
#62447=CARTESIAN_POINT('Ctrl Pts',(0.26442068399392,-1.63256844418037,11.3445530649309));
#62448=CARTESIAN_POINT('Ctrl Pts',(0.200363163100888,-1.64421053384351,
11.3417964693365));
#62449=CARTESIAN_POINT('Ctrl Pts',(0.135902532141567,-1.65227549235515,
11.3390491503551));
#62450=CARTESIAN_POINT('Ctrl Pts',(0.0706504004584388,-1.66043947907059,
11.3362680975283));
#62451=CARTESIAN_POINT('Ctrl Pts',(0.00498413291330568,-1.6649382180869,
11.333496550525));
#62452=CARTESIAN_POINT('Ctrl Pts',(-0.0607337043444866,-1.66573959706564,
11.3307295151184));
#62453=CARTESIAN_POINT('Ctrl Pts',(-0.114943810254912,-1.66640064802417,
11.3284470102656));
#62454=CARTESIAN_POINT('Ctrl Pts',(-0.169189647051337,-1.66454499730668,
11.326167575313));
#62455=CARTESIAN_POINT('Ctrl Pts',(-0.223269283792523,-1.66012780789457,
11.3238884070273));
#62456=CARTESIAN_POINT('Ctrl Pts',(-0.242921115785065,-1.65852265909112,
11.3230601871106));
#62457=CARTESIAN_POINT('Ctrl Pts',(-0.262550978640708,-1.65657902103982,
11.3222320024074));
#62458=CARTESIAN_POINT('Ctrl Pts',(-0.282149042864747,-1.65429391513469,
11.3214037184036));
#62459=CARTESIAN_POINT('Ctrl Pts',(-0.293822649715497,-1.65293278948249,
11.3209103501959));
#62460=CARTESIAN_POINT('Ctrl Pts',(-0.305486007024825,-1.65145026241138,
11.3204169024293));
#62461=CARTESIAN_POINT('Ctrl Pts',(-0.317120120921591,-1.64984824722041,
11.3199240638241));
#62462=CARTESIAN_POINT('Ctrl Pts',(-0.382649500838262,-1.64082486451904,
11.3171481404934));
#62463=CARTESIAN_POINT('Ctrl Pts',(-0.447374851901241,-1.62800143931766,
11.3143862955204));
#62464=CARTESIAN_POINT('Ctrl Pts',(-0.510936115769287,-1.6113566500933,
11.3116336908415));
#62465=CARTESIAN_POINT('Ctrl Pts',(-0.573549739883189,-1.59496001930709,
11.3089221249567));
#62466=CARTESIAN_POINT('Ctrl Pts',(-0.635034780101342,-1.57485515271455,
11.3062195258916));
#62467=CARTESIAN_POINT('Ctrl Pts',(-0.695044280650932,-1.55097228857054,
11.3035212687658));
#62468=CARTESIAN_POINT('Ctrl Pts',(-0.755213263935446,-1.52702595273528,
11.3008158406849));
#62469=CARTESIAN_POINT('Ctrl Pts',(-0.813899721511821,-1.49928127162975,
11.2981147776525));
#62470=CARTESIAN_POINT('Ctrl Pts',(-0.870916818143125,-1.46801413582731,
11.2954134178164));
#62471=CARTESIAN_POINT('Ctrl Pts',(-0.88517189274549,-1.46019691292752,
11.2947380399339));
#62472=CARTESIAN_POINT('Ctrl Pts',(-0.8993225020166,-1.4521592870016,11.294062643499));
#62473=CARTESIAN_POINT('Ctrl Pts',(-0.913365468395192,-1.44390514150358,
11.2933871556582));
#62474=CARTESIAN_POINT('Ctrl Pts',(-0.922789553247202,-1.43836587255875,
11.2929338429778));
#62475=CARTESIAN_POINT('Ctrl Pts',(-0.932156968408698,-1.43273389293101,
11.2924808828034));
#62476=CARTESIAN_POINT('Ctrl Pts',(-0.941465939330546,-1.42701150822941,
11.2920283046203));
#62477=CARTESIAN_POINT('Ctrl Pts',(-0.997258564244995,-1.39271482109252,
11.2893158109378));
#62478=CARTESIAN_POINT('Ctrl Pts',(-1.05096555773083,-1.35516769400791,
11.2866164406656));
#62479=CARTESIAN_POINT('Ctrl Pts',(-1.10242222381511,-1.31470157532149,
11.2839256753843));
#62480=CARTESIAN_POINT('Ctrl Pts',(-1.15490559840975,-1.27342804116106,
11.2811812215953));
#62481=CARTESIAN_POINT('Ctrl Pts',(-1.20504870548191,-1.22911724367845,
11.2784457196118));
#62482=CARTESIAN_POINT('Ctrl Pts',(-1.25265335579406,-1.18207076364008,
11.2757143751156));
#62483=CARTESIAN_POINT('Ctrl Pts',(-1.28397500867159,-1.15111636092502,
11.2739172770666));
#62484=CARTESIAN_POINT('Ctrl Pts',(-1.31419725536704,-1.11897666094205,
11.2721219788063));
#62485=CARTESIAN_POINT('Ctrl Pts',(-1.34325581778868,-1.08572815742637,
11.2703271147686));
#62486=CARTESIAN_POINT('Ctrl Pts',(-1.36209363901681,-1.06417411919684,
11.2691635565932));
#62487=CARTESIAN_POINT('Ctrl Pts',(-1.38044228251278,-1.04215395727969,
11.2680001809021));
#62488=CARTESIAN_POINT('Ctrl Pts',(-1.39828252264694,-1.01968718394611,
11.2668366156616));
#62489=CARTESIAN_POINT('Ctrl Pts',(-1.40805056143521,-1.00738598666853,
11.2661995306046));
#62490=CARTESIAN_POINT('Ctrl Pts',(-1.41766921695113,-0.994946604236495,
11.2655621759649));
#62491=CARTESIAN_POINT('Ctrl Pts',(-1.42711662985222,-0.982397385607975,
11.264925758661));
#62492=CARTESIAN_POINT('Ctrl Pts',(-1.46820629310292,-0.927817028752221,
11.262157786839));
#62493=CARTESIAN_POINT('Ctrl Pts',(-1.50612185513061,-0.871087521735772,
11.2594035844773));
#62494=CARTESIAN_POINT('Ctrl Pts',(-1.54066769776793,-0.812525394359864,
11.2566583590267));
#62495=CARTESIAN_POINT('Ctrl Pts',(-1.57505516312501,-0.754231748217875,
11.2539257192103));
#62496=CARTESIAN_POINT('Ctrl Pts',(-1.60610442219133,-0.694121381542228,
11.2512019741836));
#62497=CARTESIAN_POINT('Ctrl Pts',(-1.63358497140864,-0.632471603998023,
11.2484823970106));
#62498=CARTESIAN_POINT('Ctrl Pts',(-1.65966108961598,-0.573972522557314,
11.2459018075444));
#62499=CARTESIAN_POINT('Ctrl Pts',(-1.68252420078453,-0.514086499095208,
11.2433249708101));
#62500=CARTESIAN_POINT('Ctrl Pts',(-1.70193725006908,-0.453031690747441,
11.2407478481942));
#62501=CARTESIAN_POINT('Ctrl Pts',(-1.70639988231082,-0.438996535720931,
11.2401554244947));
#62502=CARTESIAN_POINT('Ctrl Pts',(-1.71068001578898,-0.424899564800969,
11.239562985688));
#62503=CARTESIAN_POINT('Ctrl Pts',(-1.71477442803653,-0.410743347710776,
11.2389704827146));
#62504=CARTESIAN_POINT('Ctrl Pts',(-1.7181060933816,-0.399224288308597,
11.238488356953));
#62505=CARTESIAN_POINT('Ctrl Pts',(-1.72131496051192,-0.387664952239154,
11.2380061462914));
#62506=CARTESIAN_POINT('Ctrl Pts',(-1.72439513423882,-0.376083269559728,
11.2375245092466));
#62507=CARTESIAN_POINT('Ctrl Pts',(-1.73399637264737,-0.339981897872015,
11.2360231938976));
#62508=CARTESIAN_POINT('Ctrl Pts',(-1.74235845090443,-0.303626928305512,
11.234525913273));
#62509=CARTESIAN_POINT('Ctrl Pts',(-1.74944665354966,-0.267065873422436,
11.2330319031487));
#62510=CARTESIAN_POINT('Ctrl Pts',(-1.76197449586933,-0.202447076028902,
11.2303913574139));
#62511=CARTESIAN_POINT('Ctrl Pts',(-1.77052625497235,-0.137185361680741,
11.227761027999));
#62512=CARTESIAN_POINT('Ctrl Pts',(-1.77528061829343,-0.0715870718432795,
11.2251366955952));
#62513=CARTESIAN_POINT('Ctrl Pts',(-1.77697828156189,-0.0481635764959884,
11.2241996126621));
#62514=CARTESIAN_POINT('Ctrl Pts',(-1.7781912975682,-0.0246970169190114,
11.2232632943623));
#62515=CARTESIAN_POINT('Ctrl Pts',(-1.77892626630995,-0.00120095233929127,
11.2223275485995));
#62516=CARTESIAN_POINT('',(1.88128289424299,-0.51655738433239,11.046));
#62517=CARTESIAN_POINT('Ctrl Pts',(1.88079991776263,-0.516378774142054,
11.046));
#62518=CARTESIAN_POINT('Ctrl Pts',(1.89035995045861,-0.445151004206684,
11.0555631104642));
#62519=CARTESIAN_POINT('Ctrl Pts',(1.8961423315859,-0.373654493774377,11.0651669654983));
#62520=CARTESIAN_POINT('Ctrl Pts',(1.89809144951916,-0.302224012343752,
11.0748303404806));
#62521=CARTESIAN_POINT('Ctrl Pts',(1.89999077178002,-0.23261842246626,11.0842468375051));
#62522=CARTESIAN_POINT('Ctrl Pts',(1.89824990827702,-0.163074621232238,
11.0937198521185));
#62523=CARTESIAN_POINT('Ctrl Pts',(1.89277099599951,-0.0939167257851171,
11.1032667571406));
#62524=CARTESIAN_POINT('Ctrl Pts',(1.88910201129244,-0.0476047485319078,
11.1096598962807));
#62525=CARTESIAN_POINT('Ctrl Pts',(1.8837557967888,-0.00146614169388357,
11.1160861707414));
#62526=CARTESIAN_POINT('Ctrl Pts',(1.87669176161129,0.0443950771863014,
11.1225507975725));
#62527=CARTESIAN_POINT('Ctrl Pts',(1.87063241478827,0.0837336455737761,
11.1280959874063));
#62528=CARTESIAN_POINT('Ctrl Pts',(1.8633089856103,0.122868068816038,11.1336693960131));
#62529=CARTESIAN_POINT('Ctrl Pts',(1.85469071090361,0.161728394728602,11.1392743160301));
#62530=CARTESIAN_POINT('Ctrl Pts',(1.85223436103037,0.172804226014781,11.1408718103131));
#62531=CARTESIAN_POINT('Ctrl Pts',(1.84967323324123,0.183855475695868,11.142471538338));
#62532=CARTESIAN_POINT('Ctrl Pts',(1.84700939076218,0.19487013146115,11.1440720571876));
#62533=CARTESIAN_POINT('Ctrl Pts',(1.83137216521354,0.259528105007685,11.1534673853433));
#62534=CARTESIAN_POINT('Ctrl Pts',(1.81217652429567,0.323030635926077,11.1629048835303));
#62535=CARTESIAN_POINT('Ctrl Pts',(1.78934255453511,0.385087390709459,11.1724028038701));
#62536=CARTESIAN_POINT('Ctrl Pts',(1.78198218565347,0.405090947322401,11.1754643914102));
#62537=CARTESIAN_POINT('Ctrl Pts',(1.77424343060636,0.424944079046285,11.1785322571122));
#62538=CARTESIAN_POINT('Ctrl Pts',(1.76612263817241,0.444636415640588,11.181607012295));
#62539=CARTESIAN_POINT('Ctrl Pts',(1.73919119835162,0.509943216945239,11.1918039955137));
#62540=CARTESIAN_POINT('Ctrl Pts',(1.70806080167302,0.573485248201441,11.2020767507448));
#62541=CARTESIAN_POINT('Ctrl Pts',(1.67301702698032,0.634984575310704,11.2124475752393));
#62542=CARTESIAN_POINT('Ctrl Pts',(1.64235372412421,0.688796486531309,11.2215220466721));
#62543=CARTESIAN_POINT('Ctrl Pts',(1.60869302252863,0.741044106677185,11.2306716023846));
#62544=CARTESIAN_POINT('Ctrl Pts',(1.57220891785208,0.791506873950779,11.239911179793));
#62545=CARTESIAN_POINT('Ctrl Pts',(1.56528521292053,0.801083354276364,11.2416646038728));
#62546=CARTESIAN_POINT('Ctrl Pts',(1.55825911602623,0.81059620160376,11.2434214216921));
#62547=CARTESIAN_POINT('Ctrl Pts',(1.55114206425445,0.820030590825838,11.2451792455347));
#62548=CARTESIAN_POINT('Ctrl Pts',(1.51163333781795,0.872403499555923,11.254937412757));
#62549=CARTESIAN_POINT('Ctrl Pts',(1.46925448012712,0.922460374176763,11.2647444648472));
#62550=CARTESIAN_POINT('Ctrl Pts',(1.42425895086728,0.969999034377404,11.2746213834588));
#62551=CARTESIAN_POINT('Ctrl Pts',(1.37955552976012,1.01722907657888,11.2844341817346));
#62552=CARTESIAN_POINT('Ctrl Pts',(1.33226826113497,1.06197396880102,11.2943159423384));
#62553=CARTESIAN_POINT('Ctrl Pts',(1.28262305484525,1.10398985376236,11.3042872409362));
#62554=CARTESIAN_POINT('Ctrl Pts',(1.23402945162958,1.14511574274852,11.3140473238087));
#62555=CARTESIAN_POINT('Ctrl Pts',(1.18317581682196,1.18362727550242,11.3238931915966));
#62556=CARTESIAN_POINT('Ctrl Pts',(1.13026675802768,1.2192467284131,11.3338441399431));
#62557=CARTESIAN_POINT('Ctrl Pts',(1.11612186853279,1.22876935528969,11.3365044606506));
#62558=CARTESIAN_POINT('Ctrl Pts',(1.1018300740637,1.23808499004259,11.3391722917297));
#62559=CARTESIAN_POINT('Ctrl Pts',(1.0873953214649,1.24718768011963,11.3418480018757));
#62560=CARTESIAN_POINT('Ctrl Pts',(1.07843141524914,1.25284040326838,11.3435096039465));
#62561=CARTESIAN_POINT('Ctrl Pts',(1.06941317684967,1.25841040829158,11.3451740914355));
#62562=CARTESIAN_POINT('Ctrl Pts',(1.06035226952456,1.2638900735973,11.346839603865));
#62563=CARTESIAN_POINT('Ctrl Pts',(1.00742079701965,1.29590085828569,11.3565690958694));
#62564=CARTESIAN_POINT('Ctrl Pts',(0.952938092487177,1.32489391547385,11.3663514013733));
#62565=CARTESIAN_POINT('Ctrl Pts',(0.897108858642945,1.35066478023243,11.3762079140514));
#62566=CARTESIAN_POINT('Ctrl Pts',(0.842238965806958,1.37599281162795,11.3858950574554));
#62567=CARTESIAN_POINT('Ctrl Pts',(0.78606756226141,1.39820862213323,11.3956538796688));
#62568=CARTESIAN_POINT('Ctrl Pts',(0.72878604220227,1.41706842320411,11.4055046903548));
#62569=CARTESIAN_POINT('Ctrl Pts',(0.67317444208947,1.43537840719681,11.4150683217683));
#62570=CARTESIAN_POINT('Ctrl Pts',(0.616515828164059,1.45052520284418,11.4247186563809));
#62571=CARTESIAN_POINT('Ctrl Pts',(0.558993687390787,1.46223733220615,11.4344742788813));
#62572=CARTESIAN_POINT('Ctrl Pts',(0.539362537898783,1.46623444634835,11.4378036765901));
#62573=CARTESIAN_POINT('Ctrl Pts',(0.519630929867265,1.46983109384517,11.4411453373854));
#62574=CARTESIAN_POINT('Ctrl Pts',(0.499806597877626,1.47301514408983,11.4445));
#62575=CARTESIAN_POINT('',(1.56060797133591,1.17265290216009,11.046));
#62576=CARTESIAN_POINT('Origin',(0.,0.,11.046));
#62577=CARTESIAN_POINT('Ctrl Pts',(-1.77892626630995,-0.00120095233929127,
11.2223275485995));
#62578=CARTESIAN_POINT('Ctrl Pts',(-1.78091222637221,0.0622877965358305,
11.2197990686688));
#62579=CARTESIAN_POINT('Ctrl Pts',(-1.77941067542291,0.125992016111799,
11.2172747683064));
#62580=CARTESIAN_POINT('Ctrl Pts',(-1.77452381634337,0.189646102027163,
11.2147508586347));
#62581=CARTESIAN_POINT('Ctrl Pts',(-1.77287868795546,0.211074823838332,
11.2139012013432));
#62582=CARTESIAN_POINT('Ctrl Pts',(-1.7708495726434,0.232497857027148,11.2130515883281));
#62583=CARTESIAN_POINT('Ctrl Pts',(-1.76843936997923,0.253904972833394,
11.2122018750387));
#62584=CARTESIAN_POINT('Ctrl Pts',(-1.76712267121633,0.265599725029338,
11.2117376748892));
#62585=CARTESIAN_POINT('Ctrl Pts',(-1.76569197102713,0.277291668505868,
11.2112733675823));
#62586=CARTESIAN_POINT('Ctrl Pts',(-1.7641484990815,0.288972974548762,11.2108091738099));
#62587=CARTESIAN_POINT('Ctrl Pts',(-1.75515036560026,0.357072658062498,
11.2081030167356));
#62588=CARTESIAN_POINT('Ctrl Pts',(-1.74235696629666,0.42456963250346,11.2054102736121));
#62589=CARTESIAN_POINT('Ctrl Pts',(-1.72594903242932,0.491138664005795,
11.2027264834948));
#62590=CARTESIAN_POINT('Ctrl Pts',(-1.70928395222888,0.558750970212142,
11.2000006328234));
#62591=CARTESIAN_POINT('Ctrl Pts',(-1.68888999030711,0.625407040269523,
11.1972840179815));
#62592=CARTESIAN_POINT('Ctrl Pts',(-1.66490278446929,0.690766734877331,
11.1945719649831));
#62593=CARTESIAN_POINT('Ctrl Pts',(-1.64112198461878,0.755564019991226,
11.1918832487577));
#62594=CARTESIAN_POINT('Ctrl Pts',(-1.61380916520598,0.81908815011939,11.1891990162058));
#62595=CARTESIAN_POINT('Ctrl Pts',(-1.5830482712126,0.880993120829078,11.186514712963));
#62596=CARTESIAN_POINT('Ctrl Pts',(-1.57216641681974,0.902892382846704,
11.1855651242728));
#62597=CARTESIAN_POINT('Ctrl Pts',(-1.56085264019442,0.92458881232314,11.1846155267362));
#62598=CARTESIAN_POINT('Ctrl Pts',(-1.54910931637308,0.946066284278751,
11.1836657187303));
#62599=CARTESIAN_POINT('Ctrl Pts',(-1.54396572241992,0.955473450134084,
11.1832497013582));
#62600=CARTESIAN_POINT('Ctrl Pts',(-1.53874121405367,0.964835754579395,
11.1828337685169));
#62601=CARTESIAN_POINT('Ctrl Pts',(-1.5334404792476,0.974144495398925,11.18241823656));
#62602=CARTESIAN_POINT('Ctrl Pts',(-1.49854818334159,1.03541964895223,11.179682981066));
#62603=CARTESIAN_POINT('Ctrl Pts',(-1.46030493742689,1.09447092650475,11.1769608571821));
#62604=CARTESIAN_POINT('Ctrl Pts',(-1.41884997832206,1.15095727599886,11.1742472453603));
#62605=CARTESIAN_POINT('Ctrl Pts',(-1.37811238995456,1.20646613920276,11.1715805921112));
#62606=CARTESIAN_POINT('Ctrl Pts',(-1.33427285188376,1.25949901944966,11.1689221588738));
#62607=CARTESIAN_POINT('Ctrl Pts',(-1.28741864153,1.30971119589593,11.166267561795));
#62608=CARTESIAN_POINT('Ctrl Pts',(-1.26549062822221,1.33321075474058,11.1650251966024));
#62609=CARTESIAN_POINT('Ctrl Pts',(-1.24290170835111,1.35609210845284,11.1637836716393));
#62610=CARTESIAN_POINT('Ctrl Pts',(-1.21965775424868,1.37831740927343,11.1625425375316));
#62611=CARTESIAN_POINT('Ctrl Pts',(-1.19165584264812,1.40509215276722,11.1610473475387));
#62612=CARTESIAN_POINT('Ctrl Pts',(-1.16270333140537,1.43091488294274,11.1595527247918));
#62613=CARTESIAN_POINT('Ctrl Pts',(-1.13285929301872,1.45577404177113,11.1580578836196));
#62614=CARTESIAN_POINT('Ctrl Pts',(-1.12175109882477,1.46502682318719,11.1575014915585));
#62615=CARTESIAN_POINT('Ctrl Pts',(-1.11051936159011,1.47414607111053,11.156945069237));
#62616=CARTESIAN_POINT('Ctrl Pts',(-1.09916702235175,1.48313103947397,11.1563885761416));
#62617=CARTESIAN_POINT('Ctrl Pts',(-1.0900493418525,1.49034735578674,11.1559416262983));
#62618=CARTESIAN_POINT('Ctrl Pts',(-1.08085382696811,1.49747696130526,11.1554946319594));
#62619=CARTESIAN_POINT('Ctrl Pts',(-1.07159363370462,1.50451093778695,11.1550481251347));
#62620=CARTESIAN_POINT('Ctrl Pts',(-1.01611106549685,1.54665509923293,11.152372873695));
#62621=CARTESIAN_POINT('Ctrl Pts',(-0.958209601759993,1.58545013781557,
11.1497101571816));
#62622=CARTESIAN_POINT('Ctrl Pts',(-0.898278760372612,1.62088563165273,
11.1470556568828));
#62623=CARTESIAN_POINT('Ctrl Pts',(-0.837571419107242,1.65678024897295,
11.1443667632881));
#62624=CARTESIAN_POINT('Ctrl Pts',(-0.774780874239298,1.6892280755481,11.1416863001956));
#62625=CARTESIAN_POINT('Ctrl Pts',(-0.71027313016202,1.71817742298682,11.1390097788418));
#62626=CARTESIAN_POINT('Ctrl Pts',(-0.66261429365752,1.73956543207362,11.13703234349));
#62627=CARTESIAN_POINT('Ctrl Pts',(-0.614017264977652,1.75904301818697,
11.135057059686));
#62628=CARTESIAN_POINT('Ctrl Pts',(-0.56462073685077,1.77657345707156,11.1330821172509));
#62629=CARTESIAN_POINT('Ctrl Pts',(-0.539231747042784,1.78558380964183,
11.1320670298498));
#62630=CARTESIAN_POINT('Ctrl Pts',(-0.513631449727103,1.79407954038564,
11.1310520326313));
#62631=CARTESIAN_POINT('Ctrl Pts',(-0.487838223654543,1.802054170041,11.1300368798027));
#62632=CARTESIAN_POINT('Ctrl Pts',(-0.475799003301229,1.80577640018727,
11.1295630480858));
#62633=CARTESIAN_POINT('Ctrl Pts',(-0.463717747565173,1.80938508638487,
11.129089182467));
#62634=CARTESIAN_POINT('Ctrl Pts',(-0.451596312388482,1.81287949077367,
11.1286152579519));
#62635=CARTESIAN_POINT('Ctrl Pts',(-0.439480899976025,1.81637215890158,
11.1281415689151));
#62636=CARTESIAN_POINT('Ctrl Pts',(-0.427332434103985,1.81974856717366,
11.1276680985874));
#62637=CARTESIAN_POINT('Ctrl Pts',(-0.415160020480683,1.8230065701324,11.1271950974533));
#62638=CARTESIAN_POINT('Ctrl Pts',(-0.345659931193023,1.8416085913534,11.1244944316633));
#62639=CARTESIAN_POINT('Ctrl Pts',(-0.275309825422015,1.85637496302517,
11.1218062647546));
#62640=CARTESIAN_POINT('Ctrl Pts',(-0.204481476884407,1.86725830113956,
11.1191261497819));
#62641=CARTESIAN_POINT('Ctrl Pts',(-0.133579826115251,1.87815290272383,
11.1164432610836));
#62642=CARTESIAN_POINT('Ctrl Pts',(-0.0621979169225611,1.88515673586772,
11.1137684409964));
#62643=CARTESIAN_POINT('Ctrl Pts',(0.00930939936232982,1.88817434312463,
11.111097228754));
#62644=CARTESIAN_POINT('Ctrl Pts',(0.0795378313902503,1.89113798149254,
11.1084737902425));
#62645=CARTESIAN_POINT('Ctrl Pts',(0.149888204683991,1.89025686041538,11.1058538316796));
#62646=CARTESIAN_POINT('Ctrl Pts',(0.220026910137412,1.88539116319202,11.1032331273822));
#62647=CARTESIAN_POINT('Ctrl Pts',(0.236366392955163,1.88425765244837,11.1026226092302));
#62648=CARTESIAN_POINT('Ctrl Pts',(0.252694364144288,1.88290767750495,11.102012050607));
#62649=CARTESIAN_POINT('Ctrl Pts',(0.269006539233807,1.88133906123029,11.1014013980884));
#62650=CARTESIAN_POINT('Ctrl Pts',(0.280730896030037,1.88021162011471,11.1009624923038));
#62651=CARTESIAN_POINT('Ctrl Pts',(0.292446914187848,1.8789711508204,11.1005235443156));
#62652=CARTESIAN_POINT('Ctrl Pts',(0.304138944100939,1.87761870427971,11.1000850620809));
#62653=CARTESIAN_POINT('Ctrl Pts',(0.375822773838615,1.86932685519343,11.0973967277121));
#62654=CARTESIAN_POINT('Ctrl Pts',(0.446738242932316,1.85681796775178,11.0947208906731));
#62655=CARTESIAN_POINT('Ctrl Pts',(0.516529562716851,1.84000805096474,11.0920531719144));
#62656=CARTESIAN_POINT('Ctrl Pts',(0.584847521294231,1.82355300752536,11.0894417712386));
#62657=CARTESIAN_POINT('Ctrl Pts',(0.652089317501138,1.80297695165361,11.0868381496919));
#62658=CARTESIAN_POINT('Ctrl Pts',(0.718036401553849,1.77856692481578,11.084238199749));
#62659=CARTESIAN_POINT('Ctrl Pts',(0.785323202313169,1.75366100765569,11.0815854317561));
#62660=CARTESIAN_POINT('Ctrl Pts',(0.851262956271168,1.7247633139281,11.0789364860598));
#62661=CARTESIAN_POINT('Ctrl Pts',(0.915607648721953,1.6921267735849,11.0762869996812));
#62662=CARTESIAN_POINT('Ctrl Pts',(0.930631108062465,1.68450666199239,11.0756683868732));
#62663=CARTESIAN_POINT('Ctrl Pts',(0.945567515715628,1.67668252571399,11.0750497445899));
#62664=CARTESIAN_POINT('Ctrl Pts',(0.960413518624615,1.6686572293506,11.074431017298));
#62665=CARTESIAN_POINT('Ctrl Pts',(0.975205360081844,1.66066121101609,11.073814547258));
#62666=CARTESIAN_POINT('Ctrl Pts',(0.989912270604597,1.65246257743845,11.0731977870787));
#62667=CARTESIAN_POINT('Ctrl Pts',(1.00450295029956,1.6440805277344,11.0725818668126));
#62668=CARTESIAN_POINT('Ctrl Pts',(1.06739734574523,1.60794897253934,11.0699268888682));
#62669=CARTESIAN_POINT('Ctrl Pts',(1.12821828188749,1.56837054324493,11.0672840147147));
#62670=CARTESIAN_POINT('Ctrl Pts',(1.18673956352194,1.52565231730803,11.0646490274931));
#62671=CARTESIAN_POINT('Ctrl Pts',(1.24608357911593,1.48233352805146,11.0619769957398));
#62672=CARTESIAN_POINT('Ctrl Pts',(1.30306365724006,1.43578546725283,11.0593130742375));
#62673=CARTESIAN_POINT('Ctrl Pts',(1.35742307425591,1.38627866511896,11.056652865764));
#62674=CARTESIAN_POINT('Ctrl Pts',(1.41159294455999,1.3369444890372,11.0540019332135));
#62675=CARTESIAN_POINT('Ctrl Pts',(1.4631611896777,1.28467147000892,11.0513546878431));
#62676=CARTESIAN_POINT('Ctrl Pts',(1.51184108762766,1.22968809505141,11.0487067782687));
#62677=CARTESIAN_POINT('Ctrl Pts',(1.52842600119773,1.21095562929319,11.0478046532996));
#62678=CARTESIAN_POINT('Ctrl Pts',(1.54467532477781,1.19190827830405,11.0469024512351));
#62679=CARTESIAN_POINT('Ctrl Pts',(1.56057659382849,1.17255425406029,11.046));
#62680=CARTESIAN_POINT('',(-0.999999999999999,-1.22464679914735E-16,12.));
#62681=CARTESIAN_POINT('',(-1.5,-1.83697019872103E-16,11.5));
#62682=CARTESIAN_POINT('Origin',(0.,0.,12.));
#62683=CARTESIAN_POINT('Ctrl Pts',(1.13509973994371,-1.59049193030953,-0.230074082272069));
#62684=CARTESIAN_POINT('Ctrl Pts',(1.66385127640631,-1.21313337847033,-0.19303686544359));
#62685=CARTESIAN_POINT('Ctrl Pts',(2.30633516687349,0.103782615975306,-0.118962431786632));
#62686=CARTESIAN_POINT('Ctrl Pts',(1.16188988078006,1.99753850566951,-0.00785078130119459));
#62687=CARTESIAN_POINT('Ctrl Pts',(-1.04655428901899,2.05782953697956,0.103260869184242));
#62688=CARTESIAN_POINT('Ctrl Pts',(-2.29698075471667,0.238333788527267,
0.214372519669679));
#62689=CARTESIAN_POINT('Ctrl Pts',(-1.44613108848303,-1.80075271725216,
0.325484170155115));
#62690=CARTESIAN_POINT('Ctrl Pts',(0.727946961077783,-2.19149774367173,
0.436595820640553));
#62691=CARTESIAN_POINT('Ctrl Pts',(2.2359411788162,-0.57762978583554,0.547707471125989));
#62692=CARTESIAN_POINT('Ctrl Pts',(1.69827668332871,1.56494259322429,0.658819121611427));
#62693=CARTESIAN_POINT('Ctrl Pts',(-0.393188016825179,2.27560800163251,
0.769930772096863));
#62694=CARTESIAN_POINT('Ctrl Pts',(-2.12490816724285,0.90434536960108,0.881042422582301));
#62695=CARTESIAN_POINT('Ctrl Pts',(-1.9125222930514,-1.29434912039326,0.992154073067737));
#62696=CARTESIAN_POINT('Ctrl Pts',(0.0496630258143332,-2.30880650358359,
1.10326572355317));
#62697=CARTESIAN_POINT('Ctrl Pts',(1.96640931676781,-1.21090966106477,1.21437737403861));
#62698=CARTESIAN_POINT('Ctrl Pts',(2.08405785032279,0.994871990457256,1.32548902452405));
#62699=CARTESIAN_POINT('Ctrl Pts',(0.294968904732024,2.29042728261432,1.43660067500948));
#62700=CARTESIAN_POINT('Ctrl Pts',(-1.76399147035948,1.49043619583305,1.54771232549492));
#62701=CARTESIAN_POINT('Ctrl Pts',(-2.20904863824581,-0.673178902258552,
1.65882397598036));
#62702=CARTESIAN_POINT('Ctrl Pts',(-0.633012670336293,-2.22089176195486,
1.7699356264658));
#62703=CARTESIAN_POINT('Ctrl Pts',(1.52217643594786,-1.73667627565877,1.88104727695123));
#62704=CARTESIAN_POINT('Ctrl Pts',(2.28470258285089,0.336451535954383,1.99215892743667));
#62705=CARTESIAN_POINT('Ctrl Pts',(0.956918672404541,2.10175453516431,2.10327057792211));
#62706=CARTESIAN_POINT('Ctrl Pts',(-1.24636506047609,1.94412953698174,2.21438222840754));
#62707=CARTESIAN_POINT('Ctrl Pts',(-2.30932995110325,0.00779007092406014,
2.32549387889298));
#62708=CARTESIAN_POINT('Ctrl Pts',(-1.2594528285163,-1.93567664513544,2.43660552937842));
#62709=CARTESIAN_POINT('Ctrl Pts',(0.942717341349318,-2.1081625941051,2.54771717986386));
#62710=CARTESIAN_POINT('Ctrl Pts',(2.28238070382781,-0.351857683462,2.65882883034929));
#62711=CARTESIAN_POINT('Ctrl Pts',(1.53385834111148,1.72636731182735,2.76994048083473));
#62712=CARTESIAN_POINT('Ctrl Pts',(-0.618014955343493,2.22511191222357,
2.88105213132016));
#62713=CARTESIAN_POINT('Ctrl Pts',(-2.20445672440028,0.68806689849701,2.99216378180561));
#62714=CARTESIAN_POINT('Ctrl Pts',(-1.77400663329184,-1.47850125855229,
3.10327543229104));
#62715=CARTESIAN_POINT('Ctrl Pts',(0.279509811935462,-2.29236554058792,
3.21438708277648));
#62716=CARTESIAN_POINT('Ctrl Pts',(2.07729836817097,-1.00890881459812,3.32549873326191));
#62717=CARTESIAN_POINT('Ctrl Pts',(1.97453422882556,1.1976143309821,3.43661038374735));
#62718=CARTESIAN_POINT('Ctrl Pts',(0.0652379087403971,2.30842143506323,
3.54772203423278));
#62719=CARTESIAN_POINT('Ctrl Pts',(-1.90374559216213,1.30721774273047,3.65883368471823));
#62720=CARTESIAN_POINT('Ctrl Pts',(-2.13096254074055,-0.889979863001003,
3.76994533520366));
#62721=CARTESIAN_POINT('Ctrl Pts',(-0.408528604769679,-2.27292100295502,
3.8810569856891));
#62722=CARTESIAN_POINT('Ctrl Pts',(1.6876745272456,-1.57633124585981,3.99216863617453));
#62723=CARTESIAN_POINT('Ctrl Pts',(2.23979789625721,0.562468568463683,4.10328028665997));
#62724=CARTESIAN_POINT('Ctrl Pts',(0.742695215461042,2.18665711155622,4.21439193714541));
#62725=CARTESIAN_POINT('Ctrl Pts',(-1.43391090854028,1.81023893808443,4.32550358763085));
#62726=CARTESIAN_POINT('Ctrl Pts',(-2.29860956455329,-0.222395090620434,
4.43661523811628));
#62727=CARTESIAN_POINT('Ctrl Pts',(-1.06027445761331,-2.05155638019547,
4.54772688860172));
#62728=CARTESIAN_POINT('Ctrl Pts',(1.14812229735204,-2.00371672072451,4.65883853908716));
#62729=CARTESIAN_POINT('Ctrl Pts',(2.30608404475241,-0.122645363248325,
4.76995018957259));
#62730=CARTESIAN_POINT('Ctrl Pts',(1.35417351061808,1.87063615108022,4.88106184005803));
#62731=CARTESIAN_POINT('Ctrl Pts',(-0.83669150175529,2.1524434574405,4.99217349054346));
#62732=CARTESIAN_POINT('Ctrl Pts',(-2.26205440167697,0.464946653328952,
5.10328514102891));
#62733=CARTESIAN_POINT('Ctrl Pts',(-1.61782842764492,-1.64793709991974,
5.21439679151433));
#62734=CARTESIAN_POINT('Ctrl Pts',(0.506574022840452,-2.25309748257175,
5.32550844199978));
#62735=CARTESIAN_POINT('Ctrl Pts',(2.1675039941815,-0.796863816342033,5.43662009248521));
#62736=CARTESIAN_POINT('Ctrl Pts',(1.84535073495005,1.38843299139974,5.54773174297065));
#62737=CARTESIAN_POINT('Ctrl Pts',(-0.1651427104253,2.30343078727826,5.65884339345609));
#62738=CARTESIAN_POINT('Ctrl Pts',(-2.024544512798,1.1109838082922,5.76995504394152));
#62739=CARTESIAN_POINT('Ctrl Pts',(-2.03165894515671,-1.09791959503082,
5.88106669442697));
#62740=CARTESIAN_POINT('Ctrl Pts',(-0.179976902307884,-2.30231922661119,
5.99217834491239));
#62741=CARTESIAN_POINT('Ctrl Pts',(1.83636881720094,-1.40029106752845,6.10328999539785));
#62742=CARTESIAN_POINT('Ctrl Pts',(2.17259204728728,0.782885242326115,6.21440164588326));
#62743=CARTESIAN_POINT('Ctrl Pts',(0.521076907609949,2.24978762618687,6.32551329636872));
#62744=CARTESIAN_POINT('Ctrl Pts',(-1.60717962682088,1.6583242004264,6.43662494685413));
#62745=CARTESIAN_POINT('Ctrl Pts',(-2.26500243885858,-0.450365916286509,
6.5477365973396));
#62746=CARTESIAN_POINT('Ctrl Pts',(-0.850539171717745,-2.14700922773088,
6.65884824782501));
#62747=CARTESIAN_POINT('Ctrl Pts',(1.34209565723166,-1.87932029027199,6.76995989831046));
#62748=CARTESIAN_POINT('Ctrl Pts',(2.30682622449346,0.107788109627418,6.8810715487959));
#62749=CARTESIAN_POINT('Ctrl Pts',(1.16100547839306,1.99627948587589,6.99218319928133));
#62750=CARTESIAN_POINT('Ctrl Pts',(-1.04703729866327,2.05834360634882,7.10329484976677));
#62751=CARTESIAN_POINT('Ctrl Pts',(-2.29712931099768,0.237197038645086,
7.21440650025221));
#62752=CARTESIAN_POINT('Ctrl Pts',(-1.44554186745893,-1.80096480143545,
7.32551815073763));
#62753=CARTESIAN_POINT('Ctrl Pts',(0.72859438989827,-2.19139583863915,7.43662980122308));
#62754=CARTESIAN_POINT('Ctrl Pts',(2.23612826941383,-0.576884623911715,
7.5477414517085));
#62755=CARTESIAN_POINT('Ctrl Pts',(1.6977934979946,1.56542733614398,7.65885310219396));
#62756=CARTESIAN_POINT('Ctrl Pts',(-0.393879040694563,2.27550539615811,
7.76996475267938));
#62757=CARTESIAN_POINT('Ctrl Pts',(-2.12518549811472,0.903688057410859,
7.88107640316484));
#62758=CARTESIAN_POINT('Ctrl Pts',(-1.91212657747833,-1.29492758803799,
7.99218805365025));
#62759=CARTESIAN_POINT('Ctrl Pts',(0.0503667898133586,-2.30879377455661,
8.1032997041357));
#62760=CARTESIAN_POINT('Ctrl Pts',(1.96677879493939,-1.21030850518371,8.21441135462113));
#62761=CARTESIAN_POINT('Ctrl Pts',(2.08375418707704,0.995506903268707,8.32552300510658));
#62762=CARTESIAN_POINT('Ctrl Pts',(0.294270353677539,2.29051751091564,8.436634655592));
#62763=CARTESIAN_POINT('Ctrl Pts',(-1.76444601777748,1.4898978999011,8.54774630607746));
#62764=CARTESIAN_POINT('Ctrl Pts',(-2.2088431932234,-0.673852547682493,
8.65885795656288));
#62765=CARTESIAN_POINT('Ctrl Pts',(-0.632335256349382,-2.2210847899434,
8.76996960704833));
#62766=CARTESIAN_POINT('Ctrl Pts',(1.52270606837662,-1.73621188252162,8.88108125753376));
#62767=CARTESIAN_POINT('Ctrl Pts',(2.28459985995541,0.337148347205355,8.99219290801919));
#62768=CARTESIAN_POINT('Ctrl Pts',(0.956277562497704,2.10204633917866,9.10330455850463));
#62769=CARTESIAN_POINT('Ctrl Pts',(-1.2469579560031,1.94374924182257,9.21441620899007));
#62770=CARTESIAN_POINT('Ctrl Pts',(-2.30933226540692,0.00708579792413808,
9.32552785947551));
#62771=CARTESIAN_POINT('Ctrl Pts',(-1.25886228368054,-1.93606087509586,
9.43663950996094));
#62772=CARTESIAN_POINT('Ctrl Pts',(0.943360139257667,-2.10787462610152,
9.54775116044639));
#62773=CARTESIAN_POINT('Ctrl Pts',(2.28248823506631,-0.351162152961091,
9.65886281093181));
#62774=CARTESIAN_POINT('Ctrl Pts',(1.53333110744206,1.72683627576032,9.76997446141726));
#62775=CARTESIAN_POINT('Ctrl Pts',(-0.618692454411617,2.22492101746939,
9.88108611190268));
#62776=CARTESIAN_POINT('Ctrl Pts',(-2.20466868021367,0.687398848825245,
9.99219776238814));
#62777=CARTESIAN_POINT('Ctrl Pts',(-1.7735514221838,-1.47905058047522,10.1033094128735));
#62778=CARTESIAN_POINT('Ctrl Pts',(0.280201048116106,-2.29226437530741,
10.214421063359));
#62779=CARTESIAN_POINT('Ctrl Pts',(2.07762111854432,-1.0083052618152,10.3255327138444));
#62780=CARTESIAN_POINT('Ctrl Pts',(1.97414006873683,1.19827380577986,10.4366443643299));
#62781=CARTESIAN_POINT('Ctrl Pts',(0.0645886152005097,2.30833217918201,
10.5477560148153));
#62782=CARTESIAN_POINT('Ctrl Pts',(-1.90424854748374,1.30684465150768,10.6588676653008));
#62783=CARTESIAN_POINT('Ctrl Pts',(-2.13049227679005,-0.891025387309722,
10.7699793157862));
#62784=CARTESIAN_POINT('Ctrl Pts',(-0.408214485225542,-2.27228942196666,
10.8810909662716));
#62785=CARTESIAN_POINT('Ctrl Pts',(1.68888461736298,-1.5772814986318,10.9922026167571));
#62786=CARTESIAN_POINT('Ctrl Pts',(2.23817187934597,0.566161966084782,11.1033142672425));
#62787=CARTESIAN_POINT('Ctrl Pts',(1.24300218570944,1.64165746435707,11.1773887008995));
#62788=CARTESIAN_POINT('Ctrl Pts',(0.627850911123727,1.850383536838,11.2144259177279));
#62789=CARTESIAN_POINT('Ctrl Pts',(1.05793541951254,-1.4823699524473,-0.153382721514713));
#62790=CARTESIAN_POINT('Ctrl Pts',(1.55074231467859,-1.13066431478549,-0.116345504686234));
#62791=CARTESIAN_POINT('Ctrl Pts',(2.14955001436596,0.0967274517879858,
-0.0422710710292769));
#62792=CARTESIAN_POINT('Ctrl Pts',(1.08290436090784,1.86174541551099,0.0688405794561606));
#62793=CARTESIAN_POINT('Ctrl Pts',(-0.975409307071879,1.91793784975909,
0.179952229941597));
#62794=CARTESIAN_POINT('Ctrl Pts',(-2.14083151712633,0.22213180716797,0.291063880427034));
#62795=CARTESIAN_POINT('Ctrl Pts',(-1.34782279118508,-1.67833716661673,
0.402175530912471));
#62796=CARTESIAN_POINT('Ctrl Pts',(0.678460972679723,-2.04251926348523,
0.513287181397908));
#62797=CARTESIAN_POINT('Ctrl Pts',(2.08394142450739,-0.538362390807298,
0.624398831883346));
#62798=CARTESIAN_POINT('Ctrl Pts',(1.58282747515632,1.45855746470163,0.735510482368781));
#62799=CARTESIAN_POINT('Ctrl Pts',(-0.366459012269607,2.12091168831785,
0.84662213285422));
#62800=CARTESIAN_POINT('Ctrl Pts',(-1.98045646054783,0.842867780077688,
0.957733783339656));
#62801=CARTESIAN_POINT('Ctrl Pts',(-1.78250862301028,-1.20635899339281,
1.06884543382509));
#62802=CARTESIAN_POINT('Ctrl Pts',(0.0462869228141735,-2.15185334908375,
1.17995708431053));
#62803=CARTESIAN_POINT('Ctrl Pts',(1.83273239545565,-1.12859176615955,1.29106873479597));
#62804=CARTESIAN_POINT('Ctrl Pts',(1.94238315681312,0.927240382098824,1.4021803852814));
#62805=CARTESIAN_POINT('Ctrl Pts',(0.274916856192995,2.13472355144377,1.51329203576684));
#62806=CARTESIAN_POINT('Ctrl Pts',(-1.64407495706399,1.38911602796551,1.62440368625228));
#62807=CARTESIAN_POINT('Ctrl Pts',(-2.0588770445336,-0.62741605808422,1.73551533673771));
#62808=CARTESIAN_POINT('Ctrl Pts',(-0.589980335104445,-2.06991507018771,
1.84662698722315));
#62809=CARTESIAN_POINT('Ctrl Pts',(1.41869855984326,-1.61861665507704,1.95773863770859));
#62810=CARTESIAN_POINT('Ctrl Pts',(2.1293880179812,0.313579489369987,2.06885028819403));
#62811=CARTESIAN_POINT('Ctrl Pts',(0.891867138635642,1.95887681727571,2.17996193867946));
#62812=CARTESIAN_POINT('Ctrl Pts',(-1.16163690001897,1.8119671998123,2.2910735891649));
#62813=CARTESIAN_POINT('Ctrl Pts',(-2.1523412125303,0.0072605002547781,
2.40218523965033));
#62814=CARTESIAN_POINT('Ctrl Pts',(-1.1738349588193,-1.80408893734178,2.51329689013577));
#62815=CARTESIAN_POINT('Ctrl Pts',(0.878631217069615,-1.96484925501419,
2.62440854062121));
#62816=CARTESIAN_POINT('Ctrl Pts',(2.12722398078527,-0.327938323711113,
2.73552019110664));
#62817=CARTESIAN_POINT('Ctrl Pts',(1.42958632662274,1.60900849678758,2.84663184159209));
#62818=CARTESIAN_POINT('Ctrl Pts',(-0.57600216794938,2.07384833374845,2.95774349207752));
#62819=CARTESIAN_POINT('Ctrl Pts',(-2.05459728996263,0.641291965189069,
3.06885514256296));
#62820=CARTESIAN_POINT('Ctrl Pts',(-1.65340928710165,-1.37799243024573,
3.17996679304839));
#62821=CARTESIAN_POINT('Ctrl Pts',(0.260508675794864,-2.13653004623031,
3.29107844353384));
#62822=CARTESIAN_POINT('Ctrl Pts',(1.93608318568785,-0.940322979965331,
3.40219009401926));
#62823=CARTESIAN_POINT('Ctrl Pts',(1.84030497427301,1.11620025542831,3.51330174450471));
#62824=CARTESIAN_POINT('Ctrl Pts',(0.0608030219043116,2.15149445760286,
3.62441339499014));
#62825=CARTESIAN_POINT('Ctrl Pts',(-1.77432856410404,1.21835280406139,3.73552504547559));
#62826=CARTESIAN_POINT('Ctrl Pts',(-1.98609925645444,-0.829478843655077,
3.84663669596101));
#62827=CARTESIAN_POINT('Ctrl Pts',(-0.380756743800589,-2.11840735237885,
3.95774834644646));
#62828=CARTESIAN_POINT('Ctrl Pts',(1.57294605588646,-1.4691719143219,4.06885999693188));
#62829=CARTESIAN_POINT('Ctrl Pts',(2.08753596148093,0.524231836199493,4.17997164741733));
#62830=CARTESIAN_POINT('Ctrl Pts',(0.692206637610257,2.03800769856489,4.29108329790276));
#62831=CARTESIAN_POINT('Ctrl Pts',(-1.33643334165982,1.68717851215016,4.4021949483882));
#62832=CARTESIAN_POINT('Ctrl Pts',(-2.1423496001257,-0.207276625316418,
4.51330659887364));
#62833=CARTESIAN_POINT('Ctrl Pts',(-0.988196775702872,-1.91209114350017,
4.62441824935908));
#62834=CARTESIAN_POINT('Ctrl Pts',(1.07007270071357,-1.86750363419964,4.73552989984451));
#62835=CARTESIAN_POINT('Ctrl Pts',(2.1493159635798,-0.11430790551128,4.84664155032995));
#62836=CARTESIAN_POINT('Ctrl Pts',(1.26211650891535,1.74346990983058,4.95775320081538));
#62837=CARTESIAN_POINT('Ctrl Pts',(-0.779813036479037,2.00611989589323,
5.06886485130082));
#62838=CARTESIAN_POINT('Ctrl Pts',(-2.1082794649543,0.433339481484583,5.17997650178626));
#62839=CARTESIAN_POINT('Ctrl Pts',(-1.50784810891129,-1.53590998727594,
5.29108815227169));
#62840=CARTESIAN_POINT('Ctrl Pts',(0.472137013611209,-2.09993143910453,
5.40219980275713));
#62841=CARTESIAN_POINT('Ctrl Pts',(2.02015661416081,-0.742692845544967,
5.51331145324257));
#62842=CARTESIAN_POINT('Ctrl Pts',(1.71990340163759,1.29404702294652,5.62442310372801));
#62843=CARTESIAN_POINT('Ctrl Pts',(-0.153916274037652,2.14684307510999,
5.73553475421344));
#62844=CARTESIAN_POINT('Ctrl Pts',(-1.88691554856225,1.03545889399597,5.84664640469888));
#62845=CARTESIAN_POINT('Ctrl Pts',(-1.89354634030427,-1.02328278871562,
5.95775805518432));
#62846=CARTESIAN_POINT('Ctrl Pts',(-0.167742034418123,-2.1458070785722,
6.06886970566975));
#62847=CARTESIAN_POINT('Ctrl Pts',(1.71153207655705,-1.30509898455162,6.1799813561552));
#62848=CARTESIAN_POINT('Ctrl Pts',(2.02489878034016,0.729664537947597,6.29109300664062));
#62849=CARTESIAN_POINT('Ctrl Pts',(0.485653989206222,2.09684658745684,6.40220465712607));
#62850=CARTESIAN_POINT('Ctrl Pts',(-1.49792321581985,1.54559097049293,6.5133163076115));
#62851=CARTESIAN_POINT('Ctrl Pts',(-2.11102709394471,-0.41974994603061,
6.62442795809694));
#62852=CARTESIAN_POINT('Ctrl Pts',(-0.79271933890819,-2.0010550862688,6.73553960858237));
#62853=CARTESIAN_POINT('Ctrl Pts',(1.25085971055702,-1.7515636994031,6.84665125906781));
#62854=CARTESIAN_POINT('Ctrl Pts',(2.15000768978506,0.100460651134341,6.95776290955325));
#62855=CARTESIAN_POINT('Ctrl Pts',(1.08208008038219,1.86057198414926,7.06887456003868));
#62856=CARTESIAN_POINT('Ctrl Pts',(-0.975859481618359,1.91841697258389,
7.17998621052413));
#62857=CARTESIAN_POINT('Ctrl Pts',(-2.14096997451993,0.221072333783236,
7.29109786100956));
#62858=CARTESIAN_POINT('Ctrl Pts',(-1.34727362553083,-1.67853483327237,
7.402209511495));
#62859=CARTESIAN_POINT('Ctrl Pts',(0.679064389152043,-2.04242428597833,
7.51332116198043));
#62860=CARTESIAN_POINT('Ctrl Pts',(2.08411579664662,-0.537667885148679,
7.62443281246587));
#62861=CARTESIAN_POINT('Ctrl Pts',(1.58237713686343,1.4590092546951,7.73554446295131));
#62862=CARTESIAN_POINT('Ctrl Pts',(-0.367103060190181,2.1208160579853,7.84665611343674));
#62863=CARTESIAN_POINT('Ctrl Pts',(-1.98071493840836,0.842255152109201,
7.95776776392219));
#62864=CARTESIAN_POINT('Ctrl Pts',(-1.78213980826558,-1.20689813668469,
8.0688794144076));
#62865=CARTESIAN_POINT('Ctrl Pts',(0.0469428447876819,-2.15184148537872,
8.17999106489306));
#62866=CARTESIAN_POINT('Ctrl Pts',(1.83307675642296,-1.12803147698245,8.29110271537848));
#62867=CARTESIAN_POINT('Ctrl Pts',(1.94210013665906,0.927832133403047,8.40221436586394));
#62868=CARTESIAN_POINT('Ctrl Pts',(0.274265792786954,2.13480764600607,8.51332601634936));
#62869=CARTESIAN_POINT('Ctrl Pts',(-1.64449860425235,1.38861432550488,8.6244376668348));
#62870=CARTESIAN_POINT('Ctrl Pts',(-2.05868556570727,-0.628043908949741,
8.73554931732024));
#62871=CARTESIAN_POINT('Ctrl Pts',(-0.589348971863656,-2.07009497609277,
8.84666096780567));
#62872=CARTESIAN_POINT('Ctrl Pts',(1.41919218774748,-1.61818383148359,8.95777261829112));
#62873=CARTESIAN_POINT('Ctrl Pts',(2.12929227820989,0.314228931244718,9.06888426877654));
#62874=CARTESIAN_POINT('Ctrl Pts',(0.891269611515884,1.95914878439144,9.179995919262));
#62875=CARTESIAN_POINT('Ctrl Pts',(-1.16218949038264,1.81161275719849,9.29110756974741));
#62876=CARTESIAN_POINT('Ctrl Pts',(-2.15234336950711,0.00660410388236847,
9.40221922023287));
#62877=CARTESIAN_POINT('Ctrl Pts',(-1.17328455934639,-1.80444704726821,
9.51333087071829));
#62878=CARTESIAN_POINT('Ctrl Pts',(0.879230317440182,-1.96458086313641,
9.62444252120374));
#62879=CARTESIAN_POINT('Ctrl Pts',(2.12732420202743,-0.327290075520782,
9.73555417168917));
#62880=CARTESIAN_POINT('Ctrl Pts',(1.42909493440969,1.60944558045319,9.8466658221746));
#62881=CARTESIAN_POINT('Ctrl Pts',(-0.576633610487541,2.07367041606005,
9.95777747266004));
#62882=CARTESIAN_POINT('Ctrl Pts',(-2.05479483697499,0.640669329675303,
10.0688891231455));
#62883=CARTESIAN_POINT('Ctrl Pts',(-1.65298502134104,-1.37850440914814,
10.1800007736309));
#62884=CARTESIAN_POINT('Ctrl Pts',(0.26115292159373,-2.13643575818697,10.2911124241164));
#62885=CARTESIAN_POINT('Ctrl Pts',(1.93638399542254,-0.939760456828254,
10.4022240746018));
#62886=CARTESIAN_POINT('Ctrl Pts',(1.83993760927049,1.11681489898982,10.5133357250872));
#62887=CARTESIAN_POINT('Ctrl Pts',(0.0601978674766102,2.15141126935532,
10.6244473755726));
#62888=CARTESIAN_POINT('Ctrl Pts',(-1.77479732841649,1.21800507565884,10.7355590260581));
#62889=CARTESIAN_POINT('Ctrl Pts',(-1.98566096114678,-0.830453293000129,
10.8466706765435));
#62890=CARTESIAN_POINT('Ctrl Pts',(-0.380463978169507,-2.11781870639967,
10.957782327029));
#62891=CARTESIAN_POINT('Ctrl Pts',(1.57407388382168,-1.47005756870945,11.0688939775144));
#62892=CARTESIAN_POINT('Ctrl Pts',(2.08602048154327,0.527674155869038,11.1800056279999));
#62893=CARTESIAN_POINT('Ctrl Pts',(1.15850263419028,1.53005724266717,11.2540800616568));
#62894=CARTESIAN_POINT('Ctrl Pts',(0.585169473375027,1.72459407258861,11.2911172784853));
#62895=CARTESIAN_POINT('Ctrl Pts',(0.980771099081375,-1.37424797458507,
-0.0766913607573581));
#62896=CARTESIAN_POINT('Ctrl Pts',(1.43763335295088,-1.04819525110066,-0.0396541439288791));
#62897=CARTESIAN_POINT('Ctrl Pts',(1.99276486185844,0.089672287600667,0.0344202897280782));
#62898=CARTESIAN_POINT('Ctrl Pts',(1.00391884103562,1.72595232535247,0.145531940213516));
#62899=CARTESIAN_POINT('Ctrl Pts',(-0.904264325124765,1.77804616253862,
0.256643590698952));
#62900=CARTESIAN_POINT('Ctrl Pts',(-1.98468227953599,0.20592982580867,0.36775524118439));
#62901=CARTESIAN_POINT('Ctrl Pts',(-1.24951449388714,-1.55592161598129,
0.478866891669827));
#62902=CARTESIAN_POINT('Ctrl Pts',(0.628974984281669,-1.89354078329874,
0.589978542155263));
#62903=CARTESIAN_POINT('Ctrl Pts',(1.93194167019859,-0.499094995779056,
0.7010901926407));
#62904=CARTESIAN_POINT('Ctrl Pts',(1.46737826698393,1.35217233617898,0.812201843126137));
#62905=CARTESIAN_POINT('Ctrl Pts',(-0.339730007714042,1.96621537500318,
0.923313493611574));
#62906=CARTESIAN_POINT('Ctrl Pts',(-1.8360047538528,0.7813901905543,1.03442514409701));
#62907=CARTESIAN_POINT('Ctrl Pts',(-1.65249495296916,-1.11836886639236,
1.14553679458245));
#62908=CARTESIAN_POINT('Ctrl Pts',(0.0429108198140191,-1.99490019458391,
1.25664844506789));
#62909=CARTESIAN_POINT('Ctrl Pts',(1.69905547414348,-1.04627387125433,1.36776009555332));
#62910=CARTESIAN_POINT('Ctrl Pts',(1.80070846330345,0.859608773740392,1.47887174603876));
#62911=CARTESIAN_POINT('Ctrl Pts',(0.254864807653961,1.97901982027321,1.5899833965242));
#62912=CARTESIAN_POINT('Ctrl Pts',(-1.52415844376849,1.28779586009797,1.70109504700963));
#62913=CARTESIAN_POINT('Ctrl Pts',(-1.90870545082139,-0.581653213909888,
1.81220669749507));
#62914=CARTESIAN_POINT('Ctrl Pts',(-0.546947999872595,-1.91893837842057,
1.92331834798051));
#62915=CARTESIAN_POINT('Ctrl Pts',(1.31522068373867,-1.50055703449532,2.03442999846594));
#62916=CARTESIAN_POINT('Ctrl Pts',(1.97407345311151,0.290707442785592,2.14554164895138));
#62917=CARTESIAN_POINT('Ctrl Pts',(0.826815604866742,1.81599909938712,2.25665329943681));
#62918=CARTESIAN_POINT('Ctrl Pts',(-1.07690873956185,1.67980486264285,2.36776494992226));
#62919=CARTESIAN_POINT('Ctrl Pts',(-1.99535247395734,0.00673092958549589,
2.47887660040769));
#62920=CARTESIAN_POINT('Ctrl Pts',(-1.0882170891223,-1.67250122954812,2.58998825089313));
#62921=CARTESIAN_POINT('Ctrl Pts',(0.814545092789914,-1.82153591592328,
2.70109990137857));
#62922=CARTESIAN_POINT('Ctrl Pts',(1.97206725774273,-0.304018963960226,
2.812211551864));
#62923=CARTESIAN_POINT('Ctrl Pts',(1.325314312134,1.49164968174781,2.92332320234944));
#62924=CARTESIAN_POINT('Ctrl Pts',(-0.533989380555266,1.92258475527334,
3.03443485283487));
#62925=CARTESIAN_POINT('Ctrl Pts',(-1.90473785552499,0.594517031881129,
3.14554650332031));
#62926=CARTESIAN_POINT('Ctrl Pts',(-1.53281194091147,-1.27748360193918,
3.25665815380575));
#62927=CARTESIAN_POINT('Ctrl Pts',(0.241507539654265,-1.98069455187271,
3.36776980429119));
#62928=CARTESIAN_POINT('Ctrl Pts',(1.79486800320472,-0.871737145332536,
3.47888145477662));
#62929=CARTESIAN_POINT('Ctrl Pts',(1.70607571972046,1.03478617987453,3.58999310526206));
#62930=CARTESIAN_POINT('Ctrl Pts',(0.0563681350682242,1.99456748014249,
3.7011047557475));
#62931=CARTESIAN_POINT('Ctrl Pts',(-1.64491153604594,1.1294878653923,3.81221640623293));
#62932=CARTESIAN_POINT('Ctrl Pts',(-1.84123597216834,-0.768977824309152,
3.92332805671837));
#62933=CARTESIAN_POINT('Ctrl Pts',(-0.352984882831497,-1.96389370180267,
4.03443970720381));
#62934=CARTESIAN_POINT('Ctrl Pts',(1.45821758452731,-1.36201258278399,4.14555135768924));
#62935=CARTESIAN_POINT('Ctrl Pts',(1.93527402670466,0.485995103935303,4.25666300817468));
#62936=CARTESIAN_POINT('Ctrl Pts',(0.641718059759468,1.88935828557357,4.36777465866012));
#62937=CARTESIAN_POINT('Ctrl Pts',(-1.23895577477937,1.56411808621589,4.47888630914555));
#62938=CARTESIAN_POINT('Ctrl Pts',(-1.98608963569812,-0.1921581600124,4.58999795963099));
#62939=CARTESIAN_POINT('Ctrl Pts',(-0.916119093792434,-1.77262590680487,
4.70110961011643));
#62940=CARTESIAN_POINT('Ctrl Pts',(0.992023104075105,-1.73129054767478,
4.81222126060186));
#62941=CARTESIAN_POINT('Ctrl Pts',(1.99254788240719,-0.105970447774237,
4.9233329110873));
#62942=CARTESIAN_POINT('Ctrl Pts',(1.17005950721263,1.61630366858093,5.03444456157274));
#62943=CARTESIAN_POINT('Ctrl Pts',(-0.722934571202785,1.85979633434597,
5.14555621205818));
#62944=CARTESIAN_POINT('Ctrl Pts',(-1.95450452823164,0.401732309640217,
5.25666786254361));
#62945=CARTESIAN_POINT('Ctrl Pts',(-1.39786779017765,-1.42388287463214,
5.36777951302905));
#62946=CARTESIAN_POINT('Ctrl Pts',(0.437700004381964,-1.9467653956373,5.47889116351449));
#62947=CARTESIAN_POINT('Ctrl Pts',(1.87280923414012,-0.688521874747905,
5.59000281399993));
#62948=CARTESIAN_POINT('Ctrl Pts',(1.59445606832513,1.19966105449332,5.70111446448536));
#62949=CARTESIAN_POINT('Ctrl Pts',(-0.142689837650004,1.99025536294172,
5.81222611497081));
#62950=CARTESIAN_POINT('Ctrl Pts',(-1.74928658432651,0.959933979699734,
5.92333776545623));
#62951=CARTESIAN_POINT('Ctrl Pts',(-1.75543373545183,-0.948645982400418,
6.03444941594168));
#62952=CARTESIAN_POINT('Ctrl Pts',(-0.155507166528361,-1.98929493053321,
6.1455610664271));
#62953=CARTESIAN_POINT('Ctrl Pts',(1.58669533591315,-1.20990690157479,6.25667271691256));
#62954=CARTESIAN_POINT('Ctrl Pts',(1.87720551339304,0.676443833569079,6.36778436739797));
#62955=CARTESIAN_POINT('Ctrl Pts',(0.450231070802491,1.94390554872681,6.47889601788343));
#62956=CARTESIAN_POINT('Ctrl Pts',(-1.38866680481881,1.43285774055946,6.59000766836885));
#62957=CARTESIAN_POINT('Ctrl Pts',(-1.95705174903083,-0.38913397577471,
6.7011193188543));
#62958=CARTESIAN_POINT('Ctrl Pts',(-0.734899506098636,-1.85510094480672,
6.81223096933973));
#62959=CARTESIAN_POINT('Ctrl Pts',(1.15962376388238,-1.62380710853421,6.92334261982516));
#62960=CARTESIAN_POINT('Ctrl Pts',(1.99318915507666,0.0931331926412601,
7.03445427031061));
#62961=CARTESIAN_POINT('Ctrl Pts',(1.00315468237132,1.72486448242263,7.14556592079604));
#62962=CARTESIAN_POINT('Ctrl Pts',(-0.904681664573454,1.77849033881895,
7.25667757128148));
#62963=CARTESIAN_POINT('Ctrl Pts',(-1.98481063804218,0.204947628921387,
7.36778922176691));
#62964=CARTESIAN_POINT('Ctrl Pts',(-1.24900538360275,-1.55610486510929,
7.47890087225236));
#62965=CARTESIAN_POINT('Ctrl Pts',(0.629534388405818,-1.89345273331751,
7.59001252273779));
#62966=CARTESIAN_POINT('Ctrl Pts',(1.93210332387941,-0.498451146385645,
7.70112417322323));
#62967=CARTESIAN_POINT('Ctrl Pts',(1.46696077573226,1.35259117324623,7.81223582370866));
#62968=CARTESIAN_POINT('Ctrl Pts',(-0.340327079685797,1.96612671981249,
7.9233474741941));
#62969=CARTESIAN_POINT('Ctrl Pts',(-1.836244378702,0.780822246807544,8.03445912467955));
#62970=CARTESIAN_POINT('Ctrl Pts',(-1.65215303905282,-1.11886868533138,
8.14557077516496));
#62971=CARTESIAN_POINT('Ctrl Pts',(0.0435188997620014,-1.99488919620082,
8.25668242565042));
#62972=CARTESIAN_POINT('Ctrl Pts',(1.69937471790653,-1.04575444878119,8.36779407613584));
#62973=CARTESIAN_POINT('Ctrl Pts',(1.80044608624107,0.860157363537389,8.47890572662129));
#62974=CARTESIAN_POINT('Ctrl Pts',(0.254261231896373,1.97909778109651,8.59001737710672));
#62975=CARTESIAN_POINT('Ctrl Pts',(-1.52455119072723,1.28733075110866,8.70112902759215));
#62976=CARTESIAN_POINT('Ctrl Pts',(-1.90852793819114,-0.58223527021699,
8.8122406780776));
#62977=CARTESIAN_POINT('Ctrl Pts',(-0.546362687377931,-1.91910516224214,
8.92335232856302));
#62978=CARTESIAN_POINT('Ctrl Pts',(1.31567830711834,-1.50015578044556,9.03446397904849));
#62979=CARTESIAN_POINT('Ctrl Pts',(1.97398469646436,0.291309515284085,9.14557562953389));
#62980=CARTESIAN_POINT('Ctrl Pts',(0.826261660534066,1.81625122960423,9.25668728001935));
#62981=CARTESIAN_POINT('Ctrl Pts',(-1.07742102476217,1.67947627257441,9.36779893050478));
#62982=CARTESIAN_POINT('Ctrl Pts',(-1.99535447360731,0.00612240984059651,
9.47891058099021));
#62983=CARTESIAN_POINT('Ctrl Pts',(-1.08770683501224,-1.67283321944057,
9.59002223147566));
#62984=CARTESIAN_POINT('Ctrl Pts',(0.815100495622697,-1.82128710017129,
9.70113388196108));
#62985=CARTESIAN_POINT('Ctrl Pts',(1.97216016898856,-0.303417998080474,
9.81224553244654));
#62986=CARTESIAN_POINT('Ctrl Pts',(1.32485876137733,1.49205488514605,9.92335718293196));
#62987=CARTESIAN_POINT('Ctrl Pts',(-0.534574766563464,1.9224198146507,10.0344688334174));
#62988=CARTESIAN_POINT('Ctrl Pts',(-1.90492099373632,0.593939810525364,
10.1455804839028));
#62989=CARTESIAN_POINT('Ctrl Pts',(-1.53241862049827,-1.27795823782107,
10.2566921343883));
#62990=CARTESIAN_POINT('Ctrl Pts',(0.242104795071353,-1.98060714106653,
10.3678037848737));
#62991=CARTESIAN_POINT('Ctrl Pts',(1.79514687230076,-0.871215651841315,
10.4789154353591));
#62992=CARTESIAN_POINT('Ctrl Pts',(1.70573514980415,1.03535599219979,10.5900270858446));
#62993=CARTESIAN_POINT('Ctrl Pts',(0.055807119752709,1.99449035952863,10.70113873633));
#62994=CARTESIAN_POINT('Ctrl Pts',(-1.64534610934924,1.12916549981001,10.8122503868155));
#62995=CARTESIAN_POINT('Ctrl Pts',(-1.84082964550351,-0.769881198690536,
10.9233620373009));
#62996=CARTESIAN_POINT('Ctrl Pts',(-0.352713471113472,-1.96334799083268,
11.0344736877863));
#62997=CARTESIAN_POINT('Ctrl Pts',(1.45926315028039,-1.36283363878709,11.1455853382718));
#62998=CARTESIAN_POINT('Ctrl Pts',(1.93386908374058,0.489186345653294,11.2566969887572));
#62999=CARTESIAN_POINT('Ctrl Pts',(1.07400308267113,1.41845702097726,11.3307714224142));
#63000=CARTESIAN_POINT('Ctrl Pts',(0.542488035626326,1.59880460833922,11.3678086392426));
#63001=CARTESIAN_POINT('Ctrl Pts',(0.903606778650208,-1.26612599672284,
-2.77555756156289E-15));
#63002=CARTESIAN_POINT('Ctrl Pts',(1.32452439122316,-0.965726187415828,
0.0370372168284762));
#63003=CARTESIAN_POINT('Ctrl Pts',(1.83597970935092,0.0826171234133487,
0.111111650485434));
#63004=CARTESIAN_POINT('Ctrl Pts',(0.924933321163406,1.59015923519395,0.222223300970871));
#63005=CARTESIAN_POINT('Ctrl Pts',(-0.833119343177651,1.63815447531815,
0.333334951456308));
#63006=CARTESIAN_POINT('Ctrl Pts',(-1.82853304194564,0.18972784444937,0.444446601941745));
#63007=CARTESIAN_POINT('Ctrl Pts',(-1.15120619658919,-1.43350606534586,
0.555558252427182));
#63008=CARTESIAN_POINT('Ctrl Pts',(0.579488995883613,-1.74456230311225,
0.666669902912619));
#63009=CARTESIAN_POINT('Ctrl Pts',(1.77994191588978,-0.459827600750814,
0.777781553398056));
#63010=CARTESIAN_POINT('Ctrl Pts',(1.35192905881154,1.24578720765632,0.888893203883492));
#63011=CARTESIAN_POINT('Ctrl Pts',(-0.313001003158473,1.81151906168851,
1.00000485436893));
#63012=CARTESIAN_POINT('Ctrl Pts',(-1.69155304715778,0.719912601030908,
1.11111650485437));
#63013=CARTESIAN_POINT('Ctrl Pts',(-1.52248128292804,-1.03037873939191,
1.2222281553398));
#63014=CARTESIAN_POINT('Ctrl Pts',(0.0395347168138628,-1.83794704008407,
1.33333980582524));
#63015=CARTESIAN_POINT('Ctrl Pts',(1.56537855283131,-0.963955976349113,
1.44445145631068));
#63016=CARTESIAN_POINT('Ctrl Pts',(1.65903376979378,0.791977165381959,1.55556310679611));
#63017=CARTESIAN_POINT('Ctrl Pts',(0.234812759114929,1.82331608910266,1.66667475728155));
#63018=CARTESIAN_POINT('Ctrl Pts',(-1.404241930473,1.18647569223042,1.77778640776699));
#63019=CARTESIAN_POINT('Ctrl Pts',(-1.75853385710917,-0.535890369735552,
1.88889805825242));
#63020=CARTESIAN_POINT('Ctrl Pts',(-0.503915664640746,-1.76796168665343,
2.00000970873786));
#63021=CARTESIAN_POINT('Ctrl Pts',(1.21174280763407,-1.38249741391359,2.1111213592233));
#63022=CARTESIAN_POINT('Ctrl Pts',(1.81875888824183,0.267835396201195,2.22223300970874));
#63023=CARTESIAN_POINT('Ctrl Pts',(0.761764071097843,1.67312138149853,2.33334466019417));
#63024=CARTESIAN_POINT('Ctrl Pts',(-0.992180579104728,1.54764252547341,
2.44445631067961));
#63025=CARTESIAN_POINT('Ctrl Pts',(-1.83836373538439,0.00620135891621234,
2.55556796116504));
#63026=CARTESIAN_POINT('Ctrl Pts',(-1.0025992194253,-1.54091352175446,2.66667961165049));
#63027=CARTESIAN_POINT('Ctrl Pts',(0.750458968510211,-1.67822257683237,
2.77779126213592));
#63028=CARTESIAN_POINT('Ctrl Pts',(1.81691053470019,-0.280099604209337,
2.88890291262136));
#63029=CARTESIAN_POINT('Ctrl Pts',(1.22104229764526,1.37429086670804,3.0000145631068));
#63030=CARTESIAN_POINT('Ctrl Pts',(-0.491976593161155,1.77132117679823,
3.11112621359223));
#63031=CARTESIAN_POINT('Ctrl Pts',(-1.75487842108734,0.547742098573187,
3.22223786407767));
#63032=CARTESIAN_POINT('Ctrl Pts',(-1.41221459472129,-1.17697477363263,
3.3333495145631));
#63033=CARTESIAN_POINT('Ctrl Pts',(0.222506403513669,-1.8248590575151,3.44446116504855));
#63034=CARTESIAN_POINT('Ctrl Pts',(1.65365282072159,-0.803151310699741,
3.55557281553397));
#63035=CARTESIAN_POINT('Ctrl Pts',(1.57184646516792,0.953372104320743,3.66668446601942));
#63036=CARTESIAN_POINT('Ctrl Pts',(0.0519332482321354,1.83764050268212,
3.77779611650485));
#63037=CARTESIAN_POINT('Ctrl Pts',(-1.51549450798785,1.04062292672322,3.88890776699029));
#63038=CARTESIAN_POINT('Ctrl Pts',(-1.69637268788223,-0.708476804963227,
4.00001941747572));
#63039=CARTESIAN_POINT('Ctrl Pts',(-0.325213021862407,-1.80938005122649,
4.11113106796117));
#63040=CARTESIAN_POINT('Ctrl Pts',(1.34348911316817,-1.25485325124609,4.2222427184466));
#63041=CARTESIAN_POINT('Ctrl Pts',(1.78301209192838,0.447758371671112,4.33335436893204));
#63042=CARTESIAN_POINT('Ctrl Pts',(0.591229481908682,1.74070887258225,4.44446601941748));
#63043=CARTESIAN_POINT('Ctrl Pts',(-1.14147820789891,1.44105766028162,4.55557766990291));
#63044=CARTESIAN_POINT('Ctrl Pts',(-1.82982967127054,-0.177039694708382,
4.66668932038835));
#63045=CARTESIAN_POINT('Ctrl Pts',(-0.844041411881997,-1.63316067010957,
4.77780097087378));
#63046=CARTESIAN_POINT('Ctrl Pts',(0.913973507436636,-1.59507746114991,
4.88891262135923));
#63047=CARTESIAN_POINT('Ctrl Pts',(1.83577980123458,-0.0976329900371924,
5.00002427184466));
#63048=CARTESIAN_POINT('Ctrl Pts',(1.0780025055099,1.48913742733129,5.1111359223301));
#63049=CARTESIAN_POINT('Ctrl Pts',(-0.666056105926533,1.7134727727987,5.22224757281553));
#63050=CARTESIAN_POINT('Ctrl Pts',(-1.80072959150898,0.37012513779585,5.33335922330097));
#63051=CARTESIAN_POINT('Ctrl Pts',(-1.28788747144402,-1.31185576198834,
5.44447087378641));
#63052=CARTESIAN_POINT('Ctrl Pts',(0.403262995152723,-1.79359935217008,
5.55558252427184));
#63053=CARTESIAN_POINT('Ctrl Pts',(1.72546185411942,-0.634350903950841,
5.66669417475728));
#63054=CARTESIAN_POINT('Ctrl Pts',(1.46900873501267,1.1052750860401,5.77780582524271));
#63055=CARTESIAN_POINT('Ctrl Pts',(-0.13146340126236,1.83366765077345,5.88891747572816));
#63056=CARTESIAN_POINT('Ctrl Pts',(-1.61165762009075,0.884409065403499,
6.00002912621358));
#63057=CARTESIAN_POINT('Ctrl Pts',(-1.6173211305994,-0.87400917608522,6.11114077669903));
#63058=CARTESIAN_POINT('Ctrl Pts',(-0.143272298638598,-1.83278278249422,
6.22225242718446));
#63059=CARTESIAN_POINT('Ctrl Pts',(1.46185859526926,-1.11471481859797,6.33336407766989));
#63060=CARTESIAN_POINT('Ctrl Pts',(1.72951224644592,0.623223129190563,6.44447572815534));
#63061=CARTESIAN_POINT('Ctrl Pts',(0.414808152398764,1.79096450999678,6.55558737864077));
#63062=CARTESIAN_POINT('Ctrl Pts',(-1.27941039381778,1.320124510626,6.66669902912621));
#63063=CARTESIAN_POINT('Ctrl Pts',(-1.80307640411694,-0.358518005518811,
6.77781067961165));
#63064=CARTESIAN_POINT('Ctrl Pts',(-0.677079673289082,-1.70914680334463,
6.8889223300971));
#63065=CARTESIAN_POINT('Ctrl Pts',(1.06838781720774,-1.49605051766532,7.00003398058251));
#63066=CARTESIAN_POINT('Ctrl Pts',(1.83637062036826,0.0858057341481814,
7.11114563106797));
#63067=CARTESIAN_POINT('Ctrl Pts',(0.924229284360448,1.589156980696,7.22225728155339));
#63068=CARTESIAN_POINT('Ctrl Pts',(-0.833503847528551,1.63856370505402,
7.33336893203883));
#63069=CARTESIAN_POINT('Ctrl Pts',(-1.82865130156443,0.188822924059537,
7.44448058252428));
#63070=CARTESIAN_POINT('Ctrl Pts',(-1.15073714167466,-1.43367489694622,
7.5555922330097));
#63071=CARTESIAN_POINT('Ctrl Pts',(0.580004387659595,-1.74448118065669,
7.66670388349515));
#63072=CARTESIAN_POINT('Ctrl Pts',(1.7800908511122,-0.459234407622611,7.77781553398057));
#63073=CARTESIAN_POINT('Ctrl Pts',(1.35154441460109,1.24617309179735,7.88892718446602));
#63074=CARTESIAN_POINT('Ctrl Pts',(-0.313551099181417,1.81143738163968,
8.00003883495145));
#63075=CARTESIAN_POINT('Ctrl Pts',(-1.69177381899564,0.719389341505889,
8.11115048543689));
#63076=CARTESIAN_POINT('Ctrl Pts',(-1.52216626984007,-1.03083923397808,
8.22226213592232));
#63077=CARTESIAN_POINT('Ctrl Pts',(0.0400949547363229,-1.83793690702293,
8.33337378640777));
#63078=CARTESIAN_POINT('Ctrl Pts',(1.56567267939011,-0.963477420579929,
8.44448543689319));
#63079=CARTESIAN_POINT('Ctrl Pts',(1.65879203582308,0.792482593671729,8.55559708737864));
#63080=CARTESIAN_POINT('Ctrl Pts',(0.234256671005791,1.82338791618694,8.66670873786407));
#63081=CARTESIAN_POINT('Ctrl Pts',(-1.40460377720211,1.18604717671243,8.77782038834951));
#63082=CARTESIAN_POINT('Ctrl Pts',(-1.75837031067501,-0.536426631484242,
8.88893203883495));
#63083=CARTESIAN_POINT('Ctrl Pts',(-0.503376402892206,-1.7681153483915,
9.00004368932038));
#63084=CARTESIAN_POINT('Ctrl Pts',(1.2121644264892,-1.38212772940753,9.11115533980582));
#63085=CARTESIAN_POINT('Ctrl Pts',(1.81867711471885,0.26839009932345,9.22226699029127));
#63086=CARTESIAN_POINT('Ctrl Pts',(0.761253709552246,1.67335367481701,9.33337864077668));
#63087=CARTESIAN_POINT('Ctrl Pts',(-0.99265255914171,1.54733978795034,9.44449029126215));
#63088=CARTESIAN_POINT('Ctrl Pts',(-1.8383655777075,0.00564071579882353,
9.55560194174756));
#63089=CARTESIAN_POINT('Ctrl Pts',(-1.00212911067809,-1.54121939161292,
9.66671359223301));
#63090=CARTESIAN_POINT('Ctrl Pts',(0.750970673805211,-1.67799333720618,
9.77782524271844));
#63091=CARTESIAN_POINT('Ctrl Pts',(1.81699613594968,-0.279545920640164,
9.88893689320389));
#63092=CARTESIAN_POINT('Ctrl Pts',(1.22062258834496,1.37466418983892,10.0000485436893));
#63093=CARTESIAN_POINT('Ctrl Pts',(-0.492515922639386,1.77116921324136,
10.1111601941748));
#63094=CARTESIAN_POINT('Ctrl Pts',(-1.75504715049764,0.547210291375423,
10.2222718446602));
#63095=CARTESIAN_POINT('Ctrl Pts',(-1.4118522196555,-1.177412066494,10.3333834951456));
#63096=CARTESIAN_POINT('Ctrl Pts',(0.223056668548975,-1.82477852394609,
10.4444951456311));
#63097=CARTESIAN_POINT('Ctrl Pts',(1.65390974917898,-0.802670846854376,
10.5556067961165));
#63098=CARTESIAN_POINT('Ctrl Pts',(1.57153269033781,0.953897085409752,10.6667184466019));
#63099=CARTESIAN_POINT('Ctrl Pts',(0.0514163720288116,1.83756944970195,
10.7778300970874));
#63100=CARTESIAN_POINT('Ctrl Pts',(-1.51589489028199,1.04032592396117,10.8889417475728));
#63101=CARTESIAN_POINT('Ctrl Pts',(-1.69599832986023,-0.709309104380943,
11.0000533980583));
#63102=CARTESIAN_POINT('Ctrl Pts',(-0.324962964057439,-1.80887727526569,
11.1111650485437));
#63103=CARTESIAN_POINT('Ctrl Pts',(1.34445241673909,-1.25560970886474,11.2222766990291));
#63104=CARTESIAN_POINT('Ctrl Pts',(1.78171768593789,0.450698535437549,11.3333883495146));
#63105=CARTESIAN_POINT('Ctrl Pts',(0.989503531151977,1.30685679928735,11.4074627831715));
#63106=CARTESIAN_POINT('Ctrl Pts',(0.499806597877626,1.47301514408983,11.4445));
#63107=CARTESIAN_POINT('',(0.903606778650206,-1.26612599672284,0.));
#63108=CARTESIAN_POINT('Ctrl Pts',(0.903606778650208,-1.26612599672284,
-2.77555756156289E-15));
#63109=CARTESIAN_POINT('Ctrl Pts',(1.32452439122316,-0.965726187415828,
0.0370372168284762));
#63110=CARTESIAN_POINT('Ctrl Pts',(1.83597970935092,0.0826171234133487,
0.111111650485434));
#63111=CARTESIAN_POINT('Ctrl Pts',(0.924933321163406,1.59015923519395,0.222223300970871));
#63112=CARTESIAN_POINT('Ctrl Pts',(-0.833119343177651,1.63815447531815,
0.333334951456308));
#63113=CARTESIAN_POINT('Ctrl Pts',(-1.5310616378989,0.622578531632503,0.411241775931451));
#63114=CARTESIAN_POINT('Ctrl Pts',(-1.55772922446558,0.0543356393242454,
0.452111383578116));
#63115=CARTESIAN_POINT('Ctrl Pts',(-1.55735926886437,0.00101346774827265,
0.455943774396301));
#63116=CARTESIAN_POINT('Ctrl Pts',(0.863567639152676,1.75641488315944,2.28983498828939E-16));
#63117=CARTESIAN_POINT('Ctrl Pts',(0.902605506355985,1.73244147111074,2.48310810971475E-16));
#63118=CARTESIAN_POINT('Ctrl Pts',(0.940681517855526,1.70703362163956,1.53446104133306E-16));
#63119=CARTESIAN_POINT('Ctrl Pts',(0.977705169885396,1.68018661523996,1.12757025938492E-16));
#63120=CARTESIAN_POINT('Ctrl Pts',(1.0358643592122,1.63801357064694,3.49621561433049E-17));
#63121=CARTESIAN_POINT('Ctrl Pts',(1.09142895154027,1.59229038852923,-3.14041157591089E-18));
#63122=CARTESIAN_POINT('Ctrl Pts',(1.14423757319707,1.54335784953327,-1.00613961606655E-16));
#63123=CARTESIAN_POINT('Ctrl Pts',(1.16947625472704,1.51997165369202,-1.47199231391008E-16));
#63124=CARTESIAN_POINT('Ctrl Pts',(1.19408480623982,1.49585194230134,-1.44940981238328E-16));
#63125=CARTESIAN_POINT('Ctrl Pts',(1.21804196717247,1.47103398018765,-1.04083408558608E-16));
#63126=CARTESIAN_POINT('Ctrl Pts',(1.23020142841566,1.45843761915368,-8.33461403619852E-17));
#63127=CARTESIAN_POINT('Ctrl Pts',(1.24219304748387,1.44566136836505,-3.17714931440926E-16));
#63128=CARTESIAN_POINT('Ctrl Pts',(1.25401379483509,1.43270976178997,-3.05311331771918E-16));
#63129=CARTESIAN_POINT('Ctrl Pts',(1.26389181876557,1.42188673377951,-2.94946246493115E-16));
#63130=CARTESIAN_POINT('Ctrl Pts',(1.27364380619492,1.41094858444086,-5.46603369369435E-16));
#63131=CARTESIAN_POINT('Ctrl Pts',(1.28326720497828,1.3998998522991,-5.34294830600857E-16));
#63132=CARTESIAN_POINT('Ctrl Pts',(1.330154786252,1.3460676940429,-4.74324582576826E-16));
#63133=CARTESIAN_POINT('Ctrl Pts',(1.37400431756963,1.2896005558432,-2.78813144032988E-17));
#63134=CARTESIAN_POINT('Ctrl Pts',(1.41465239664765,1.2308327382907,1.45716771982052E-16));
#63135=CARTESIAN_POINT('Ctrl Pts',(1.44369336478921,1.18884614615641,2.69743702909727E-16));
#63136=CARTESIAN_POINT('Ctrl Pts',(1.47109927736379,1.14568453076923,1.23340209484872E-16));
#63137=CARTESIAN_POINT('Ctrl Pts',(1.4967949674738,1.10146499100096,1.52655665885959E-16));
#63138=CARTESIAN_POINT('Ctrl Pts',(1.51164370962241,1.07591189080641,1.69596158676961E-16));
#63139=CARTESIAN_POINT('Ctrl Pts',(1.5259211042574,1.05000546373499,-2.47389032972511E-16));
#63140=CARTESIAN_POINT('Ctrl Pts',(1.53961051084784,1.0237681518455,-2.63677968348475E-16));
#63141=CARTESIAN_POINT('Ctrl Pts',(1.5453767175419,1.01271655786648,-2.70539139983884E-16));
#63142=CARTESIAN_POINT('Ctrl Pts',(1.55103417937643,1.00161467257822,6.72528652799515E-17));
#63143=CARTESIAN_POINT('Ctrl Pts',(1.55658137030158,0.990465869694384,6.24500451351651E-17));
#63144=CARTESIAN_POINT('Ctrl Pts',(1.58759523113096,0.928133884781808,3.5597896440648E-17));
#63145=CARTESIAN_POINT('Ctrl Pts',(1.61517455934254,0.864320573166324,-1.32844578099872E-16));
#63146=CARTESIAN_POINT('Ctrl Pts',(1.639165272121,0.799334213601843,-1.80411241501588E-16));
#63147=CARTESIAN_POINT('Ctrl Pts',(1.66256479067373,0.735949288762567,-2.26805737281603E-16));
#63148=CARTESIAN_POINT('Ctrl Pts',(1.68255047093124,0.671447445488438,-3.92048207771591E-16));
#63149=CARTESIAN_POINT('Ctrl Pts',(1.69893099532196,0.606109731061441,-4.30211422042248E-16));
#63150=CARTESIAN_POINT('Ctrl Pts',(1.70969999791506,0.563154939181291,-4.55300957861645E-16));
#63151=CARTESIAN_POINT('Ctrl Pts',(1.71890982821634,0.519838805550124,-3.77882014063636E-16));
#63152=CARTESIAN_POINT('Ctrl Pts',(1.72649398406889,0.476242912678102,-4.71844785465692E-16));
#63153=CARTESIAN_POINT('Ctrl Pts',(1.73287054571603,0.439588616027976,-5.50846247992205E-16));
#63154=CARTESIAN_POINT('Ctrl Pts',(1.73809775889755,0.402736552578244,-9.42921937940892E-17));
#63155=CARTESIAN_POINT('Ctrl Pts',(1.74213052178609,0.36573694696249,-1.2490009027033E-16));
#63156=CARTESIAN_POINT('Ctrl Pts',(1.74338539139703,0.354223827548557,-1.34424309820125E-16));
#63157=CARTESIAN_POINT('Ctrl Pts',(1.74452450777523,0.342696049837886,-3.03274465566551E-16));
#63158=CARTESIAN_POINT('Ctrl Pts',(1.74554535151306,0.331170337018761,-2.91433543964104E-16));
#63159=CARTESIAN_POINT('Ctrl Pts',(1.75129431083391,0.266262406759456,-2.24750491415529E-16));
#63160=CARTESIAN_POINT('Ctrl Pts',(1.75331011127704,0.201301920292928,9.80627071070611E-17));
#63161=CARTESIAN_POINT('Ctrl Pts',(1.75142561531544,0.136549272921142,2.77555756156289E-17));
#63162=CARTESIAN_POINT('Ctrl Pts',(1.75088296778463,0.11790351037964,7.510378979319E-18));
#63163=CARTESIAN_POINT('Ctrl Pts',(1.75001659332986,0.099275023041261,-5.08054903583662E-16));
#63164=CARTESIAN_POINT('Ctrl Pts',(1.74882170147482,0.0806701752180915,
-4.85722573273506E-16));
#63165=CARTESIAN_POINT('Ctrl Pts',(1.74442082328573,0.0121470962041962,
-4.16579971360731E-16));
#63166=CARTESIAN_POINT('Ctrl Pts',(1.73556771390717,-0.056057442313777,
-1.52368272571946E-16));
#63167=CARTESIAN_POINT('Ctrl Pts',(1.72245534586321,-0.123606275893366,
-5.55111512312578E-17));
#63168=CARTESIAN_POINT('Ctrl Pts',(1.71065390208195,-0.184401836184713,
3.16625666268892E-17));
#63169=CARTESIAN_POINT('Ctrl Pts',(1.69540107690307,-0.244666544752314,
-5.10914177950054E-16));
#63170=CARTESIAN_POINT('Ctrl Pts',(1.67680493801022,-0.304129401844208,
-5.82867087928207E-16));
#63171=CARTESIAN_POINT('Ctrl Pts',(1.67349552259788,-0.314711560692091,
-5.95672007842828E-16));
#63172=CARTESIAN_POINT('Ctrl Pts',(1.67008173945308,-0.325263020743978,
-2.82234476894323E-16));
#63173=CARTESIAN_POINT('Ctrl Pts',(1.66656691458475,-0.335775244456298,
-2.77555756156289E-16));
#63174=CARTESIAN_POINT('Ctrl Pts',(1.64601434320315,-0.39724437487395,-2.5019742521657E-16));
#63175=CARTESIAN_POINT('Ctrl Pts',(1.6219871213203,-0.457449913435399,-1.49651752513019E-16));
#63176=CARTESIAN_POINT('Ctrl Pts',(1.59467186427628,-0.5161179062652,-1.94289029309402E-16));
#63177=CARTESIAN_POINT('Ctrl Pts',(1.56746479951959,-0.57455352257637,-2.38749503483388E-16));
#63178=CARTESIAN_POINT('Ctrl Pts',(1.53699493854014,-0.631464584970275,
-4.11608014004163E-16));
#63179=CARTESIAN_POINT('Ctrl Pts',(1.50340708769257,-0.686547887629179,
-4.71844785465692E-16));
#63180=CARTESIAN_POINT('Ctrl Pts',(1.47050686756616,-0.740503491725204,
-5.30848353445754E-16));
#63181=CARTESIAN_POINT('Ctrl Pts',(1.43461427022078,-0.792706028859038,
8.26037042042841E-17));
#63182=CARTESIAN_POINT('Ctrl Pts',(1.39583852741916,-0.842828743497358,
1.94289029309402E-16));
#63183=CARTESIAN_POINT('Ctrl Pts',(1.38891448399703,-0.851778974428235,
2.14232271779286E-16));
#63184=CARTESIAN_POINT('Ctrl Pts',(1.38189845475662,-0.860662765012678,
1.05754276149716E-16));
#63185=CARTESIAN_POINT('Ctrl Pts',(1.3747909965488,-0.869478087839508,1.11022302462516E-16));
#63186=CARTESIAN_POINT('Ctrl Pts',(1.36801000346398,-0.877888498619479,
1.1604835382339E-16));
#63187=CARTESIAN_POINT('Ctrl Pts',(1.36114891147745,-0.8862326313589,4.78426519390645E-16));
#63188=CARTESIAN_POINT('Ctrl Pts',(1.35421355798306,-0.894502968665375,
4.71844785465692E-16));
#63189=CARTESIAN_POINT('Ctrl Pts',(1.3143417576089,-0.942049678199007,4.34005967100638E-16));
#63190=CARTESIAN_POINT('Ctrl Pts',(1.27196760499602,-0.987223303029092,
-4.84873724376989E-16));
#63191=CARTESIAN_POINT('Ctrl Pts',(1.22722986402911,-1.02975664627632,-3.05311331771918E-16));
#63192=CARTESIAN_POINT('Ctrl Pts',(1.18329662429212,-1.07152512911229,-1.2897793916942E-16));
#63193=CARTESIAN_POINT('Ctrl Pts',(1.13708333146208,-1.1107479710078,1.42267300457324E-16));
#63194=CARTESIAN_POINT('Ctrl Pts',(1.08869802628341,-1.14712822354107,1.94289029309402E-16));
#63195=CARTESIAN_POINT('Ctrl Pts',(1.04185702701945,-1.1823473334721,2.44650389103912E-16));
#63196=CARTESIAN_POINT('Ctrl Pts',(0.99297984330778,-1.21490270865201,1.66616011326585E-16));
#63197=CARTESIAN_POINT('Ctrl Pts',(0.942151955941521,-1.24447758118399,
1.11022302462516E-16));
#63198=CARTESIAN_POINT('Ctrl Pts',(0.929425469464971,-1.25188265416315,
9.71025308430195E-17));
#63199=CARTESIAN_POINT('Ctrl Pts',(0.916576650468056,-1.25910062269163,
1.9641793555709E-16));
#63200=CARTESIAN_POINT('Ctrl Pts',(0.903606778650242,-1.26612599672281,
1.94289029309402E-16));
#63201=CARTESIAN_POINT('Ctrl Pts',(1.88079991776263,-0.516378774142081,
11.046));
#63202=CARTESIAN_POINT('Ctrl Pts',(1.79754570390634,-0.821182550519846,
11.028067538919));
#63203=CARTESIAN_POINT('Ctrl Pts',(1.64446793279769,-1.10682480125595,11.010135077838));
#63204=CARTESIAN_POINT('Ctrl Pts',(1.43091597726206,-1.33587557506818,10.9922026167571));
#63205=CARTESIAN_POINT('Ctrl Pts',(0.9898515831668,-1.80895080641009,10.9551653999286));
#63206=CARTESIAN_POINT('Ctrl Pts',(0.290818548970629,-2.04062011418838,
10.9181281831001));
#63207=CARTESIAN_POINT('Ctrl Pts',(-0.345744266721549,-1.9262440956347,
10.8810909662716));
#63208=CARTESIAN_POINT('Ctrl Pts',(-0.982307082413709,-1.81186807708102,
10.8440537494431));
#63209=CARTESIAN_POINT('Ctrl Pts',(-1.55639967960188,-1.35144673219537,
10.8070165326147));
#63210=CARTESIAN_POINT('Ctrl Pts',(-1.80573868997825,-0.754924386616321,
10.7699793157862));
#63211=CARTESIAN_POINT('Ctrl Pts',(-1.90472245868201,-0.518114150655666,
10.7552761078989));
#63212=CARTESIAN_POINT('Ctrl Pts',(-1.95252608806662,-0.259854826956367,
10.7405729000116));
#63213=CARTESIAN_POINT('Ctrl Pts',(-1.95129684289216,-0.00113636086278679,
10.7258696921242));
#63214=CARTESIAN_POINT('Origin',(0.,0.,-1.29405622560369));
#63215=CARTESIAN_POINT('',(-0.903606778650172,-1.26612599672286,0.));
#63216=CARTESIAN_POINT('Ctrl Pts',(-0.905549614304886,-1.26792015305981,
1.24276674021151E-15));
#63217=CARTESIAN_POINT('Ctrl Pts',(-0.513706458239086,-1.54472437079514,
0.0344950590738082));
#63218=CARTESIAN_POINT('Ctrl Pts',(0.587535178885047,-1.72169358136003,
0.106052258091336));
#63219=CARTESIAN_POINT('Ctrl Pts',(1.77508460417327,-0.479721809770191,
0.214671597052585));
#63220=CARTESIAN_POINT('Ctrl Pts',(1.3650560094313,1.23222299189869,0.325858016883748));
#63221=CARTESIAN_POINT('Ctrl Pts',(-0.295638381403906,1.81478253869214,
0.43704443671491));
#63222=CARTESIAN_POINT('Ctrl Pts',(-1.41307745535963,0.946781319192958,
0.526443839621562));
#63223=CARTESIAN_POINT('Ctrl Pts',(-1.55414936746312,0.214718667413076,
0.578781102584494));
#63224=CARTESIAN_POINT('Ctrl Pts',(-1.55326046963413,0.000729270061605551,
0.594056225603705));
#63225=CARTESIAN_POINT('Origin',(0.,0.,0.));
#63226=CARTESIAN_POINT('Ctrl Pts',(-0.685825729128748,1.39614588036674,
-0.230074082272066));
#63227=CARTESIAN_POINT('Ctrl Pts',(-1.15028016933624,1.16799292759742,-0.193011942328345));
#63228=CARTESIAN_POINT('Ctrl Pts',(-1.82555218707277,0.215691441263552,
-0.118887662440903));
#63229=CARTESIAN_POINT('Ctrl Pts',(-1.16942936218886,-1.42059634545264,
-0.00770124260974049));
#63230=CARTESIAN_POINT('Ctrl Pts',(0.559468948314244,-1.75104601534012,
0.103485177221422));
#63231=CARTESIAN_POINT('Ctrl Pts',(1.77508460417327,-0.479721809770191,
0.214671597052585));
#63232=CARTESIAN_POINT('Ctrl Pts',(1.3650560094313,1.23222299189869,0.325858016883748));
#63233=CARTESIAN_POINT('Ctrl Pts',(-0.295638381403906,1.81478253869214,
0.43704443671491));
#63234=CARTESIAN_POINT('Ctrl Pts',(-1.68540213790592,0.735245708832444,
0.548230856546073));
#63235=CARTESIAN_POINT('Ctrl Pts',(-1.53132379752993,-1.01797781965797,
0.659417276377235));
#63236=CARTESIAN_POINT('Ctrl Pts',(0.0255447675030308,-1.83860034663711,
0.770603696208398));
#63237=CARTESIAN_POINT('Ctrl Pts',(1.55899683301632,-0.975032021788082,
0.881790116039561));
#63238=CARTESIAN_POINT('Ctrl Pts',(1.66434877052597,0.781732535368643,0.992976535870723));
#63239=CARTESIAN_POINT('Ctrl Pts',(0.245080507541896,1.82238325373942,1.10416295570189));
#63240=CARTESIAN_POINT('Ctrl Pts',(-1.39868975820189,1.19365863723167,1.21534937553305));
#63241=CARTESIAN_POINT('Ctrl Pts',(-1.76120077222934,-0.528512641939849,
1.32653579536421));
#63242=CARTESIAN_POINT('Ctrl Pts',(-0.510374815939226,-1.76654153931159,
1.43772221519537));
#63243=CARTESIAN_POINT('Ctrl Pts',(1.20797626960931,-1.38634273102519,1.54890863502654));
#63244=CARTESIAN_POINT('Ctrl Pts',(1.81976886629041,0.263806680570579,1.6600950548577));
#63245=CARTESIAN_POINT('Ctrl Pts',(0.764574137846417,1.67229745635935,1.77128147468886));
#63246=CARTESIAN_POINT('Ctrl Pts',(-0.991003621173195,1.54889135395602,
1.88246789452002));
#63247=CARTESIAN_POINT('Ctrl Pts',(-1.83877909581896,0.00663349951290586,
1.99365431435119));
#63248=CARTESIAN_POINT('Ctrl Pts',(-1.00215313155719,-1.54170088892816,
2.10484073418235));
#63249=CARTESIAN_POINT('Ctrl Pts',(0.752488571272716,-1.67777039880966,
2.21602715401351));
#63250=CARTESIAN_POINT('Ctrl Pts',(1.81781810074028,-0.276929424335053,
2.32721357384467));
#63251=CARTESIAN_POINT('Ctrl Pts',(1.21794738393109,1.37759091140133,2.43839999367584));
#63252=CARTESIAN_POINT('Ctrl Pts',(-0.497615974795104,1.77017821004958,
2.549586413507));
#63253=CARTESIAN_POINT('Ctrl Pts',(-1.75734151264734,0.541205469518692,
2.66077283333817));
#63254=CARTESIAN_POINT('Ctrl Pts',(-1.40726598433086,-1.1835349598584,2.77195925316932));
#63255=CARTESIAN_POINT('Ctrl Pts',(0.231926238140432,-1.82410602009977,
2.88314567300049));
#63256=CARTESIAN_POINT('Ctrl Pts',(1.65866396469461,-0.793716828903688,
2.99433209283165));
#63257=CARTESIAN_POINT('Ctrl Pts',(1.56599354026699,0.96375141196464,3.10551851266282));
#63258=CARTESIAN_POINT('Ctrl Pts',(0.0388050940998321,1.83838154825996,
3.21670493249398));
#63259=CARTESIAN_POINT('Ctrl Pts',(-1.52393050178991,1.02897443019027,3.32789135232514));
#63260=CARTESIAN_POINT('Ctrl Pts',(-1.69067964401488,-0.723017906820314,
3.4390777721563));
#63261=CARTESIAN_POINT('Ctrl Pts',(-0.308692884081366,-1.81269447386996,
3.55026419198746));
#63262=CARTESIAN_POINT('Ctrl Pts',(1.35606994996762,-1.24186426112907,3.66145061181863));
#63263=CARTESIAN_POINT('Ctrl Pts',(1.77861387826841,0.466567491694538,3.77263703164979));
#63264=CARTESIAN_POINT('Ctrl Pts',(0.571870330903418,1.74760318061885,3.88382345148095));
#63265=CARTESIAN_POINT('Ctrl Pts',(-1.15873124952358,1.42775853828764,3.99500987131212));
#63266=CARTESIAN_POINT('Ctrl Pts',(-1.82788473512851,-0.199974866820836,
4.10619629114327));
#63267=CARTESIAN_POINT('Ctrl Pts',(-0.822616502622442,-1.64452261823584,
4.21738271097444));
#63268=CARTESIAN_POINT('Ctrl Pts',(0.936204134582059,-1.58261630557358,
4.3285691308056));
#63269=CARTESIAN_POINT('Ctrl Pts',(1.83742116834086,-0.0709647969689106,
4.43975555063676));
#63270=CARTESIAN_POINT('Ctrl Pts',(1.0554806974386,1.50569354438759,4.55094197046793));
#63271=CARTESIAN_POINT('Ctrl Pts',(-0.693325883166112,1.70307127625589,
4.66212839029909));
#63272=CARTESIAN_POINT('Ctrl Pts',(-1.80701587562324,0.340361833232659,
4.77331481013025));
#63273=CARTESIAN_POINT('Ctrl Pts',(-1.26540093064824,-1.33413381524886,
4.88450122996142));
#63274=CARTESIAN_POINT('Ctrl Pts',(0.435376164803608,-1.7865050090601,4.99568764979258));
#63275=CARTESIAN_POINT('Ctrl Pts',(1.73732980498774,-0.602360109052031,
5.10687406962374));
#63276=CARTESIAN_POINT('Ctrl Pts',(1.44781397169404,1.13357278356683,5.21806048945491));
#63277=CARTESIAN_POINT('Ctrl Pts',(-0.167962271460079,1.83110382765203,
5.32924690928607));
#63278=CARTESIAN_POINT('Ctrl Pts',(-1.62987778710162,0.851264325217889,
5.44043332911723));
#63279=CARTESIAN_POINT('Ctrl Pts',(-1.59875453933454,-0.908370230265797,
5.55161974894839));
#63280=CARTESIAN_POINT('Ctrl Pts',(-0.103102773360761,-1.83589824620028,
5.66280616877956));
#63281=CARTESIAN_POINT('Ctrl Pts',(1.4869956060099,-1.08166382022474,5.77399258861071));
#63282=CARTESIAN_POINT('Ctrl Pts',(1.71494149863546,0.663421591850831,5.88517900844189));
#63283=CARTESIAN_POINT('Ctrl Pts',(0.371926577693494,1.80078404398782,5.99636542827304));
#63284=CARTESIAN_POINT('Ctrl Pts',(-1.311789224034,1.28855018683177,6.10755184810421));
#63285=CARTESIAN_POINT('Ctrl Pts',(-1.79384918603911,-0.404051543769803,
6.21873826793537));
#63286=CARTESIAN_POINT('Ctrl Pts',(-0.632665469493242,-1.72652453095426,
6.32992468776653));
#63287=CARTESIAN_POINT('Ctrl Pts',(1.10806726459172,-1.46742614445027,6.44111110759769));
#63288=CARTESIAN_POINT('Ctrl Pts',(1.83376231205259,0.135898253011021,6.55229752742886));
#63289=CARTESIAN_POINT('Ctrl Pts',(0.879651525947856,1.61473395492061,6.66348394726001));
#63290=CARTESIAN_POINT('Ctrl Pts',(-0.880258220622017,1.61440330069759,
6.77467036709119));
#63291=CARTESIAN_POINT('Ctrl Pts',(-1.83381324808445,0.13520918395534,6.88585678692234));
#63292=CARTESIAN_POINT('Ctrl Pts',(-1.1075157823663,-1.46784241118916,6.99704320675351));
#63293=CARTESIAN_POINT('Ctrl Pts',(0.633314188332071,-1.72628667698419,
7.10822962658467));
#63294=CARTESIAN_POINT('Ctrl Pts',(1.7940008868909,-0.403377453646542,7.21941604641583));
#63295=CARTESIAN_POINT('Ctrl Pts',(1.31130494233742,1.28904301731096,7.33060246624699));
#63296=CARTESIAN_POINT('Ctrl Pts',(-0.372603218894873,1.80064416072257,
7.44178888607816));
#63297=CARTESIAN_POINT('Ctrl Pts',(-1.71519066664489,0.662777133981789,
7.55297530590932));
#63298=CARTESIAN_POINT('Ctrl Pts',(-1.48658905212271,-1.08222250133236,
7.66416172574049));
#63299=CARTESIAN_POINT('Ctrl Pts',(0.103792628149562,-1.8358593744105,7.77534814557165));
#63300=CARTESIAN_POINT('Ctrl Pts',(1.59909575810308,-0.907769413831382,
7.8865345654028));
#63301=CARTESIAN_POINT('Ctrl Pts',(1.62955779866738,0.851876712390422,7.99772098523398));
#63302=CARTESIAN_POINT('Ctrl Pts',(0.167274199086701,1.83116681231986,8.10890740506512));
#63303=CARTESIAN_POINT('Ctrl Pts',(-1.44823982381472,1.1330286690894,8.2200938248963));
#63304=CARTESIAN_POINT('Ctrl Pts',(-1.73710333792674,-0.603012890298399,
8.33128024472746));
#63305=CARTESIAN_POINT('Ctrl Pts',(-0.434704832044991,-1.78666848096071,
8.44246666455862));
#63306=CARTESIAN_POINT('Ctrl Pts',(1.26590215885116,-1.33365823077974,8.55365308438979));
#63307=CARTESIAN_POINT('Ctrl Pts',(1.8068878531032,0.341040818691465,8.66483950422094));
#63308=CARTESIAN_POINT('Ctrl Pts',(0.69268588294083,1.70333168137465,8.77602592405212));
#63309=CARTESIAN_POINT('Ctrl Pts',(-1.05604640517969,1.5052968290502,8.88721234388326));
#63310=CARTESIAN_POINT('Ctrl Pts',(-1.83739437498563,-0.0716552286239433,
8.99839876371444));
#63311=CARTESIAN_POINT('Ctrl Pts',(-0.935609375970031,-1.5829679799695,
9.1095851835456));
#63312=CARTESIAN_POINT('Ctrl Pts',(0.823234386500799,-1.64421340203127,
9.22077160337675));
#63313=CARTESIAN_POINT('Ctrl Pts',(1.82795976495949,-0.199287985657338,
9.33195802320793));
#63314=CARTESIAN_POINT('Ctrl Pts',(1.15819463928053,1.42819381470141,9.44314444303908));
#63315=CARTESIAN_POINT('Ctrl Pts',(-0.572526917402423,1.74738822826618,
9.55433086287024));
#63316=CARTESIAN_POINT('Ctrl Pts',(-1.77878918025408,0.46589901053406,9.66551728270142));
#63317=CARTESIAN_POINT('Ctrl Pts',(-1.35560300066214,-1.24237352171324,
9.77670370253256));
#63318=CARTESIAN_POINT('Ctrl Pts',(0.309373610575528,-1.81257875466721,
9.88789012236375));
#63319=CARTESIAN_POINT('Ctrl Pts',(1.69095195914933,-0.722381792257861,
9.99907654219489));
#63320=CARTESIAN_POINT('Ctrl Pts',(1.52354231364944,1.0295455294481,10.1102629620261));
#63321=CARTESIAN_POINT('Ctrl Pts',(-0.0394931635484403,1.83836962465064,
10.2214493818572));
#63322=CARTESIAN_POINT('Ctrl Pts',(-1.56636075542215,0.963157594965877,
10.3326358016884));
#63323=CARTESIAN_POINT('Ctrl Pts',(-1.65835572967195,-0.794329933758677,
10.4438222215196));
#63324=CARTESIAN_POINT('Ctrl Pts',(-0.231259578302998,-1.82421227428175,
10.5550086413507));
#63325=CARTESIAN_POINT('Ctrl Pts',(1.40774638007895,-1.1829694620695,10.6661950611819));
#63326=CARTESIAN_POINT('Ctrl Pts',(1.75706993010233,0.541796064983141,10.7773814810131));
#63327=CARTESIAN_POINT('Ctrl Pts',(0.497080432048737,1.77049779856472,10.8885679008442));
#63328=CARTESIAN_POINT('Ctrl Pts',(-1.21871201614337,1.37688031013954,10.9997543206754));
#63329=CARTESIAN_POINT('Ctrl Pts',(-1.81724153253684,-0.27712968875509,
11.1109407405065));
#63330=CARTESIAN_POINT('Ctrl Pts',(-0.75277483453787,-1.67898453189698,
11.2221271603377));
#63331=CARTESIAN_POINT('Ctrl Pts',(1.00462758039806,-1.53944373403644,11.3333135801688));
#63332=CARTESIAN_POINT('Ctrl Pts',(1.55754888396286,-0.511266487217653,
11.4074378600563));
#63333=CARTESIAN_POINT('Ctrl Pts',(1.55548765964692,0.00619602180124784,
11.4445));
#63334=CARTESIAN_POINT('Ctrl Pts',(-0.74439243930934,1.51537102412034,-0.153382721514711));
#63335=CARTESIAN_POINT('Ctrl Pts',(-1.24850938769699,1.26773474301532,-0.11632058157099));
#63336=CARTESIAN_POINT('Ctrl Pts',(-1.98144687185762,0.234110607521693,
-0.042196301683548));
#63337=CARTESIAN_POINT('Ctrl Pts',(-1.26929384324154,-1.54190945884872,
0.0689901181476148));
#63338=CARTESIAN_POINT('Ctrl Pts',(0.607245306591998,-1.90057817801302,
0.180176537978778));
#63339=CARTESIAN_POINT('Ctrl Pts',(1.92666956394248,-0.520688088821623,
0.29136295780994));
#63340=CARTESIAN_POINT('Ctrl Pts',(1.48162620545796,1.33744979191402,0.402549377641103));
#63341=CARTESIAN_POINT('Ctrl Pts',(-0.320884689126903,1.9697575395855,0.513735797472264));
#63342=CARTESIAN_POINT('Ctrl Pts',(-1.82932858212653,0.798032683003624,
0.624922217303428));
#63343=CARTESIAN_POINT('Ctrl Pts',(-1.66209258212561,-1.10490895887015,
0.736108637134591));
#63344=CARTESIAN_POINT('Ctrl Pts',(0.0277261860929502,-1.99560929084259,
0.847295056965753));
#63345=CARTESIAN_POINT('Ctrl Pts',(1.69212878157669,-1.0582957656395,0.958481476796916));
#63346=CARTESIAN_POINT('Ctrl Pts',(1.80647734334385,0.848489294255244,1.06966789662808));
#63347=CARTESIAN_POINT('Ctrl Pts',(0.266009379770665,1.97800732458805,1.18085431645924));
#63348=CARTESIAN_POINT('Ctrl Pts',(-1.51813213871049,1.2955921992025,1.29204073629041));
#63349=CARTESIAN_POINT('Ctrl Pts',(-1.91160010957712,-0.573645458357494,
1.40322715612156));
#63350=CARTESIAN_POINT('Ctrl Pts',(-0.553958736254638,-1.91739695630841,
1.51441357595273));
#63351=CARTESIAN_POINT('Ctrl Pts',(1.31113249878304,-1.50473072594935,1.62559999578389));
#63352=CARTESIAN_POINT('Ctrl Pts',(1.9751696791516,0.286334691329668,1.73678641561505));
#63353=CARTESIAN_POINT('Ctrl Pts',(0.829865639814035,1.81510481441338,1.84797283544622));
#63354=CARTESIAN_POINT('Ctrl Pts',(-1.07563127424026,1.68116033596642,1.95915925527738));
#63355=CARTESIAN_POINT('Ctrl Pts',(-1.99580330447296,0.00719997322039096,
2.07034567510854));
#63356=CARTESIAN_POINT('Ctrl Pts',(-1.08773290717609,-1.67335583465575,
2.18153209493971));
#63357=CARTESIAN_POINT('Ctrl Pts',(0.816748015321165,-1.82104512374819,
2.29271851477087));
#63358=CARTESIAN_POINT('Ctrl Pts',(1.97305232620797,-0.300578063700233,
2.40390493460203));
#63359=CARTESIAN_POINT('Ctrl Pts',(1.32195510545613,1.49523153675082,2.51509135443319));
#63360=CARTESIAN_POINT('Ctrl Pts',(-0.54011034229875,1.92134418384253,2.62627777426435));
#63361=CARTESIAN_POINT('Ctrl Pts',(-1.90741128502276,0.587422201459822,
2.73746419409552));
#63362=CARTESIAN_POINT('Ctrl Pts',(-1.52744073944838,-1.28460400121777,
2.84865061392668));
#63363=CARTESIAN_POINT('Ctrl Pts',(0.251731789602741,-1.9798772081443,2.95983703375785));
#63364=CARTESIAN_POINT('Ctrl Pts',(1.80030707836241,-0.861496997406464,
3.071023453589));
#63365=CARTESIAN_POINT('Ctrl Pts',(1.69972297898904,1.04605183790867,3.18220987342017));
#63366=CARTESIAN_POINT('Ctrl Pts',(0.0421188903066005,1.99537180797957,
3.29339629325133));
#63367=CARTESIAN_POINT('Ctrl Pts',(-1.65406792919015,1.11684463493277,3.4045827130825));
#63368=CARTESIAN_POINT('Ctrl Pts',(-1.83505676565636,-0.784760676748056,
3.51576913291366));
#63369=CARTESIAN_POINT('Ctrl Pts',(-0.335053992900935,-1.96749116257395,
3.62695555274482));
#63370=CARTESIAN_POINT('Ctrl Pts',(1.47187277329603,-1.34791438607496,3.73814197257599));
#63371=CARTESIAN_POINT('Ctrl Pts',(1.93050022360002,0.506410445822938,3.84932839240714));
#63372=CARTESIAN_POINT('Ctrl Pts',(0.620705716495424,1.89684133929807,3.96051481223831));
#63373=CARTESIAN_POINT('Ctrl Pts',(-1.25768215554202,1.54968327363698,4.07170123206947));
#63374=CARTESIAN_POINT('Ctrl Pts',(-1.9839786099702,-0.217051901949521,
4.18288765190064));
#63375=CARTESIAN_POINT('Ctrl Pts',(-0.892864584974339,-1.78495811879663,
4.29407407173179));
#63376=CARTESIAN_POINT('Ctrl Pts',(1.01615213578872,-1.71776526041577,4.40526049156296));
#63377=CARTESIAN_POINT('Ctrl Pts',(1.99432941554622,-0.0770249001709277,
4.51644691139412));
#63378=CARTESIAN_POINT('Ctrl Pts',(1.14561442891388,1.6342736102696,4.62763333122529));
#63379=CARTESIAN_POINT('Ctrl Pts',(-0.752533075803338,1.84850659257176,
4.73881975105645));
#63380=CARTESIAN_POINT('Ctrl Pts',(-1.96132763527948,0.369427340688636,
4.85000617088761));
#63381=CARTESIAN_POINT('Ctrl Pts',(-1.3734609908354,-1.44806338245697,4.96119259071877));
#63382=CARTESIAN_POINT('Ctrl Pts',(0.472555507281729,-1.9390652246629,5.07237901054994));
#63383=CARTESIAN_POINT('Ctrl Pts',(1.88569065943703,-0.653799196903168,
5.1835654303811));
#63384=CARTESIAN_POINT('Ctrl Pts',(1.57145135896933,1.23037525956625,5.29475185021226));
#63385=CARTESIAN_POINT('Ctrl Pts',(-0.182305561972616,1.98747259981946,
5.40593827004342));
#63386=CARTESIAN_POINT('Ctrl Pts',(-1.76906267902489,0.923958814363803,
5.51712468987459));
#63387=CARTESIAN_POINT('Ctrl Pts',(-1.73528163328608,-0.985941329968107,
5.62831110970574));
#63388=CARTESIAN_POINT('Ctrl Pts',(-0.111907328205795,-1.99267644208816,
5.73949752953692));
#63389=CARTESIAN_POINT('Ctrl Pts',(1.61397894448518,-1.17403348321834,5.85068394936807));
#63390=CARTESIAN_POINT('Ctrl Pts',(1.86139048335769,0.720075080408093,5.96187036919923));
#63391=CARTESIAN_POINT('Ctrl Pts',(0.403687585131819,1.9545636307293,6.0730567890304));
#63392=CARTESIAN_POINT('Ctrl Pts',(-1.42381065460884,1.39858709874703,6.18424320886156));
#63393=CARTESIAN_POINT('Ctrl Pts',(-1.94703656429618,-0.438555891823412,
6.29542962869273));
#63394=CARTESIAN_POINT('Ctrl Pts',(-0.686692511086116,-1.87396265922711,
6.40661604852388));
#63395=CARTESIAN_POINT('Ctrl Pts',(1.20269167366484,-1.59273833100625,6.51780246835505));
#63396=CARTESIAN_POINT('Ctrl Pts',(1.99035810790665,0.147503407586138,6.62898888818621));
#63397=CARTESIAN_POINT('Ctrl Pts',(0.954770165847204,1.75262562555938,6.74017530801738));
#63398=CARTESIAN_POINT('Ctrl Pts',(-0.9554286697633,1.7522667348191,6.85136172784854));
#63399=CARTESIAN_POINT('Ctrl Pts',(-1.99041339366714,0.146755494853507,
6.9625481476797));
#63400=CARTESIAN_POINT('Ctrl Pts',(-1.20209309711463,-1.59319014522084,
7.07373456751086));
#63401=CARTESIAN_POINT('Ctrl Pts',(0.687396627858533,-1.87370449350154,
7.18492098734203));
#63402=CARTESIAN_POINT('Ctrl Pts',(1.94720121977979,-0.437824237162718,
7.29610740717318));
#63403=CARTESIAN_POINT('Ctrl Pts',(1.42328501723757,1.39912201493195,7.40729382700435));
#63404=CARTESIAN_POINT('Ctrl Pts',(-0.404422008722263,1.95441180200575,
7.51848024683551));
#63405=CARTESIAN_POINT('Ctrl Pts',(-1.86166092929526,0.719375588474842,
7.62966666666667));
#63406=CARTESIAN_POINT('Ctrl Pts',(-1.61353767256008,-1.17463987340584,
7.74085308649784));
#63407=CARTESIAN_POINT('Ctrl Pts',(0.112656093769942,-1.99263425080664,
7.852039506329));
#63408=CARTESIAN_POINT('Ctrl Pts',(1.73565199074082,-0.985289206269375,
7.96322592616017));
#63409=CARTESIAN_POINT('Ctrl Pts',(1.76871536488809,0.924623496894334,8.07441234599133));
#63410=CARTESIAN_POINT('Ctrl Pts',(0.181558731034875,1.98754096312013,8.18559876582249));
#63411=CARTESIAN_POINT('Ctrl Pts',(-1.57191357711808,1.22978467993954,8.29678518565365));
#63412=CARTESIAN_POINT('Ctrl Pts',(-1.88544485301595,-0.6545077229961,8.40797160548482));
#63413=CARTESIAN_POINT('Ctrl Pts',(-0.471826845453332,-1.93924265639472,
8.51915802531597));
#63414=CARTESIAN_POINT('Ctrl Pts',(1.37400502187529,-1.44754718502077,8.63034444514714));
#63415=CARTESIAN_POINT('Ctrl Pts',(1.96118868016023,0.370164308726493,8.7415308649783));
#63416=CARTESIAN_POINT('Ctrl Pts',(0.751838422178375,1.84878923522181,8.85271728480947));
#63417=CARTESIAN_POINT('Ctrl Pts',(-1.14622844578058,1.63384301706618,8.96390370464062));
#63418=CARTESIAN_POINT('Ctrl Pts',(-1.99430033414812,-0.077774291863319,
9.0750901244718));
#63419=CARTESIAN_POINT('Ctrl Pts',(-1.01550658722561,-1.71814696636568,
9.18627654430294));
#63420=CARTESIAN_POINT('Ctrl Pts',(0.893535233606871,-1.78462249679383,
9.29746296413412));
#63421=CARTESIAN_POINT('Ctrl Pts',(1.98406004704164,-0.216306363946107,
9.40864938396527));
#63422=CARTESIAN_POINT('Ctrl Pts',(1.2570997209806,1.55015572087487,9.51983580379645));
#63423=CARTESIAN_POINT('Ctrl Pts',(-0.621418372793996,1.8966080308943,9.63102222362759));
#63424=CARTESIAN_POINT('Ctrl Pts',(-1.93069049565776,0.50568487910749,9.74220864345877));
#63425=CARTESIAN_POINT('Ctrl Pts',(-1.47136594843111,-1.34846713542859,
9.85339506328992));
#63426=CARTESIAN_POINT('Ctrl Pts',(0.335792850651442,-1.96736556142493,
9.9645814831211));
#63427=CARTESIAN_POINT('Ctrl Pts',(1.83535233538869,-0.784070240605622,
10.0757679029522));
#63428=CARTESIAN_POINT('Ctrl Pts',(1.65364659137136,1.11746450372967,10.1869543227834));
#63429=CARTESIAN_POINT('Ctrl Pts',(-0.0428657180698079,1.99535886614283,
10.2981407426146));
#63430=CARTESIAN_POINT('Ctrl Pts',(-1.70012155281541,1.04540731136874,10.4093271624457));
#63431=CARTESIAN_POINT('Ctrl Pts',(-1.79997252133044,-0.862162458906591,
10.5205135822769));
#63432=CARTESIAN_POINT('Ctrl Pts',(-0.251008199743871,-1.97999253599851,
10.6317000021081));
#63433=CARTESIAN_POINT('Ctrl Pts',(1.52796215902707,-1.28399021223231,10.7428864219392));
#63434=CARTESIAN_POINT('Ctrl Pts',(1.90711651044001,0.588063231359589,10.8540728417704));
#63435=CARTESIAN_POINT('Ctrl Pts',(0.539529066393858,1.92169106390877,10.9652592616015));
#63436=CARTESIAN_POINT('Ctrl Pts',(-1.32278503412967,1.49446025304978,11.0764456814327));
#63437=CARTESIAN_POINT('Ctrl Pts',(-1.97242652143987,-0.300795429882017,
11.1876321012639));
#63438=CARTESIAN_POINT('Ctrl Pts',(-0.817058724297523,-1.82236293883171,
11.2988185210951));
#63439=CARTESIAN_POINT('Ctrl Pts',(1.09041866382002,-1.67090592797485,11.4100049409262));
#63440=CARTESIAN_POINT('Ctrl Pts',(1.69055718360052,-0.554926552610627,
11.4841292208136));
#63441=CARTESIAN_POINT('Ctrl Pts',(1.6883199391646,0.00672513670271936,
11.5211913607574));
#63442=CARTESIAN_POINT('Ctrl Pts',(-0.802959149489932,1.63459616787394,
-0.0766913607573554));
#63443=CARTESIAN_POINT('Ctrl Pts',(-1.34673860605774,1.36747655843322,-0.0396292208136346));
#63444=CARTESIAN_POINT('Ctrl Pts',(-2.13734155664247,0.252529773779836,
0.0344950590738073));
#63445=CARTESIAN_POINT('Ctrl Pts',(-1.36915832429422,-1.66322257224481,
0.14568147890497));
#63446=CARTESIAN_POINT('Ctrl Pts',(0.655021664869751,-2.05011034068591,
0.256867898736133));
#63447=CARTESIAN_POINT('Ctrl Pts',(2.0782545237117,-0.561654367873057,0.368054318567295));
#63448=CARTESIAN_POINT('Ctrl Pts',(1.59819640148463,1.44267659192936,0.479240738398458));
#63449=CARTESIAN_POINT('Ctrl Pts',(-0.346130996849898,2.12473254047885,
0.590427158229621));
#63450=CARTESIAN_POINT('Ctrl Pts',(-1.97325502634714,0.860819657174806,
0.701613578060782));
#63451=CARTESIAN_POINT('Ctrl Pts',(-1.79286136672128,-1.19184009808233,
0.812799997891947));
#63452=CARTESIAN_POINT('Ctrl Pts',(0.0299076046828686,-2.15261823504807,
0.923986417723108));
#63453=CARTESIAN_POINT('Ctrl Pts',(1.82526073013706,-1.14155950949091,1.03517283755427));
#63454=CARTESIAN_POINT('Ctrl Pts',(1.94860591616173,0.915246053141843,1.14635925738543));
#63455=CARTESIAN_POINT('Ctrl Pts',(0.286938251999433,2.13363139543668,1.2575456772166));
#63456=CARTESIAN_POINT('Ctrl Pts',(-1.63757451921909,1.39752576117334,1.36873209704776));
#63457=CARTESIAN_POINT('Ctrl Pts',(-2.0619994469249,-0.618778274775138,
1.47991851687892));
#63458=CARTESIAN_POINT('Ctrl Pts',(-0.597542656570052,-2.06825237330522,
1.59110493671008));
#63459=CARTESIAN_POINT('Ctrl Pts',(1.41428872795678,-1.62311872087351,1.70229135654125));
#63460=CARTESIAN_POINT('Ctrl Pts',(2.13057049201279,0.308862702088754,1.81347777637241));
#63461=CARTESIAN_POINT('Ctrl Pts',(0.895157141781652,1.95791217246742,1.92466419620357));
#63462=CARTESIAN_POINT('Ctrl Pts',(-1.16025892730732,1.81342931797682,2.03585061603473));
#63463=CARTESIAN_POINT('Ctrl Pts',(-2.15282751312695,0.00776644692787891,
2.1470370358659));
#63464=CARTESIAN_POINT('Ctrl Pts',(-1.173312682795,-1.80501078038335,2.25822345569706));
#63465=CARTESIAN_POINT('Ctrl Pts',(0.881007459369614,-1.96431984868673,
2.36940987552822));
#63466=CARTESIAN_POINT('Ctrl Pts',(2.12828655167567,-0.324226703065412,
2.48059629535939));
#63467=CARTESIAN_POINT('Ctrl Pts',(1.42596282698117,1.6128721621003,2.59178271519055));
#63468=CARTESIAN_POINT('Ctrl Pts',(-0.582604709802392,2.07251015763547,
2.70296913502171));
#63469=CARTESIAN_POINT('Ctrl Pts',(-2.05748105739819,0.633638933400953,
2.81415555485287));
#63470=CARTESIAN_POINT('Ctrl Pts',(-1.6476154945659,-1.38567304257714,2.92534197468403));
#63471=CARTESIAN_POINT('Ctrl Pts',(0.271537341065049,-2.13564839618882,
3.0365283945152));
#63472=CARTESIAN_POINT('Ctrl Pts',(1.9419501920302,-0.92927716590924,3.14771481434636));
#63473=CARTESIAN_POINT('Ctrl Pts',(1.83345241771109,1.12835226385271,3.25890123417753));
#63474=CARTESIAN_POINT('Ctrl Pts',(0.045432686513366,2.15236206769919,3.37008765400868));
#63475=CARTESIAN_POINT('Ctrl Pts',(-1.78420535659039,1.20471483967528,3.48127407383985));
#63476=CARTESIAN_POINT('Ctrl Pts',(-1.97943388729784,-0.8465034466758,3.59246049367101));
#63477=CARTESIAN_POINT('Ctrl Pts',(-0.361415101720502,-2.12228785127793,
3.70364691350217));
#63478=CARTESIAN_POINT('Ctrl Pts',(1.58767559662444,-1.45396451102085,3.81483333333334));
#63479=CARTESIAN_POINT('Ctrl Pts',(2.08238656893164,0.546253399951339,3.9260197531645));
#63480=CARTESIAN_POINT('Ctrl Pts',(0.669541102087431,2.04607949797729,4.03720617299566));
#63481=CARTESIAN_POINT('Ctrl Pts',(-1.35663306156047,1.67160800898631,4.14839259282683));
#63482=CARTESIAN_POINT('Ctrl Pts',(-2.14007248481188,-0.234128937078206,
4.25957901265799));
#63483=CARTESIAN_POINT('Ctrl Pts',(-0.963112667326238,-1.92539361935742,
4.37076543248915));
#63484=CARTESIAN_POINT('Ctrl Pts',(1.09610013699538,-1.85291421525797,4.48195185232032));
#63485=CARTESIAN_POINT('Ctrl Pts',(2.15123766275159,-0.0830850033729405,
4.59313827215147));
#63486=CARTESIAN_POINT('Ctrl Pts',(1.23574816038915,1.76285367615161,4.70432469198265));
#63487=CARTESIAN_POINT('Ctrl Pts',(-0.811740268440561,1.99394190888763,
4.8155111118138));
#63488=CARTESIAN_POINT('Ctrl Pts',(-2.11563939493572,0.398492848144611,
4.92669753164497));
#63489=CARTESIAN_POINT('Ctrl Pts',(-1.48152105102257,-1.56199294966507,
5.03788395147612));
#63490=CARTESIAN_POINT('Ctrl Pts',(0.509734849759847,-2.0916254402657,5.1490703713073));
#63491=CARTESIAN_POINT('Ctrl Pts',(2.03405151388631,-0.705238284754304,
5.26025679113844));
#63492=CARTESIAN_POINT('Ctrl Pts',(1.69508874624462,1.32717773556567,5.37144321096963));
#63493=CARTESIAN_POINT('Ctrl Pts',(-0.19664885248515,2.1438413719869,5.48262963080077));
#63494=CARTESIAN_POINT('Ctrl Pts',(-1.90824757094816,0.996653303509719,
5.59381605063195));
#63495=CARTESIAN_POINT('Ctrl Pts',(-1.87180872723762,-1.06351242967042,
5.70500247046309));
#63496=CARTESIAN_POINT('Ctrl Pts',(-0.12071188305083,-2.14945463797604,
5.81618889029427));
#63497=CARTESIAN_POINT('Ctrl Pts',(1.74096228296046,-1.26640314621194,5.92737531012542));
#63498=CARTESIAN_POINT('Ctrl Pts',(2.00783946807991,0.776728568965356,6.0385617299566));
#63499=CARTESIAN_POINT('Ctrl Pts',(0.435448592570146,2.10834321747079,6.14974814978775));
#63500=CARTESIAN_POINT('Ctrl Pts',(-1.53583208518367,1.50862401066228,6.26093456961893));
#63501=CARTESIAN_POINT('Ctrl Pts',(-2.10022394255324,-0.473060239877022,
6.37212098945007));
#63502=CARTESIAN_POINT('Ctrl Pts',(-0.74071955267899,-2.02140078749996,
6.48330740928124));
#63503=CARTESIAN_POINT('Ctrl Pts',(1.29731608273796,-1.71805051756223,6.5944938291124));
#63504=CARTESIAN_POINT('Ctrl Pts',(2.14695390376071,0.15910856216126,6.70568024894357));
#63505=CARTESIAN_POINT('Ctrl Pts',(1.02988880574655,1.89051729619815,6.81686666877473));
#63506=CARTESIAN_POINT('Ctrl Pts',(-1.03059911890458,1.89013016894061,6.92805308860589));
#63507=CARTESIAN_POINT('Ctrl Pts',(-2.14701353924984,0.158301805751674,
7.03923950843705));
#63508=CARTESIAN_POINT('Ctrl Pts',(-1.29667041186295,-1.71853787925252,
7.15042592826822));
#63509=CARTESIAN_POINT('Ctrl Pts',(0.741479067384996,-2.0211223100189,7.26161234809938));
#63510=CARTESIAN_POINT('Ctrl Pts',(2.10040155266868,-0.472271020678894,
7.37279876793055));
#63511=CARTESIAN_POINT('Ctrl Pts',(1.53526509213771,1.50920101255294,7.48398518776171));
#63512=CARTESIAN_POINT('Ctrl Pts',(-0.436240798549652,2.10817944328893,
7.59517160759286));
#63513=CARTESIAN_POINT('Ctrl Pts',(-2.00813119194563,0.775974042967894,
7.70635802742404));
#63514=CARTESIAN_POINT('Ctrl Pts',(-1.74048629299744,-1.26705724547931,
7.81754444725519));
#63515=CARTESIAN_POINT('Ctrl Pts',(0.121519559390324,-2.14940912720278,
7.92873086708636));
#63516=CARTESIAN_POINT('Ctrl Pts',(1.87220822337856,-1.06280899870737,8.03991728691751));
#63517=CARTESIAN_POINT('Ctrl Pts',(1.90787293110882,0.997370281398245,8.15110370674869));
#63518=CARTESIAN_POINT('Ctrl Pts',(0.195843262983046,2.1439151139204,8.26229012657984));
#63519=CARTESIAN_POINT('Ctrl Pts',(-1.69558733042143,1.32654069078969,8.37347654641101));
#63520=CARTESIAN_POINT('Ctrl Pts',(-2.03378636810517,-0.706002555693802,
8.48466296624217));
#63521=CARTESIAN_POINT('Ctrl Pts',(-0.508948858861673,-2.09181683182873,
8.59584938607333));
#63522=CARTESIAN_POINT('Ctrl Pts',(1.48210788489943,-1.56143613926181,8.70703580590451));
#63523=CARTESIAN_POINT('Ctrl Pts',(2.11548950721726,0.399287798761521,8.81822222573564));
#63524=CARTESIAN_POINT('Ctrl Pts',(0.810990961415923,1.99424678906897,8.92940864556684));
#63525=CARTESIAN_POINT('Ctrl Pts',(-1.23641048638147,1.76238920508216,9.04059506539797));
#63526=CARTESIAN_POINT('Ctrl Pts',(-2.15120629331062,-0.0838933551026959,
9.15178148522916));
#63527=CARTESIAN_POINT('Ctrl Pts',(-1.09540379848118,-1.85332595276186,
9.26296790506031));
#63528=CARTESIAN_POINT('Ctrl Pts',(0.963836080712942,-1.9250315915564,9.37415432489147));
#63529=CARTESIAN_POINT('Ctrl Pts',(2.14016032912378,-0.233324742234878,
9.48534074472264));
#63530=CARTESIAN_POINT('Ctrl Pts',(1.35600480268067,1.67211762704833,9.5965271645538));
#63531=CARTESIAN_POINT('Ctrl Pts',(-0.67030982818557,2.04582783352242,9.70771358438496));
#63532=CARTESIAN_POINT('Ctrl Pts',(-2.08259181106143,0.545470747680921,
9.81890000421612));
#63533=CARTESIAN_POINT('Ctrl Pts',(-1.58712889620009,-1.45456074914393,
9.93008642404728));
#63534=CARTESIAN_POINT('Ctrl Pts',(0.362212090727357,-2.12215236818265,
10.0412728438785));
#63535=CARTESIAN_POINT('Ctrl Pts',(1.97975271162804,-0.845758688953388,
10.1524592637096));
#63536=CARTESIAN_POINT('Ctrl Pts',(1.78375086909329,1.20538347801125,10.2636456835408));
#63537=CARTESIAN_POINT('Ctrl Pts',(-0.0462382725911752,2.15234810763501,
10.3748321033719));
#63538=CARTESIAN_POINT('Ctrl Pts',(-1.83388235020868,1.12765702777161,10.4860185232031));
#63539=CARTESIAN_POINT('Ctrl Pts',(-1.94158931298892,-0.929994984054507,
10.5972049430343));
#63540=CARTESIAN_POINT('Ctrl Pts',(-0.270756821184746,-2.13577279771527,
10.7083913628654));
#63541=CARTESIAN_POINT('Ctrl Pts',(1.64817793797518,-1.38501096239512,10.8195777826966));
#63542=CARTESIAN_POINT('Ctrl Pts',(2.0571630907777,0.634330397736036,10.9307642025277));
#63543=CARTESIAN_POINT('Ctrl Pts',(0.58197770073898,2.07288432925282,11.0419506223589));
#63544=CARTESIAN_POINT('Ctrl Pts',(-1.42685805211597,1.61204019596003,11.1531370421901));
#63545=CARTESIAN_POINT('Ctrl Pts',(-2.12761151034289,-0.324461171008946,
11.2643234620212));
#63546=CARTESIAN_POINT('Ctrl Pts',(-0.881342614057178,-1.96574134576644,
11.3755098818524));
#63547=CARTESIAN_POINT('Ctrl Pts',(1.17620974724197,-1.80236812191326,11.4866963016836));
#63548=CARTESIAN_POINT('Ctrl Pts',(1.82356548323819,-0.598586618003602,
11.560820581571));
#63549=CARTESIAN_POINT('Ctrl Pts',(1.82115221868229,0.00725425160419088,
11.5978827215147));
#63550=CARTESIAN_POINT('Ctrl Pts',(-0.861525859670525,1.75382131162755,
-1.38777878078145E-16));
#63551=CARTESIAN_POINT('Ctrl Pts',(-1.44496782441849,1.46721837385112,0.0370621399437207));
#63552=CARTESIAN_POINT('Ctrl Pts',(-2.29323624142731,0.270948940037977,
0.111186419831162));
#63553=CARTESIAN_POINT('Ctrl Pts',(-1.4690228053469,-1.78453568564088,0.222372839662325));
#63554=CARTESIAN_POINT('Ctrl Pts',(0.702798023147504,-2.19964250335881,
0.333559259493488));
#63555=CARTESIAN_POINT('Ctrl Pts',(2.22983948348091,-0.602620646924488,
0.44474567932465));
#63556=CARTESIAN_POINT('Ctrl Pts',(1.71476659751129,1.54790339194469,0.555932099155814));
#63557=CARTESIAN_POINT('Ctrl Pts',(-0.371377304572895,2.2797075413722,0.667118518986976));
#63558=CARTESIAN_POINT('Ctrl Pts',(-2.11718147056775,0.923606631345987,
0.778304938818138));
#63559=CARTESIAN_POINT('Ctrl Pts',(-1.92363015131696,-1.2787712372945,0.889491358649302));
#63560=CARTESIAN_POINT('Ctrl Pts',(0.0320890232727887,-2.30962717925356,
1.00067777848046));
#63561=CARTESIAN_POINT('Ctrl Pts',(1.95839267869742,-1.22482325334233,1.11186419831163));
#63562=CARTESIAN_POINT('Ctrl Pts',(2.09073448897961,0.982002812028443,1.22305061814279));
#63563=CARTESIAN_POINT('Ctrl Pts',(0.3078671242282,2.28925546628532,1.33423703797395));
#63564=CARTESIAN_POINT('Ctrl Pts',(-1.75701689972769,1.49945932314417,1.44542345780511));
#63565=CARTESIAN_POINT('Ctrl Pts',(-2.21239878427269,-0.663911091192784,
1.55660987763628));
#63566=CARTESIAN_POINT('Ctrl Pts',(-0.641126576885465,-2.21910779030204,
1.66779629746744));
#63567=CARTESIAN_POINT('Ctrl Pts',(1.51744495713052,-1.74150671579767,1.7789827172986));
#63568=CARTESIAN_POINT('Ctrl Pts',(2.28597130487397,0.331390712847842,1.89016913712977));
#63569=CARTESIAN_POINT('Ctrl Pts',(0.960448643749269,2.10071953052146,2.00135555696093));
#63570=CARTESIAN_POINT('Ctrl Pts',(-1.24488658037438,1.94569829998722,2.11254197679209));
#63571=CARTESIAN_POINT('Ctrl Pts',(-2.30985172178094,0.00833292063536468,
2.22372839662325));
#63572=CARTESIAN_POINT('Ctrl Pts',(-1.2588924584139,-1.93666572611094,2.33491481645442));
#63573=CARTESIAN_POINT('Ctrl Pts',(0.945266903418065,-2.10759457362527,
2.44610123628558));
#63574=CARTESIAN_POINT('Ctrl Pts',(2.28352077714336,-0.347875342430591,
2.55728765611674));
#63575=CARTESIAN_POINT('Ctrl Pts',(1.52997054850621,1.73051278744978,2.6684740759479));
#63576=CARTESIAN_POINT('Ctrl Pts',(-0.625099077306038,2.22367613142842,
2.77966049577907));
#63577=CARTESIAN_POINT('Ctrl Pts',(-2.20755082977362,0.679855665342084,
2.89084691561023));
#63578=CARTESIAN_POINT('Ctrl Pts',(-1.76779024968342,-1.48674208393651,
3.00203333544139));
#63579=CARTESIAN_POINT('Ctrl Pts',(0.291342892527361,-2.29141958423335,
3.11321975527256));
#63580=CARTESIAN_POINT('Ctrl Pts',(2.08359330569799,-0.997057334412016,
3.22440617510372));
#63581=CARTESIAN_POINT('Ctrl Pts',(1.96718185643314,1.21065268979674,3.33559259493488));
#63582=CARTESIAN_POINT('Ctrl Pts',(0.0487464827201324,2.30935232741881,
3.44677901476604));
#63583=CARTESIAN_POINT('Ctrl Pts',(-1.91434278399063,1.29258504441778,3.55796543459721));
#63584=CARTESIAN_POINT('Ctrl Pts',(-2.12381100893932,-0.908246216603541,
3.66915185442837));
#63585=CARTESIAN_POINT('Ctrl Pts',(-0.38777621054007,-2.27708453998192,
3.78033827425954));
#63586=CARTESIAN_POINT('Ctrl Pts',(1.70347841995286,-1.56001463596674,3.89152469409069));
#63587=CARTESIAN_POINT('Ctrl Pts',(2.23427291426326,0.58609635407974,4.00271111392186));
#63588=CARTESIAN_POINT('Ctrl Pts',(0.718376487679439,2.19531765665651,4.11389753375301));
#63589=CARTESIAN_POINT('Ctrl Pts',(-1.45558396757891,1.79353274433565,4.22508395358419));
#63590=CARTESIAN_POINT('Ctrl Pts',(-2.29616635965357,-0.251205972206891,
4.33627037341534));
#63591=CARTESIAN_POINT('Ctrl Pts',(-1.03336074967814,-2.06582911991821,
4.44745679324651));
#63592=CARTESIAN_POINT('Ctrl Pts',(1.17604813820203,-1.98806317010017,4.55864321307767));
#63593=CARTESIAN_POINT('Ctrl Pts',(2.30814590995695,-0.0891451065749571,
4.66982963290884));
#63594=CARTESIAN_POINT('Ctrl Pts',(1.32588189186442,1.89143374203362,4.78101605273999));
#63595=CARTESIAN_POINT('Ctrl Pts',(-0.870947461077787,2.1393772252035,4.89220247257116));
#63596=CARTESIAN_POINT('Ctrl Pts',(-2.26995115459196,0.427558355600586,
5.00338889240232));
#63597=CARTESIAN_POINT('Ctrl Pts',(-1.58958111120973,-1.67592251687317,
5.11457531223348));
#63598=CARTESIAN_POINT('Ctrl Pts',(0.546914192237968,-2.24418565586851,
5.22576173206465));
#63599=CARTESIAN_POINT('Ctrl Pts',(2.1824123683356,-0.756677372605439,5.33694815189581));
#63600=CARTESIAN_POINT('Ctrl Pts',(1.81872613351991,1.4239802115651,5.44813457172697));
#63601=CARTESIAN_POINT('Ctrl Pts',(-0.210992142997687,2.30021014415434,
5.55932099155813));
#63602=CARTESIAN_POINT('Ctrl Pts',(-2.04743246287144,1.06934779265563,5.67050741138931));
#63603=CARTESIAN_POINT('Ctrl Pts',(-2.00833582118916,-1.14108352937273,
5.78169383122044));
#63604=CARTESIAN_POINT('Ctrl Pts',(-0.129516437895867,-2.30623283386393,
5.89288025105164));
#63605=CARTESIAN_POINT('Ctrl Pts',(1.86794562143574,-1.35877280920554,6.00406667088277));
#63606=CARTESIAN_POINT('Ctrl Pts',(2.15428845280213,0.83338205752262,6.11525309071395));
#63607=CARTESIAN_POINT('Ctrl Pts',(0.467209600008474,2.26212280421227,6.22643951054511));
#63608=CARTESIAN_POINT('Ctrl Pts',(-1.64785351575852,1.61866092257753,6.33762593037627));
#63609=CARTESIAN_POINT('Ctrl Pts',(-2.25341132081031,-0.507564587930634,
6.44881235020743));
#63610=CARTESIAN_POINT('Ctrl Pts',(-0.794746594271866,-2.1688389157728,
6.55999877003859));
#63611=CARTESIAN_POINT('Ctrl Pts',(1.39194049181108,-1.84336270411821,6.67118518986976));
#63612=CARTESIAN_POINT('Ctrl Pts',(2.30354969961477,0.170713716736379,6.78237160970093));
#63613=CARTESIAN_POINT('Ctrl Pts',(1.1050074456459,2.02840896683692,6.89355802953208));
#63614=CARTESIAN_POINT('Ctrl Pts',(-1.10576956804586,2.02799360306213,7.00474444936325));
#63615=CARTESIAN_POINT('Ctrl Pts',(-2.30361368483253,0.169848116649841,
7.11593086919441));
#63616=CARTESIAN_POINT('Ctrl Pts',(-1.39124772661127,-1.84388561328419,
7.22711728902557));
#63617=CARTESIAN_POINT('Ctrl Pts',(0.795561506911461,-2.16854012653626,
7.33830370885674));
#63618=CARTESIAN_POINT('Ctrl Pts',(2.25360188555757,-0.506717804195071,
7.44949012868789));
#63619=CARTESIAN_POINT('Ctrl Pts',(1.64724516703786,1.61928001017393,7.56067654851907));
#63620=CARTESIAN_POINT('Ctrl Pts',(-0.468059588377044,2.26194708457211,
7.67186296835021));
#63621=CARTESIAN_POINT('Ctrl Pts',(-2.154601454596,0.832572497460946,7.78304938818139));
#63622=CARTESIAN_POINT('Ctrl Pts',(-1.8674349134348,-1.35947461755279,7.89423580801255));
#63623=CARTESIAN_POINT('Ctrl Pts',(0.130383025010703,-2.30618400359892,
8.00542222784371));
#63624=CARTESIAN_POINT('Ctrl Pts',(2.00876445601631,-1.14032879114536,8.11660864767487));
#63625=CARTESIAN_POINT('Ctrl Pts',(2.04703049732954,1.07011706590215,8.22779506750604));
#63626=CARTESIAN_POINT('Ctrl Pts',(0.210127794931219,2.30028926472067,8.3389814873372));
#63627=CARTESIAN_POINT('Ctrl Pts',(-1.81926108372479,1.42329670163983,8.45016790716836));
#63628=CARTESIAN_POINT('Ctrl Pts',(-2.18212788319439,-0.757497388391501,
8.56135432699953));
#63629=CARTESIAN_POINT('Ctrl Pts',(-0.546070872270014,-2.24439100726275,
8.67254074683069));
#63630=CARTESIAN_POINT('Ctrl Pts',(1.59021074792356,-1.67532509350284,8.78372716666185));
#63631=CARTESIAN_POINT('Ctrl Pts',(2.26979033427429,0.428411288796547,8.89491358649301));
#63632=CARTESIAN_POINT('Ctrl Pts',(0.870143500653468,2.13970434291613,9.00610000632417));
#63633=CARTESIAN_POINT('Ctrl Pts',(-1.32659252698235,1.89093539309814,9.11728642615534));
#63634=CARTESIAN_POINT('Ctrl Pts',(-2.30811225247311,-0.0900124183420705,
9.2284728459865));
#63635=CARTESIAN_POINT('Ctrl Pts',(-1.17530100973675,-1.98850493915805,
9.33965926581767));
#63636=CARTESIAN_POINT('Ctrl Pts',(1.03413692781901,-2.06544068631896,9.45084568564882));
#63637=CARTESIAN_POINT('Ctrl Pts',(2.29626061120593,-0.250343120523647,
9.56203210547999));
#63638=CARTESIAN_POINT('Ctrl Pts',(1.45490988438074,1.79407953322179,9.67321852531115));
#63639=CARTESIAN_POINT('Ctrl Pts',(-0.719201283577143,2.19504763615053,
9.78440494514231));
#63640=CARTESIAN_POINT('Ctrl Pts',(-2.2344931264651,0.585256616254353,9.89559136497349));
#63641=CARTESIAN_POINT('Ctrl Pts',(-1.70289184396906,-1.56065436285928,
10.0067777848046));
#63642=CARTESIAN_POINT('Ctrl Pts',(0.388631330803272,-2.27693917494037,
10.1179642046358));
#63643=CARTESIAN_POINT('Ctrl Pts',(2.1241530878674,-0.907447137301155,10.229150624467));
#63644=CARTESIAN_POINT('Ctrl Pts',(1.91385514681521,1.29330245229283,10.3403370442981));
#63645=CARTESIAN_POINT('Ctrl Pts',(-0.0496108271125438,2.30933734912719,
10.4515234641293));
#63646=CARTESIAN_POINT('Ctrl Pts',(-1.96764314760194,1.20990674417448,10.5627098839605));
#63647=CARTESIAN_POINT('Ctrl Pts',(-2.08320610464741,-0.997827509202423,
10.6738963037916));
#63648=CARTESIAN_POINT('Ctrl Pts',(-0.290505442625618,-2.29155305943203,
10.7850827236228));
#63649=CARTESIAN_POINT('Ctrl Pts',(1.7683937169233,-1.48603171255794,10.8962691434539));
#63650=CARTESIAN_POINT('Ctrl Pts',(2.20720967111538,0.680597564112484,11.0074555632851));
#63651=CARTESIAN_POINT('Ctrl Pts',(0.624426335084105,2.22407759459687,11.1186419831163));
#63652=CARTESIAN_POINT('Ctrl Pts',(-1.53093107010227,1.72962013887028,11.2298284029474));
#63653=CARTESIAN_POINT('Ctrl Pts',(-2.28279649924591,-0.348126912135875,
11.3410148227786));
#63654=CARTESIAN_POINT('Ctrl Pts',(-0.945626503816835,-2.10911975270116,
11.4522012426097));
#63655=CARTESIAN_POINT('Ctrl Pts',(1.26200083066393,-1.93383031585166,11.5633876624409));
#63656=CARTESIAN_POINT('Ctrl Pts',(1.95657378287586,-0.642246683396576,
11.6375119423284));
#63657=CARTESIAN_POINT('Ctrl Pts',(1.95398449819998,0.0077833665056624,
11.6745740822721));
#63658=CARTESIAN_POINT('Ctrl Pts',(-1.95093054978418,-0.000550606481354719,
10.6241303078758));
#63659=CARTESIAN_POINT('Ctrl Pts',(-1.95166977968097,-0.292567552961119,
10.640718973181));
#63660=CARTESIAN_POINT('Ctrl Pts',(-1.89027401228485,-0.584289311968449,
10.6573076384863));
#63661=CARTESIAN_POINT('Ctrl Pts',(-1.7651621681362,-0.845492725344543,
10.6738963037916));
#63662=CARTESIAN_POINT('Ctrl Pts',(-1.48563921730681,-1.42906935927896,
10.7109584437353));
#63663=CARTESIAN_POINT('Ctrl Pts',(-0.888072329966215,-1.8603112093555,
10.7480205836791));
#63664=CARTESIAN_POINT('Ctrl Pts',(-0.246139026371096,-1.94167857658142,
10.7850827236228));
#63665=CARTESIAN_POINT('Ctrl Pts',(0.395794277224022,-2.02304594380734,
10.8221448635665));
#63666=CARTESIAN_POINT('Ctrl Pts',(1.08209399707366,-1.75453882818264,10.8592070035102));
#63667=CARTESIAN_POINT('Ctrl Pts',(1.49837984936383,-1.25918039092522,10.8962691434539));
#63668=CARTESIAN_POINT('Ctrl Pts',(1.91466570165399,-0.763821953667804,
10.9333312833977));
#63669=CARTESIAN_POINT('Ctrl Pts',(2.06093768638468,-0.041612194777677,
10.9703934233414));
#63670=CARTESIAN_POINT('Ctrl Pts',(1.87027645607817,0.576739356414784,11.0074555632851));
#63671=CARTESIAN_POINT('Ctrl Pts',(1.80418088670294,0.791100177355746,11.0203037088567));
#63672=CARTESIAN_POINT('Ctrl Pts',(1.69759382901609,0.992979671982257,11.0331518544284));
#63673=CARTESIAN_POINT('Ctrl Pts',(1.56057659382855,1.17255425406022,11.046));
#63674=CARTESIAN_POINT('Ctrl Pts',(-0.9055496143049,-1.2679201530598,4.59701721133854E-17));
#63675=CARTESIAN_POINT('Ctrl Pts',(-0.937460871048188,-1.25085822491965,
4.11134559556874E-17));
#63676=CARTESIAN_POINT('Ctrl Pts',(-0.968677330061127,-1.23263760516135,
2.44937731663795E-16));
#63677=CARTESIAN_POINT('Ctrl Pts',(-0.999128467894991,-1.21327242330634,
1.95156391047391E-16));
#63678=CARTESIAN_POINT('Ctrl Pts',(-1.04916478169554,-1.18145218981002,
1.19833509668E-16));
#63679=CARTESIAN_POINT('Ctrl Pts',(-1.09713600671012,-1.14654455097205,
1.20483738925504E-16));
#63680=CARTESIAN_POINT('Ctrl Pts',(-1.14296368523792,-1.10887020140839,
3.46944695195361E-17));
#63681=CARTESIAN_POINT('Ctrl Pts',(-1.1691715546085,-1.08732504652154,-1.4366579135275E-17));
#63682=CARTESIAN_POINT('Ctrl Pts',(-1.19467812556179,-1.06487409533188,
1.54611493479508E-16));
#63683=CARTESIAN_POINT('Ctrl Pts',(-1.21946596262297,-1.04157045589269,
1.28369537222284E-16));
#63684=CARTESIAN_POINT('Ctrl Pts',(-1.23288807387334,-1.02895200756582,
1.14160049906282E-16));
#63685=CARTESIAN_POINT('Ctrl Pts',(-1.24610308792281,-1.01607950194371,
2.35779340588765E-16));
#63686=CARTESIAN_POINT('Ctrl Pts',(-1.25908578368524,-1.0029839550804,2.28983498828939E-16));
#63687=CARTESIAN_POINT('Ctrl Pts',(-1.30296735026586,-0.95872095130156,
2.06013524941215E-16));
#63688=CARTESIAN_POINT('Ctrl Pts',(-1.34424080059494,-0.911874911049719,
3.41092537496216E-16));
#63689=CARTESIAN_POINT('Ctrl Pts',(-1.3828175432908,-0.862794893107178,
2.15105711021124E-16));
#63690=CARTESIAN_POINT('Ctrl Pts',(-1.41246270387874,-0.825078255778903,
1.18288316865636E-16));
#63691=CARTESIAN_POINT('Ctrl Pts',(-1.44051505756546,-0.786041114269597,
-3.41744083773187E-17));
#63692=CARTESIAN_POINT('Ctrl Pts',(-1.46692433972057,-0.745823635123971,
-2.77555756156289E-17));
#63693=CARTESIAN_POINT('Ctrl Pts',(-1.479951210132,-0.725985614308893,-2.45893667770833E-17));
#63694=CARTESIAN_POINT('Ctrl Pts',(-1.49257814628919,-0.705860181165347,
1.12314029669873E-16));
#63695=CARTESIAN_POINT('Ctrl Pts',(-1.50479813274716,-0.685463000140721,
1.31838984174237E-16));
#63696=CARTESIAN_POINT('Ctrl Pts',(-1.51107691151866,-0.674982678607113,
1.41871145034493E-16));
#63697=CARTESIAN_POINT('Ctrl Pts',(-1.51724344631134,-0.664438579506566,
2.39743182585592E-16));
#63698=CARTESIAN_POINT('Ctrl Pts',(-1.52329612440982,-0.653835068968427,
2.42861286636753E-16));
#63699=CARTESIAN_POINT('Ctrl Pts',(-1.55541704658302,-0.597563360607725,
2.59408734877987E-16));
#63700=CARTESIAN_POINT('Ctrl Pts',(-1.58434358367058,-0.539605423501723,
2.32306933354682E-17));
#63701=CARTESIAN_POINT('Ctrl Pts',(-1.60998194797531,-0.480314579840224,
1.38777878078145E-17));
#63702=CARTESIAN_POINT('Ctrl Pts',(-1.63611695660561,-0.419875204988797,
4.34370584461709E-18));
#63703=CARTESIAN_POINT('Ctrl Pts',(-1.65883591999594,-0.358049987819819,
-3.99522282745635E-16));
#63704=CARTESIAN_POINT('Ctrl Pts',(-1.67800508733892,-0.295172269836945,
-4.02455846426619E-16));
#63705=CARTESIAN_POINT('Ctrl Pts',(-1.69036857863681,-0.254618180804147,
-4.04347899868101E-16));
#63706=CARTESIAN_POINT('Ctrl Pts',(-1.70125468815875,-0.21362546632645,
2.10692284276142E-16));
#63707=CARTESIAN_POINT('Ctrl Pts',(-1.71061789501208,-0.172277279535232,
2.22044604925031E-16));
#63708=CARTESIAN_POINT('Ctrl Pts',(-1.71585060492304,-0.149169484288187,
2.28388948449886E-16));
#63709=CARTESIAN_POINT('Ctrl Pts',(-1.72060753217063,-0.125950592727189,
-7.81124113857471E-17));
#63710=CARTESIAN_POINT('Ctrl Pts',(-1.72487954070067,-0.102634681883505,
-6.93889390390723E-17));
#63711=CARTESIAN_POINT('Ctrl Pts',(-1.72700542719079,-0.0910319475914671,
-6.50478634353357E-17));
#63712=CARTESIAN_POINT('Ctrl Pts',(-1.7290114810898,-0.0794035343790101,
3.2530658909822E-16));
#63713=CARTESIAN_POINT('Ctrl Pts',(-1.73089565945358,-0.0677563287869385,
3.05311331771918E-16));
#63714=CARTESIAN_POINT('Ctrl Pts',(-1.74172479313661,-0.000815136373784872,
1.90390516006322E-16));
#63715=CARTESIAN_POINT('Ctrl Pts',(-1.74848828323664,0.0664709663887247,
1.66332759660732E-17));
#63716=CARTESIAN_POINT('Ctrl Pts',(-1.75106678678907,0.133744024330042,
0.));
#63717=CARTESIAN_POINT('Ctrl Pts',(-1.75197767455289,0.157509050853062,
-5.87590718476407E-18));
#63718=CARTESIAN_POINT('Ctrl Pts',(-1.75236592486458,0.181272742240003,
-1.43574718418596E-16));
#63719=CARTESIAN_POINT('Ctrl Pts',(-1.75222496230419,0.20502014676713,-1.52655665885959E-16));
#63720=CARTESIAN_POINT('Ctrl Pts',(-1.75184009030703,0.269858008556557,
-1.89868827307373E-16));
#63721=CARTESIAN_POINT('Ctrl Pts',(-1.74751402866387,0.334573792851957,
-3.30194805135327E-16));
#63722=CARTESIAN_POINT('Ctrl Pts',(-1.7394637798186,0.398932034828451,-3.60822483003176E-16));
#63723=CARTESIAN_POINT('Ctrl Pts',(-1.73512917103287,0.433585348839861,
-3.77313774654407E-16));
#63724=CARTESIAN_POINT('Ctrl Pts',(-1.72971393872322,0.468135193807322,
-2.30290250750647E-16));
#63725=CARTESIAN_POINT('Ctrl Pts',(-1.72324590502527,0.502545438383202,
-2.22044604925031E-16));
#63726=CARTESIAN_POINT('Ctrl Pts',(-1.71875224847293,0.526451903350239,
-2.16315955056648E-16));
#63727=CARTESIAN_POINT('Ctrl Pts',(-1.71375034317529,0.550290993458765,
-1.09112752506388E-16));
#63728=CARTESIAN_POINT('Ctrl Pts',(-1.70824837476028,0.574050543226345,
-1.11022302462516E-16));
#63729=CARTESIAN_POINT('Ctrl Pts',(-1.70556019910987,0.585659087356796,
-1.11955278682682E-16));
#63730=CARTESIAN_POINT('Ctrl Pts',(-1.70275214211861,0.597250589985584,
-1.86923780482983E-17));
#63731=CARTESIAN_POINT('Ctrl Pts',(-1.69982665236451,0.608817432227434,
-2.77555756156289E-17));
#63732=CARTESIAN_POINT('Ctrl Pts',(-1.68323412399998,0.674421202576402,
-7.91594003935956E-17));
#63733=CARTESIAN_POINT('Ctrl Pts',(-1.6629277813761,0.739001412074313,-4.05964646411352E-16));
#63734=CARTESIAN_POINT('Ctrl Pts',(-1.63916833994428,0.802303176749866,
-3.88578058618805E-16));
#63735=CARTESIAN_POINT('Ctrl Pts',(-1.61488642929252,0.866996944840365,
-3.70809140417215E-16));
#63736=CARTESIAN_POINT('Ctrl Pts',(-1.58699772603761,0.930356288581554,
-4.09457680297508E-17));
#63737=CARTESIAN_POINT('Ctrl Pts',(-1.55572518982035,0.992113582996803,
0.));
#63738=CARTESIAN_POINT('Ctrl Pts',(-1.52416508821539,1.05443876420538,4.13222832434933E-17));
#63739=CARTESIAN_POINT('Ctrl Pts',(-1.48915832892389,1.11513327578217,-2.91589739144645E-16));
#63740=CARTESIAN_POINT('Ctrl Pts',(-1.45088203376165,1.17391247934435,-2.77555756156289E-16));
#63741=CARTESIAN_POINT('Ctrl Pts',(-1.43586030613212,1.19698067814596,-2.72048047818399E-16));
#63742=CARTESIAN_POINT('Ctrl Pts',(-1.42033446520901,1.21975369583959,-2.46829292445535E-16));
#63743=CARTESIAN_POINT('Ctrl Pts',(-1.40431321996707,1.24221341255695,-2.22044604925031E-16));
#63744=CARTESIAN_POINT('Ctrl Pts',(-1.39827097600966,1.25068385824148,-2.12697320981403E-16));
#63745=CARTESIAN_POINT('Ctrl Pts',(-1.39215941512485,1.25910802930607,-2.5395452896005E-16));
#63746=CARTESIAN_POINT('Ctrl Pts',(-1.38598454691313,1.26747777400967,-2.4980018054066E-16));
#63747=CARTESIAN_POINT('Ctrl Pts',(-1.3431243018081,1.32557282918544,-2.20964521964367E-16));
#63748=CARTESIAN_POINT('Ctrl Pts',(-1.29714727100707,1.38114651172693,8.67497813555755E-17));
#63749=CARTESIAN_POINT('Ctrl Pts',(-1.24829449348075,1.43391808714502,5.55111512312578E-17));
#63750=CARTESIAN_POINT('Ctrl Pts',(-1.19933005104754,1.48681028483588,2.42011176187261E-17));
#63751=CARTESIAN_POINT('Ctrl Pts',(-1.14747626839011,1.53688856046327,-1.29713890200027E-16));
#63752=CARTESIAN_POINT('Ctrl Pts',(-1.09292624810297,1.58385401467225,-2.77555756156289E-17));
#63753=CARTESIAN_POINT('Ctrl Pts',(-1.03954323648884,1.62981471962349,7.20215071969156E-17));
#63754=CARTESIAN_POINT('Ctrl Pts',(-0.983577547054738,1.67279522220595,
1.33536308196711E-16));
#63755=CARTESIAN_POINT('Ctrl Pts',(-0.92517040004714,1.71248622994896,1.66533453693773E-16));
#63756=CARTESIAN_POINT('Ctrl Pts',(-0.904266808925204,1.72669141954621,
1.78342947445829E-16));
#63757=CARTESIAN_POINT('Ctrl Pts',(-0.883050159709791,1.74047492561567,
-1.31748417511445E-16));
#63758=CARTESIAN_POINT('Ctrl Pts',(-0.861525859670525,1.75382131162755,
-1.38777878078145E-16));
#63759=CARTESIAN_POINT('Origin',(0.,0.,0.));
#63760=CARTESIAN_POINT('Origin',(-0.866025403784439,-1.5,-4.));
#63761=CARTESIAN_POINT('',(-0.866025403784439,-1.5,-4.));
#63762=CARTESIAN_POINT('',(0.866025403784439,-1.5,-4.));
#63763=CARTESIAN_POINT('',(-0.43301270189222,-1.5,-4.));
#63764=CARTESIAN_POINT('',(-0.866025403784439,-1.5,-2.));
#63765=CARTESIAN_POINT('',(-0.866025403784439,-1.5,-4.));
#63766=CARTESIAN_POINT('',(0.866025403784439,-1.5,-2.));
#63767=CARTESIAN_POINT('',(-0.866025403784439,-1.5,-2.));
#63768=CARTESIAN_POINT('',(0.866025403784439,-1.5,-4.));
#63769=CARTESIAN_POINT('Origin',(-1.73205080756888,2.12115047744981E-16,
-4.));
#63770=CARTESIAN_POINT('',(-1.73205080756888,2.12115047744981E-16,-4.));
#63771=CARTESIAN_POINT('',(-1.51554445662277,-0.375,-4.));
#63772=CARTESIAN_POINT('',(-1.73205080756888,2.77555756156289E-16,-2.));
#63773=CARTESIAN_POINT('',(-1.73205080756888,2.12115047744981E-16,-4.));
#63774=CARTESIAN_POINT('',(-1.73205080756888,2.12115047744981E-16,-2.));
#63775=CARTESIAN_POINT('Origin',(-0.866025403784438,1.5,-4.));
#63776=CARTESIAN_POINT('',(-0.866025403784438,1.5,-4.));
#63777=CARTESIAN_POINT('',(-1.08253175473055,1.125,-4.));
#63778=CARTESIAN_POINT('',(-0.866025403784438,1.5,-2.));
#63779=CARTESIAN_POINT('',(-0.866025403784438,1.5,-4.));
#63780=CARTESIAN_POINT('',(-0.866025403784438,1.5,-2.));
#63781=CARTESIAN_POINT('Origin',(0.866025403784439,1.5,-4.));
#63782=CARTESIAN_POINT('',(0.866025403784439,1.5,-4.));
#63783=CARTESIAN_POINT('',(0.43301270189222,1.5,-4.));
#63784=CARTESIAN_POINT('',(0.866025403784439,1.5,-2.));
#63785=CARTESIAN_POINT('',(0.866025403784439,1.5,-4.));
#63786=CARTESIAN_POINT('',(0.866025403784439,1.5,-2.));
#63787=CARTESIAN_POINT('Origin',(1.73205080756888,0.,-4.));
#63788=CARTESIAN_POINT('',(1.73205080756888,0.,-4.));
#63789=CARTESIAN_POINT('',(1.51554445662277,0.375,-4.));
#63790=CARTESIAN_POINT('',(1.73205080756888,0.,-2.));
#63791=CARTESIAN_POINT('',(1.73205080756888,0.,-4.));
#63792=CARTESIAN_POINT('',(1.73205080756888,0.,-2.));
#63793=CARTESIAN_POINT('Origin',(0.866025403784439,-1.5,-4.));
#63794=CARTESIAN_POINT('',(1.08253175473055,-1.125,-4.));
#63795=CARTESIAN_POINT('',(0.866025403784439,-1.5,-2.));
#63796=CARTESIAN_POINT('Origin',(0.,2.77555756156289E-16,-2.));
#63797=CARTESIAN_POINT('Origin',(0.,0.,0.));
#63798=CARTESIAN_POINT('',(-3.5,-4.28626379701574E-16,0.));
#63799=CARTESIAN_POINT('Origin',(0.,0.,0.));
#63800=CARTESIAN_POINT('Origin',(0.,0.,-4.));
#63801=CARTESIAN_POINT('',(-3.5,-4.28626379701574E-16,-4.));
#63802=CARTESIAN_POINT('',(-3.5,-4.28626379701574E-16,-4.));
#63803=CARTESIAN_POINT('Origin',(0.,0.,-4.));
#63804=CARTESIAN_POINT('Origin',(0.,0.,-4.));
#63805=CARTESIAN_POINT('Origin',(0.,0.,12.));
#63806=CARTESIAN_POINT('',(0.,0.,0.));
#63807=CARTESIAN_POINT('',(0.,0.,0.));
#63808=CARTESIAN_POINT('',(0.,0.,179.));
#63809=CARTESIAN_POINT('',(0.,0.,0.));
#63810=CARTESIAN_POINT('',(0.,0.,0.));
#63811=CARTESIAN_POINT('',(0.,0.,0.));
#63812=CARTESIAN_POINT('',(0.,0.,181.));
#63813=CARTESIAN_POINT('',(0.,0.,0.));
#63814=CARTESIAN_POINT('',(0.,0.,50.));
#63815=CARTESIAN_POINT('',(0.,0.,50.));
#63816=CARTESIAN_POINT('',(30.,0.,50.));
#63817=CARTESIAN_POINT('',(0.,0.,50.));
#63818=CARTESIAN_POINT('',(80.,0.,0.));
#63819=CARTESIAN_POINT('',(80.,0.,150.));
#63820=CARTESIAN_POINT('',(80.,0.,148.));
#63821=CARTESIAN_POINT('',(80.,0.,147.));
#63822=CARTESIAN_POINT('',(26.,0.,10.));
#63823=CARTESIAN_POINT('',(-32.,-32.,183.));
#63824=CARTESIAN_POINT('',(0.,0.,41.));
#63825=CARTESIAN_POINT('',(25.9807621135332,15.,50.));
#63826=CARTESIAN_POINT('',(15.,25.9807621135332,50.));
#63827=CARTESIAN_POINT('',(0.,30.,50.));
#63828=CARTESIAN_POINT('',(-15.,25.9807621135332,50.));
#63829=CARTESIAN_POINT('',(-25.9807621135332,15.,50.));
#63830=CARTESIAN_POINT('',(-30.,3.67394039744206E-15,50.));
#63831=CARTESIAN_POINT('',(-25.9807621135332,-15.,50.));
#63832=CARTESIAN_POINT('',(-15.,-25.9807621135332,50.));
#63833=CARTESIAN_POINT('',(-4.44089209850063E-15,-30.,50.));
#63834=CARTESIAN_POINT('',(15.,-25.9807621135332,50.));
#63835=CARTESIAN_POINT('',(25.9807621135332,-15.,50.));
#63836=CARTESIAN_POINT('',(0.,0.,170.));
#63837=CARTESIAN_POINT('',(0.,0.,170.));
#63838=CARTESIAN_POINT('',(30.,0.,170.));
#63839=CARTESIAN_POINT('',(25.9807621135332,15.,170.));
#63840=CARTESIAN_POINT('',(15.,25.9807621135332,170.));
#63841=CARTESIAN_POINT('',(0.,30.,170.));
#63842=CARTESIAN_POINT('',(-15.,25.9807621135332,170.));
#63843=CARTESIAN_POINT('',(-25.9807621135332,15.,170.));
#63844=CARTESIAN_POINT('',(-30.,3.67394039744206E-15,170.));
#63845=CARTESIAN_POINT('',(-25.9807621135332,-15.,170.));
#63846=CARTESIAN_POINT('',(-15.,-25.9807621135332,170.));
#63847=CARTESIAN_POINT('',(-4.44089209850063E-15,-30.,170.));
#63848=CARTESIAN_POINT('',(15.,-25.9807621135332,170.));
#63849=CARTESIAN_POINT('',(25.9807621135332,-15.,170.));
#63850=CARTESIAN_POINT('',(0.,0.,170.));
#63851=CARTESIAN_POINT('',(80.,0.,160.));
#63852=CARTESIAN_POINT('',(-32.,32.,183.));
#63853=CARTESIAN_POINT('',(32.,-32.,183.));
#63854=CARTESIAN_POINT('',(32.,32.,183.));
#63855=CARTESIAN_POINT('',(-32.,-32.,37.));
#63856=CARTESIAN_POINT('',(-32.,32.,37.));
#63857=CARTESIAN_POINT('',(32.,-32.,37.));
#63858=CARTESIAN_POINT('',(32.,32.,37.));
#63859=UNCERTAINTY_MEASURE_WITH_UNIT(LENGTH_MEASURE(0.01),#63899,
'DISTANCE_ACCURACY_VALUE',
'Maximum model space distance between geometric entities at asserted c
onnectivities');
#63860=UNCERTAINTY_MEASURE_WITH_UNIT(LENGTH_MEASURE(0.01),#63899,
'DISTANCE_ACCURACY_VALUE',
'Maximum model space distance between geometric entities at asserted c
onnectivities');
#63861=UNCERTAINTY_MEASURE_WITH_UNIT(LENGTH_MEASURE(0.01),#63899,
'DISTANCE_ACCURACY_VALUE',
'Maximum model space distance between geometric entities at asserted c
onnectivities');
#63862=UNCERTAINTY_MEASURE_WITH_UNIT(LENGTH_MEASURE(0.01),#63899,
'DISTANCE_ACCURACY_VALUE',
'Maximum model space distance between geometric entities at asserted c
onnectivities');
#63863=UNCERTAINTY_MEASURE_WITH_UNIT(LENGTH_MEASURE(0.01),#63899,
'DISTANCE_ACCURACY_VALUE',
'Maximum model space distance between geometric entities at asserted c
onnectivities');
#63864=UNCERTAINTY_MEASURE_WITH_UNIT(LENGTH_MEASURE(0.01),#63899,
'DISTANCE_ACCURACY_VALUE',
'Maximum model space distance between geometric entities at asserted c
onnectivities');
#63865=UNCERTAINTY_MEASURE_WITH_UNIT(LENGTH_MEASURE(0.01),#63899,
'DISTANCE_ACCURACY_VALUE',
'Maximum model space distance between geometric entities at asserted c
onnectivities');
#63866=UNCERTAINTY_MEASURE_WITH_UNIT(LENGTH_MEASURE(0.01),#63899,
'DISTANCE_ACCURACY_VALUE',
'Maximum model space distance between geometric entities at asserted c
onnectivities');
#63867=UNCERTAINTY_MEASURE_WITH_UNIT(LENGTH_MEASURE(0.01),#63899,
'DISTANCE_ACCURACY_VALUE',
'Maximum model space distance between geometric entities at asserted c
onnectivities');
#63868=UNCERTAINTY_MEASURE_WITH_UNIT(LENGTH_MEASURE(0.01),#63899,
'DISTANCE_ACCURACY_VALUE',
'Maximum model space distance between geometric entities at asserted c
onnectivities');
#63869=UNCERTAINTY_MEASURE_WITH_UNIT(LENGTH_MEASURE(0.01),#63899,
'DISTANCE_ACCURACY_VALUE',
'Maximum model space distance between geometric entities at asserted c
onnectivities');
#63870=UNCERTAINTY_MEASURE_WITH_UNIT(LENGTH_MEASURE(0.01),#63899,
'DISTANCE_ACCURACY_VALUE',
'Maximum model space distance between geometric entities at asserted c
onnectivities');
#63871=UNCERTAINTY_MEASURE_WITH_UNIT(LENGTH_MEASURE(0.01),#63899,
'DISTANCE_ACCURACY_VALUE',
'Maximum model space distance between geometric entities at asserted c
onnectivities');
#63872=UNCERTAINTY_MEASURE_WITH_UNIT(LENGTH_MEASURE(0.01),#63899,
'DISTANCE_ACCURACY_VALUE',
'Maximum model space distance between geometric entities at asserted c
onnectivities');
#63873=UNCERTAINTY_MEASURE_WITH_UNIT(LENGTH_MEASURE(0.01),#63899,
'DISTANCE_ACCURACY_VALUE',
'Maximum model space distance between geometric entities at asserted c
onnectivities');
#63874=UNCERTAINTY_MEASURE_WITH_UNIT(LENGTH_MEASURE(0.01),#63899,
'DISTANCE_ACCURACY_VALUE',
'Maximum model space distance between geometric entities at asserted c
onnectivities');
#63875=UNCERTAINTY_MEASURE_WITH_UNIT(LENGTH_MEASURE(0.01),#63899,
'DISTANCE_ACCURACY_VALUE',
'Maximum model space distance between geometric entities at asserted c
onnectivities');
#63876=UNCERTAINTY_MEASURE_WITH_UNIT(LENGTH_MEASURE(0.01),#63899,
'DISTANCE_ACCURACY_VALUE',
'Maximum model space distance between geometric entities at asserted c
onnectivities');
#63877=UNCERTAINTY_MEASURE_WITH_UNIT(LENGTH_MEASURE(0.01),#63899,
'DISTANCE_ACCURACY_VALUE',
'Maximum model space distance between geometric entities at asserted c
onnectivities');
#63878=UNCERTAINTY_MEASURE_WITH_UNIT(LENGTH_MEASURE(0.01),#63899,
'DISTANCE_ACCURACY_VALUE',
'Maximum model space distance between geometric entities at asserted c
onnectivities');
#63879=(
GEOMETRIC_REPRESENTATION_CONTEXT(3)
GLOBAL_UNCERTAINTY_ASSIGNED_CONTEXT((#63859))
GLOBAL_UNIT_ASSIGNED_CONTEXT((#63899,#63901,#63902))
REPRESENTATION_CONTEXT('','3D')
);
#63880=(
GEOMETRIC_REPRESENTATION_CONTEXT(3)
GLOBAL_UNCERTAINTY_ASSIGNED_CONTEXT((#63860))
GLOBAL_UNIT_ASSIGNED_CONTEXT((#63899,#63901,#63902))
REPRESENTATION_CONTEXT('','3D')
);
#63881=(
GEOMETRIC_REPRESENTATION_CONTEXT(3)
GLOBAL_UNCERTAINTY_ASSIGNED_CONTEXT((#63861))
GLOBAL_UNIT_ASSIGNED_CONTEXT((#63899,#63901,#63902))
REPRESENTATION_CONTEXT('','3D')
);
#63882=(
GEOMETRIC_REPRESENTATION_CONTEXT(3)
GLOBAL_UNCERTAINTY_ASSIGNED_CONTEXT((#63862))
GLOBAL_UNIT_ASSIGNED_CONTEXT((#63899,#63901,#63902))
REPRESENTATION_CONTEXT('','3D')
);
#63883=(
GEOMETRIC_REPRESENTATION_CONTEXT(3)
GLOBAL_UNCERTAINTY_ASSIGNED_CONTEXT((#63863))
GLOBAL_UNIT_ASSIGNED_CONTEXT((#63899,#63901,#63902))
REPRESENTATION_CONTEXT('','3D')
);
#63884=(
GEOMETRIC_REPRESENTATION_CONTEXT(3)
GLOBAL_UNCERTAINTY_ASSIGNED_CONTEXT((#63864))
GLOBAL_UNIT_ASSIGNED_CONTEXT((#63899,#63901,#63902))
REPRESENTATION_CONTEXT('','3D')
);
#63885=(
GEOMETRIC_REPRESENTATION_CONTEXT(3)
GLOBAL_UNCERTAINTY_ASSIGNED_CONTEXT((#63865))
GLOBAL_UNIT_ASSIGNED_CONTEXT((#63899,#63901,#63902))
REPRESENTATION_CONTEXT('','3D')
);
#63886=(
GEOMETRIC_REPRESENTATION_CONTEXT(3)
GLOBAL_UNCERTAINTY_ASSIGNED_CONTEXT((#63866))
GLOBAL_UNIT_ASSIGNED_CONTEXT((#63899,#63901,#63902))
REPRESENTATION_CONTEXT('','3D')
);
#63887=(
GEOMETRIC_REPRESENTATION_CONTEXT(3)
GLOBAL_UNCERTAINTY_ASSIGNED_CONTEXT((#63867))
GLOBAL_UNIT_ASSIGNED_CONTEXT((#63899,#63901,#63902))
REPRESENTATION_CONTEXT('','3D')
);
#63888=(
GEOMETRIC_REPRESENTATION_CONTEXT(3)
GLOBAL_UNCERTAINTY_ASSIGNED_CONTEXT((#63868))
GLOBAL_UNIT_ASSIGNED_CONTEXT((#63899,#63901,#63902))
REPRESENTATION_CONTEXT('','3D')
);
#63889=(
GEOMETRIC_REPRESENTATION_CONTEXT(3)
GLOBAL_UNCERTAINTY_ASSIGNED_CONTEXT((#63869))
GLOBAL_UNIT_ASSIGNED_CONTEXT((#63899,#63901,#63902))
REPRESENTATION_CONTEXT('','3D')
);
#63890=(
GEOMETRIC_REPRESENTATION_CONTEXT(3)
GLOBAL_UNCERTAINTY_ASSIGNED_CONTEXT((#63870))
GLOBAL_UNIT_ASSIGNED_CONTEXT((#63899,#63901,#63902))
REPRESENTATION_CONTEXT('','3D')
);
#63891=(
GEOMETRIC_REPRESENTATION_CONTEXT(3)
GLOBAL_UNCERTAINTY_ASSIGNED_CONTEXT((#63871))
GLOBAL_UNIT_ASSIGNED_CONTEXT((#63899,#63901,#63902))
REPRESENTATION_CONTEXT('','3D')
);
#63892=(
GEOMETRIC_REPRESENTATION_CONTEXT(3)
GLOBAL_UNCERTAINTY_ASSIGNED_CONTEXT((#63872))
GLOBAL_UNIT_ASSIGNED_CONTEXT((#63899,#63901,#63902))
REPRESENTATION_CONTEXT('','3D')
);
#63893=(
GEOMETRIC_REPRESENTATION_CONTEXT(3)
GLOBAL_UNCERTAINTY_ASSIGNED_CONTEXT((#63873))
GLOBAL_UNIT_ASSIGNED_CONTEXT((#63899,#63901,#63902))
REPRESENTATION_CONTEXT('','3D')
);
#63894=(
GEOMETRIC_REPRESENTATION_CONTEXT(3)
GLOBAL_UNCERTAINTY_ASSIGNED_CONTEXT((#63874))
GLOBAL_UNIT_ASSIGNED_CONTEXT((#63899,#63901,#63902))
REPRESENTATION_CONTEXT('','3D')
);
#63895=(
GEOMETRIC_REPRESENTATION_CONTEXT(3)
GLOBAL_UNCERTAINTY_ASSIGNED_CONTEXT((#63875))
GLOBAL_UNIT_ASSIGNED_CONTEXT((#63899,#63901,#63902))
REPRESENTATION_CONTEXT('','3D')
);
#63896=(
GEOMETRIC_REPRESENTATION_CONTEXT(3)
GLOBAL_UNCERTAINTY_ASSIGNED_CONTEXT((#63876))
GLOBAL_UNIT_ASSIGNED_CONTEXT((#63899,#63901,#63902))
REPRESENTATION_CONTEXT('','3D')
);
#63897=(
GEOMETRIC_REPRESENTATION_CONTEXT(3)
GLOBAL_UNCERTAINTY_ASSIGNED_CONTEXT((#63877))
GLOBAL_UNIT_ASSIGNED_CONTEXT((#63899,#63901,#63902))
REPRESENTATION_CONTEXT('','3D')
);
#63898=(
GEOMETRIC_REPRESENTATION_CONTEXT(3)
GLOBAL_UNCERTAINTY_ASSIGNED_CONTEXT((#63878))
GLOBAL_UNIT_ASSIGNED_CONTEXT((#63899,#63901,#63902))
REPRESENTATION_CONTEXT('','3D')
);
#63899=(
LENGTH_UNIT()
NAMED_UNIT(*)
SI_UNIT(.MILLI.,.METRE.)
);
#63900=(
LENGTH_UNIT()
NAMED_UNIT(*)
SI_UNIT($,.METRE.)
);
#63901=(
NAMED_UNIT(*)
PLANE_ANGLE_UNIT()
SI_UNIT($,.RADIAN.)
);
#63902=(
NAMED_UNIT(*)
SI_UNIT($,.STERADIAN.)
SOLID_ANGLE_UNIT()
);
#63903=SHAPE_DEFINITION_REPRESENTATION(#63922,#63994);
#63904=SHAPE_DEFINITION_REPRESENTATION(#63923,#63995);
#63905=SHAPE_DEFINITION_REPRESENTATION(#63924,#63996);
#63906=SHAPE_DEFINITION_REPRESENTATION(#63925,#63997);
#63907=SHAPE_DEFINITION_REPRESENTATION(#63926,#63998);
#63908=SHAPE_DEFINITION_REPRESENTATION(#63927,#63999);
#63909=SHAPE_DEFINITION_REPRESENTATION(#63928,#64000);
#63910=SHAPE_DEFINITION_REPRESENTATION(#63929,#64001);
#63911=SHAPE_DEFINITION_REPRESENTATION(#63930,#64002);
#63912=SHAPE_DEFINITION_REPRESENTATION(#63931,#64003);
#63913=SHAPE_DEFINITION_REPRESENTATION(#63932,#64004);
#63914=SHAPE_DEFINITION_REPRESENTATION(#63933,#64005);
#63915=SHAPE_DEFINITION_REPRESENTATION(#63934,#64006);
#63916=SHAPE_DEFINITION_REPRESENTATION(#63935,#64007);
#63917=SHAPE_DEFINITION_REPRESENTATION(#63936,#64008);
#63918=SHAPE_DEFINITION_REPRESENTATION(#63937,#64009);
#63919=SHAPE_DEFINITION_REPRESENTATION(#63938,#64010);
#63920=SHAPE_DEFINITION_REPRESENTATION(#63939,#64011);
#63921=SHAPE_DEFINITION_REPRESENTATION(#63940,#64012);
#63922=PRODUCT_DEFINITION_SHAPE('',$,#64014);
#63923=PRODUCT_DEFINITION_SHAPE('',$,#64015);
#63924=PRODUCT_DEFINITION_SHAPE('',$,#64016);
#63925=PRODUCT_DEFINITION_SHAPE('',$,#64017);
#63926=PRODUCT_DEFINITION_SHAPE('',$,#64018);
#63927=PRODUCT_DEFINITION_SHAPE('',$,#64019);
#63928=PRODUCT_DEFINITION_SHAPE('',$,#64020);
#63929=PRODUCT_DEFINITION_SHAPE('',$,#64021);
#63930=PRODUCT_DEFINITION_SHAPE('',$,#64022);
#63931=PRODUCT_DEFINITION_SHAPE('',$,#64023);
#63932=PRODUCT_DEFINITION_SHAPE('',$,#64024);
#63933=PRODUCT_DEFINITION_SHAPE('',$,#64025);
#63934=PRODUCT_DEFINITION_SHAPE('',$,#64026);
#63935=PRODUCT_DEFINITION_SHAPE('',$,#64027);
#63936=PRODUCT_DEFINITION_SHAPE('',$,#64028);
#63937=PRODUCT_DEFINITION_SHAPE('',$,#64029);
#63938=PRODUCT_DEFINITION_SHAPE('',$,#64030);
#63939=PRODUCT_DEFINITION_SHAPE('',$,#64031);
#63940=PRODUCT_DEFINITION_SHAPE('',$,#64032);
#63941=PRODUCT_DEFINITION_SHAPE($,$,#170);
#63942=PRODUCT_DEFINITION_SHAPE($,$,#171);
#63943=PRODUCT_DEFINITION_SHAPE($,$,#172);
#63944=PRODUCT_DEFINITION_SHAPE($,$,#173);
#63945=PRODUCT_DEFINITION_SHAPE($,$,#174);
#63946=PRODUCT_DEFINITION_SHAPE($,$,#175);
#63947=PRODUCT_DEFINITION_SHAPE($,$,#176);
#63948=PRODUCT_DEFINITION_SHAPE($,$,#177);
#63949=PRODUCT_DEFINITION_SHAPE($,$,#178);
#63950=PRODUCT_DEFINITION_SHAPE($,$,#179);
#63951=PRODUCT_DEFINITION_SHAPE($,$,#180);
#63952=PRODUCT_DEFINITION_SHAPE($,$,#181);
#63953=PRODUCT_DEFINITION_SHAPE($,$,#182);
#63954=PRODUCT_DEFINITION_SHAPE($,$,#183);
#63955=PRODUCT_DEFINITION_SHAPE($,$,#184);
#63956=PRODUCT_DEFINITION_SHAPE($,$,#185);
#63957=PRODUCT_DEFINITION_SHAPE($,$,#186);
#63958=PRODUCT_DEFINITION_SHAPE($,$,#187);
#63959=PRODUCT_DEFINITION_SHAPE($,$,#188);
#63960=PRODUCT_DEFINITION_SHAPE($,$,#189);
#63961=PRODUCT_DEFINITION_SHAPE($,$,#190);
#63962=PRODUCT_DEFINITION_SHAPE($,$,#191);
#63963=PRODUCT_DEFINITION_SHAPE($,$,#192);
#63964=PRODUCT_DEFINITION_SHAPE($,$,#193);
#63965=PRODUCT_DEFINITION_SHAPE($,$,#194);
#63966=PRODUCT_DEFINITION_SHAPE($,$,#195);
#63967=PRODUCT_DEFINITION_SHAPE($,$,#196);
#63968=PRODUCT_DEFINITION_SHAPE($,$,#197);
#63969=PRODUCT_DEFINITION_SHAPE($,$,#198);
#63970=PRODUCT_DEFINITION_SHAPE($,$,#199);
#63971=PRODUCT_DEFINITION_SHAPE($,$,#200);
#63972=PRODUCT_DEFINITION_SHAPE($,$,#201);
#63973=PRODUCT_DEFINITION_SHAPE($,$,#202);
#63974=PRODUCT_DEFINITION_SHAPE($,$,#203);
#63975=PRODUCT_DEFINITION_SHAPE($,$,#204);
#63976=PRODUCT_DEFINITION_SHAPE($,$,#205);
#63977=PRODUCT_DEFINITION_SHAPE($,$,#206);
#63978=PRODUCT_DEFINITION_SHAPE($,$,#207);
#63979=PRODUCT_DEFINITION_SHAPE($,$,#208);
#63980=PRODUCT_DEFINITION_SHAPE($,$,#209);
#63981=PRODUCT_DEFINITION_SHAPE($,$,#210);
#63982=PRODUCT_DEFINITION_SHAPE($,$,#211);
#63983=PRODUCT_DEFINITION_SHAPE($,$,#212);
#63984=PRODUCT_DEFINITION_SHAPE($,$,#213);
#63985=PRODUCT_DEFINITION_SHAPE($,$,#214);
#63986=PRODUCT_DEFINITION_SHAPE($,$,#215);
#63987=PRODUCT_DEFINITION_SHAPE($,$,#216);
#63988=PRODUCT_DEFINITION_SHAPE($,$,#217);
#63989=PRODUCT_DEFINITION_SHAPE($,$,#218);
#63990=PRODUCT_DEFINITION_SHAPE($,$,#219);
#63991=PRODUCT_DEFINITION_SHAPE($,$,#220);
#63992=PRODUCT_DEFINITION_SHAPE($,$,#221);
#63993=PRODUCT_DEFINITION_SHAPE($,$,#222);
#63994=SHAPE_REPRESENTATION('',(#15695,#16806,#16807,#16808,#16809,#16810,
#16811,#16812,#16813,#16814,#16815,#16816,#16817,#16818,#16819,#16820,#16821,
#16822,#16823,#16824,#16825,#16826,#16827,#16828,#16829,#16830,#16831,#16832,
#16833,#16834,#16835,#16836,#16837,#16838,#16839,#16840,#16841,#16842,#16843,
#16844,#16845,#16846,#16847,#16848,#16849,#16850,#16851,#16852,#16853,#16854,
#16855,#16856,#16857,#16858),#63879);
#63995=SHAPE_REPRESENTATION('',(#15696),#63880);
#63996=SHAPE_REPRESENTATION('',(#15752),#63881);
#63997=SHAPE_REPRESENTATION('',(#16184),#63882);
#63998=SHAPE_REPRESENTATION('',(#16268),#63883);
#63999=SHAPE_REPRESENTATION('',(#16277),#63884);
#64000=SHAPE_REPRESENTATION('',(#16286),#63885);
#64001=SHAPE_REPRESENTATION('',(#16297),#63886);
#64002=SHAPE_REPRESENTATION('',(#16304),#63887);
#64003=SHAPE_REPRESENTATION('',(#16511),#63888);
#64004=SHAPE_REPRESENTATION('',(#16520),#63889);
#64005=SHAPE_REPRESENTATION('',(#16531),#63890);
#64006=SHAPE_REPRESENTATION('',(#16583),#63891);
#64007=SHAPE_REPRESENTATION('',(#16620),#63892);
#64008=SHAPE_REPRESENTATION('',(#16634),#63893);
#64009=SHAPE_REPRESENTATION('',(#16648),#63894);
#64010=SHAPE_REPRESENTATION('',(#16651),#63895);
#64011=SHAPE_REPRESENTATION('',(#16743),#63896);
#64012=SHAPE_REPRESENTATION('',(#16752),#63897);
#64013=PRODUCT_DEFINITION_CONTEXT('part definition',#64072,'design');
#64014=PRODUCT_DEFINITION('MAS-310','MAS-310',#64033,#64013);
#64015=PRODUCT_DEFINITION('Guide housing','Guide housing',#64034,#64013);
#64016=PRODUCT_DEFINITION('Quill','Quill',#64035,#64013);
#64017=PRODUCT_DEFINITION('Spindle','Spindle',#64036,#64013);
#64018=PRODUCT_DEFINITION('Inner race spacer','Inner race spacer',#64037,
#64013);
#64019=PRODUCT_DEFINITION('Spindle thrust washer',
'Spindle thrust washer',#64038,#64013);
#64020=PRODUCT_DEFINITION('Spindle retaining ring',
'Spindle retaining ring',#64039,#64013);
#64021=PRODUCT_DEFINITION('Guide key','Guide key',#64040,#64013);
#64022=PRODUCT_DEFINITION('Feed screw','Feed screw',#64041,#64013);
#64023=PRODUCT_DEFINITION('Feed journal bushing','Feed journal bushing',
#64042,#64013);
#64024=PRODUCT_DEFINITION('Feed retaining ring','Feed retaining ring',#64043,
#64013);
#64025=PRODUCT_DEFINITION('Set screw M6x18','Set screw M6x18',#64044,#64013);
#64026=PRODUCT_DEFINITION('Bearing end cover','Bearing end cover',#64045,
#64013);
#64027=PRODUCT_DEFINITION('Inner race','Inner race',#64046,#64013);
#64028=PRODUCT_DEFINITION('Outer race','Outer race',#64047,#64013);
#64029=PRODUCT_DEFINITION('Bearing ball','Bearing ball',#64048,#64013);
#64030=PRODUCT_DEFINITION('Ball cage','Ball cage',#64049,#64013);
#64031=PRODUCT_DEFINITION('Feed thrust washer','Feed thrust washer',#64050,
#64013);
#64032=PRODUCT_DEFINITION('Socket head cap screw M4x12',
'Socket head cap screw M4x12',#64051,#64013);
#64033=PRODUCT_DEFINITION_FORMATION('',$,#64074);
#64034=PRODUCT_DEFINITION_FORMATION('',$,#64075);
#64035=PRODUCT_DEFINITION_FORMATION('',$,#64076);
#64036=PRODUCT_DEFINITION_FORMATION('',$,#64077);
#64037=PRODUCT_DEFINITION_FORMATION('',$,#64078);
#64038=PRODUCT_DEFINITION_FORMATION('',$,#64079);
#64039=PRODUCT_DEFINITION_FORMATION('',$,#64080);
#64040=PRODUCT_DEFINITION_FORMATION('',$,#64081);
#64041=PRODUCT_DEFINITION_FORMATION('',$,#64082);
#64042=PRODUCT_DEFINITION_FORMATION('',$,#64083);
#64043=PRODUCT_DEFINITION_FORMATION('',$,#64084);
#64044=PRODUCT_DEFINITION_FORMATION('',$,#64085);
#64045=PRODUCT_DEFINITION_FORMATION('',$,#64086);
#64046=PRODUCT_DEFINITION_FORMATION('',$,#64087);
#64047=PRODUCT_DEFINITION_FORMATION('',$,#64088);
#64048=PRODUCT_DEFINITION_FORMATION('',$,#64089);
#64049=PRODUCT_DEFINITION_FORMATION('',$,#64090);
#64050=PRODUCT_DEFINITION_FORMATION('',$,#64091);
#64051=PRODUCT_DEFINITION_FORMATION('',$,#64092);
#64052=PRODUCT_RELATED_PRODUCT_CATEGORY('MAS-310','MAS-310',(#64074));
#64053=PRODUCT_RELATED_PRODUCT_CATEGORY('Guide housing','Guide housing',
(#64075));
#64054=PRODUCT_RELATED_PRODUCT_CATEGORY('Quill','Quill',(#64076));
#64055=PRODUCT_RELATED_PRODUCT_CATEGORY('Spindle','Spindle',(#64077));
#64056=PRODUCT_RELATED_PRODUCT_CATEGORY('Inner race spacer',
'Inner race spacer',(#64078));
#64057=PRODUCT_RELATED_PRODUCT_CATEGORY('Spindle thrust washer',
'Spindle thrust washer',(#64079));
#64058=PRODUCT_RELATED_PRODUCT_CATEGORY('Spindle retaining ring',
'Spindle retaining ring',(#64080));
#64059=PRODUCT_RELATED_PRODUCT_CATEGORY('Guide key','Guide key',(#64081));
#64060=PRODUCT_RELATED_PRODUCT_CATEGORY('Feed screw','Feed screw',(#64082));
#64061=PRODUCT_RELATED_PRODUCT_CATEGORY('Feed journal bushing',
'Feed journal bushing',(#64083));
#64062=PRODUCT_RELATED_PRODUCT_CATEGORY('Feed retaining ring',
'Feed retaining ring',(#64084));
#64063=PRODUCT_RELATED_PRODUCT_CATEGORY('Set screw M6x18',
'Set screw M6x18',(#64085));
#64064=PRODUCT_RELATED_PRODUCT_CATEGORY('Bearing end cover',
'Bearing end cover',(#64086));
#64065=PRODUCT_RELATED_PRODUCT_CATEGORY('Inner race','Inner race',(#64087));
#64066=PRODUCT_RELATED_PRODUCT_CATEGORY('Outer race','Outer race',(#64088));
#64067=PRODUCT_RELATED_PRODUCT_CATEGORY('Bearing ball','Bearing ball',(#64089));
#64068=PRODUCT_RELATED_PRODUCT_CATEGORY('Ball cage','Ball cage',(#64090));
#64069=PRODUCT_RELATED_PRODUCT_CATEGORY('Feed thrust washer',
'Feed thrust washer',(#64091));
#64070=PRODUCT_RELATED_PRODUCT_CATEGORY('Socket head cap screw M4x12',
'Socket head cap screw M4x12',(#64092));
#64071=APPLICATION_PROTOCOL_DEFINITION('international standard',
'automotive_design',2009,#64072);
#64072=APPLICATION_CONTEXT(
'Core Data for Automotive Mechanical Design Process');
#64073=PRODUCT_CONTEXT('part definition',#64072,'mechanical');
#64074=PRODUCT('MAS-310','MAS-310',
'Independent30mm screw-fed quill/spindle unit with16mm straight tool s
ocket, radial set screw, native reusable open ball bearings, retained 
inner/outer race stacks, keyed quill guide and M12x1.75 fine feed. Ext
ernal moving drive and tool not included. Ideal cage orbital links; in
dividual ball spin, force and preload not simulated. No drilling capac
ity, runout, speed, torque, load, life or machine safety rating.',(#64073));
#64075=PRODUCT('Guide housing','Guide housing',$,(#64073));
#64076=PRODUCT('Quill','Quill',$,(#64073));
#64077=PRODUCT('Spindle','Spindle',$,(#64073));
#64078=PRODUCT('Inner race spacer','Inner race spacer',
'Inner race spacer',(#64073));
#64079=PRODUCT('Spindle thrust washer','Spindle thrust washer',$,(#64073));
#64080=PRODUCT('Spindle retaining ring','Spindle retaining ring',$,(#64073));
#64081=PRODUCT('Guide key','Guide key',$,(#64073));
#64082=PRODUCT('Feed screw','Feed screw','Feed screw',(#64073));
#64083=PRODUCT('Feed journal bushing','Feed journal bushing',$,(#64073));
#64084=PRODUCT('Feed retaining ring','Feed retaining ring',$,(#64073));
#64085=PRODUCT('Set screw M6x18','Set screw M6x18',$,(#64073));
#64086=PRODUCT('Bearing end cover','Bearing end cover',$,(#64073));
#64087=PRODUCT('Inner race','Inner race',$,(#64073));
#64088=PRODUCT('Outer race','Outer race',$,(#64073));
#64089=PRODUCT('Bearing ball','Bearing ball',$,(#64073));
#64090=PRODUCT('Ball cage','Ball cage',$,(#64073));
#64091=PRODUCT('Feed thrust washer','Feed thrust washer',$,(#64073));
#64092=PRODUCT('Socket head cap screw M4x12',
'Socket head cap screw M4x12',$,(#64073));
#64093=PRESENTATION_STYLE_ASSIGNMENT((#64106));
#64094=PRESENTATION_STYLE_ASSIGNMENT((#64107));
#64095=PRESENTATION_STYLE_ASSIGNMENT((#64108));
#64096=PRESENTATION_STYLE_ASSIGNMENT((#64109));
#64097=PRESENTATION_STYLE_ASSIGNMENT((#64110));
#64098=PRESENTATION_STYLE_ASSIGNMENT((#64111));
#64099=PRESENTATION_STYLE_ASSIGNMENT((#64112));
#64100=PRESENTATION_STYLE_ASSIGNMENT((#64113));
#64101=PRESENTATION_STYLE_ASSIGNMENT((#64114));
#64102=PRESENTATION_STYLE_ASSIGNMENT((#64115));
#64103=PRESENTATION_STYLE_ASSIGNMENT((#64116));
#64104=PRESENTATION_STYLE_ASSIGNMENT((#64117));
#64105=PRESENTATION_STYLE_ASSIGNMENT((#64118));
#64106=SURFACE_STYLE_USAGE(.BOTH.,#64119);
#64107=SURFACE_STYLE_USAGE(.BOTH.,#64120);
#64108=SURFACE_STYLE_USAGE(.BOTH.,#64121);
#64109=SURFACE_STYLE_USAGE(.BOTH.,#64122);
#64110=SURFACE_STYLE_USAGE(.BOTH.,#64123);
#64111=SURFACE_STYLE_USAGE(.BOTH.,#64124);
#64112=SURFACE_STYLE_USAGE(.BOTH.,#64125);
#64113=SURFACE_STYLE_USAGE(.BOTH.,#64126);
#64114=SURFACE_STYLE_USAGE(.BOTH.,#64127);
#64115=SURFACE_STYLE_USAGE(.BOTH.,#64128);
#64116=SURFACE_STYLE_USAGE(.BOTH.,#64129);
#64117=SURFACE_STYLE_USAGE(.BOTH.,#64130);
#64118=SURFACE_STYLE_USAGE(.BOTH.,#64131);
#64119=SURFACE_SIDE_STYLE('',(#64132));
#64120=SURFACE_SIDE_STYLE('',(#64133));
#64121=SURFACE_SIDE_STYLE('',(#64134));
#64122=SURFACE_SIDE_STYLE('',(#64135));
#64123=SURFACE_SIDE_STYLE('',(#64136));
#64124=SURFACE_SIDE_STYLE('',(#64137));
#64125=SURFACE_SIDE_STYLE('',(#64138));
#64126=SURFACE_SIDE_STYLE('',(#64139));
#64127=SURFACE_SIDE_STYLE('',(#64140));
#64128=SURFACE_SIDE_STYLE('',(#64141));
#64129=SURFACE_SIDE_STYLE('',(#64142));
#64130=SURFACE_SIDE_STYLE('',(#64143));
#64131=SURFACE_SIDE_STYLE('',(#64144));
#64132=SURFACE_STYLE_FILL_AREA(#64145);
#64133=SURFACE_STYLE_FILL_AREA(#64146);
#64134=SURFACE_STYLE_FILL_AREA(#64147);
#64135=SURFACE_STYLE_FILL_AREA(#64148);
#64136=SURFACE_STYLE_FILL_AREA(#64149);
#64137=SURFACE_STYLE_FILL_AREA(#64150);
#64138=SURFACE_STYLE_FILL_AREA(#64151);
#64139=SURFACE_STYLE_FILL_AREA(#64152);
#64140=SURFACE_STYLE_FILL_AREA(#64153);
#64141=SURFACE_STYLE_FILL_AREA(#64154);
#64142=SURFACE_STYLE_FILL_AREA(#64155);
#64143=SURFACE_STYLE_FILL_AREA(#64156);
#64144=SURFACE_STYLE_FILL_AREA(#64157);
#64145=FILL_AREA_STYLE('Steel - Satin',(#64158));
#64146=FILL_AREA_STYLE('Dark blue',(#64159));
#64147=FILL_AREA_STYLE('Light blue',(#64160));
#64148=FILL_AREA_STYLE('Spindle gray',(#64161));
#64149=FILL_AREA_STYLE('Light gray',(#64162));
#64150=FILL_AREA_STYLE('Gray',(#64163));
#64151=FILL_AREA_STYLE('Dark gray',(#64164));
#64152=FILL_AREA_STYLE('Charcoal',(#64165));
#64153=FILL_AREA_STYLE('Sky blue',(#64166));
#64154=FILL_AREA_STYLE('Inner race gray',(#64167));
#64155=FILL_AREA_STYLE('Outer race gray',(#64168));
#64156=FILL_AREA_STYLE('Ball light gray',(#64169));
#64157=FILL_AREA_STYLE('Cage dark gray',(#64170));
#64158=FILL_AREA_STYLE_COLOUR('Steel - Satin',#64171);
#64159=FILL_AREA_STYLE_COLOUR('Dark blue',#64172);
#64160=FILL_AREA_STYLE_COLOUR('Light blue',#64173);
#64161=FILL_AREA_STYLE_COLOUR('Spindle gray',#64174);
#64162=FILL_AREA_STYLE_COLOUR('Light gray',#64175);
#64163=FILL_AREA_STYLE_COLOUR('Gray',#64176);
#64164=FILL_AREA_STYLE_COLOUR('Dark gray',#64177);
#64165=FILL_AREA_STYLE_COLOUR('Charcoal',#64178);
#64166=FILL_AREA_STYLE_COLOUR('Sky blue',#64179);
#64167=FILL_AREA_STYLE_COLOUR('Inner race gray',#64180);
#64168=FILL_AREA_STYLE_COLOUR('Outer race gray',#64181);
#64169=FILL_AREA_STYLE_COLOUR('Ball light gray',#64182);
#64170=FILL_AREA_STYLE_COLOUR('Cage dark gray',#64183);
#64171=COLOUR_RGB('Steel - Satin',0.627450980392157,0.627450980392157,0.627450980392157);
#64172=COLOUR_RGB('Dark blue',0.0901960784313725,0.270588235294118,0.513725490196078);
#64173=COLOUR_RGB('Light blue',0.662745098039216,0.831372549019608,0.949019607843137);
#64174=COLOUR_RGB('Spindle gray',0.576470588235294,0.615686274509804,0.666666666666667);
#64175=COLOUR_RGB('Light gray',0.725490196078431,0.752941176470588,0.792156862745098);
#64176=COLOUR_RGB('Gray',0.407843137254902,0.447058823529412,0.498039215686275);
#64177=COLOUR_RGB('Dark gray',0.250980392156863,0.282352941176471,0.32156862745098);
#64178=COLOUR_RGB('Charcoal',0.164705882352941,0.184313725490196,0.211764705882353);
#64179=COLOUR_RGB('Sky blue',0.317647058823529,0.686274509803922,0.890196078431372);
#64180=COLOUR_RGB('Inner race gray',0.576470588235294,0.615686274509804,
0.666666666666667);
#64181=COLOUR_RGB('Outer race gray',0.407843137254902,0.447058823529412,
0.498039215686275);
#64182=COLOUR_RGB('Ball light gray',0.784313725490196,0.815686274509804,
0.854901960784314);
#64183=COLOUR_RGB('Cage dark gray',0.250980392156863,0.282352941176471,
0.32156862745098);
ENDSEC;
END-ISO-10303-21;
